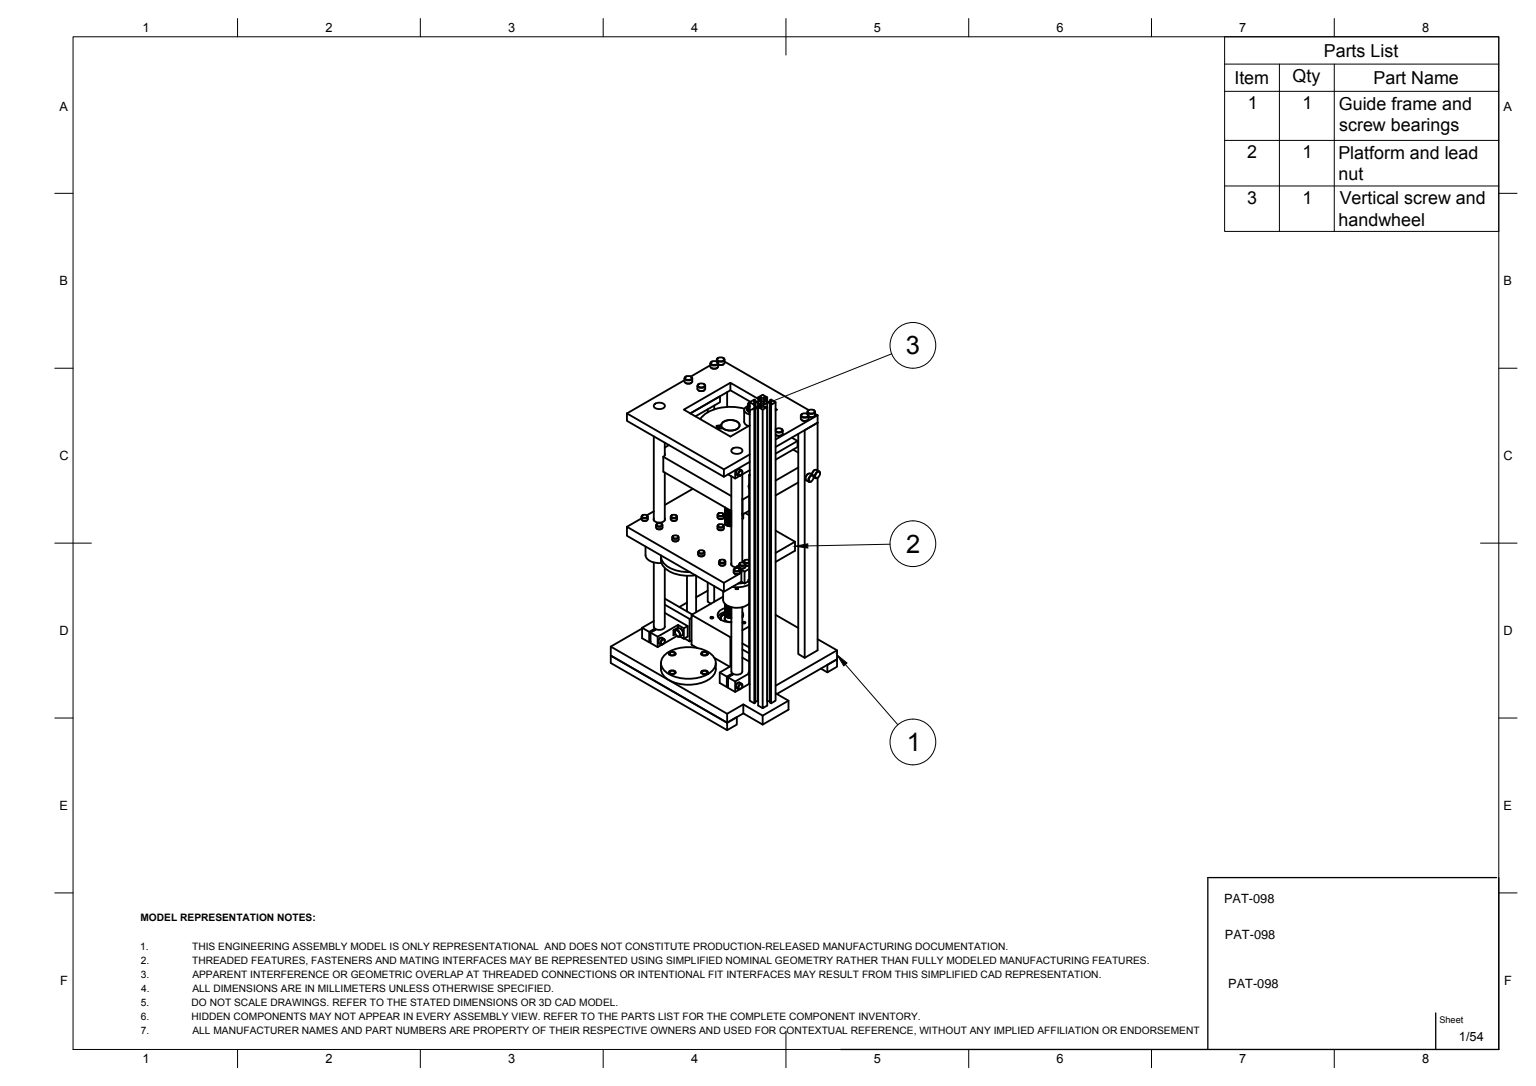
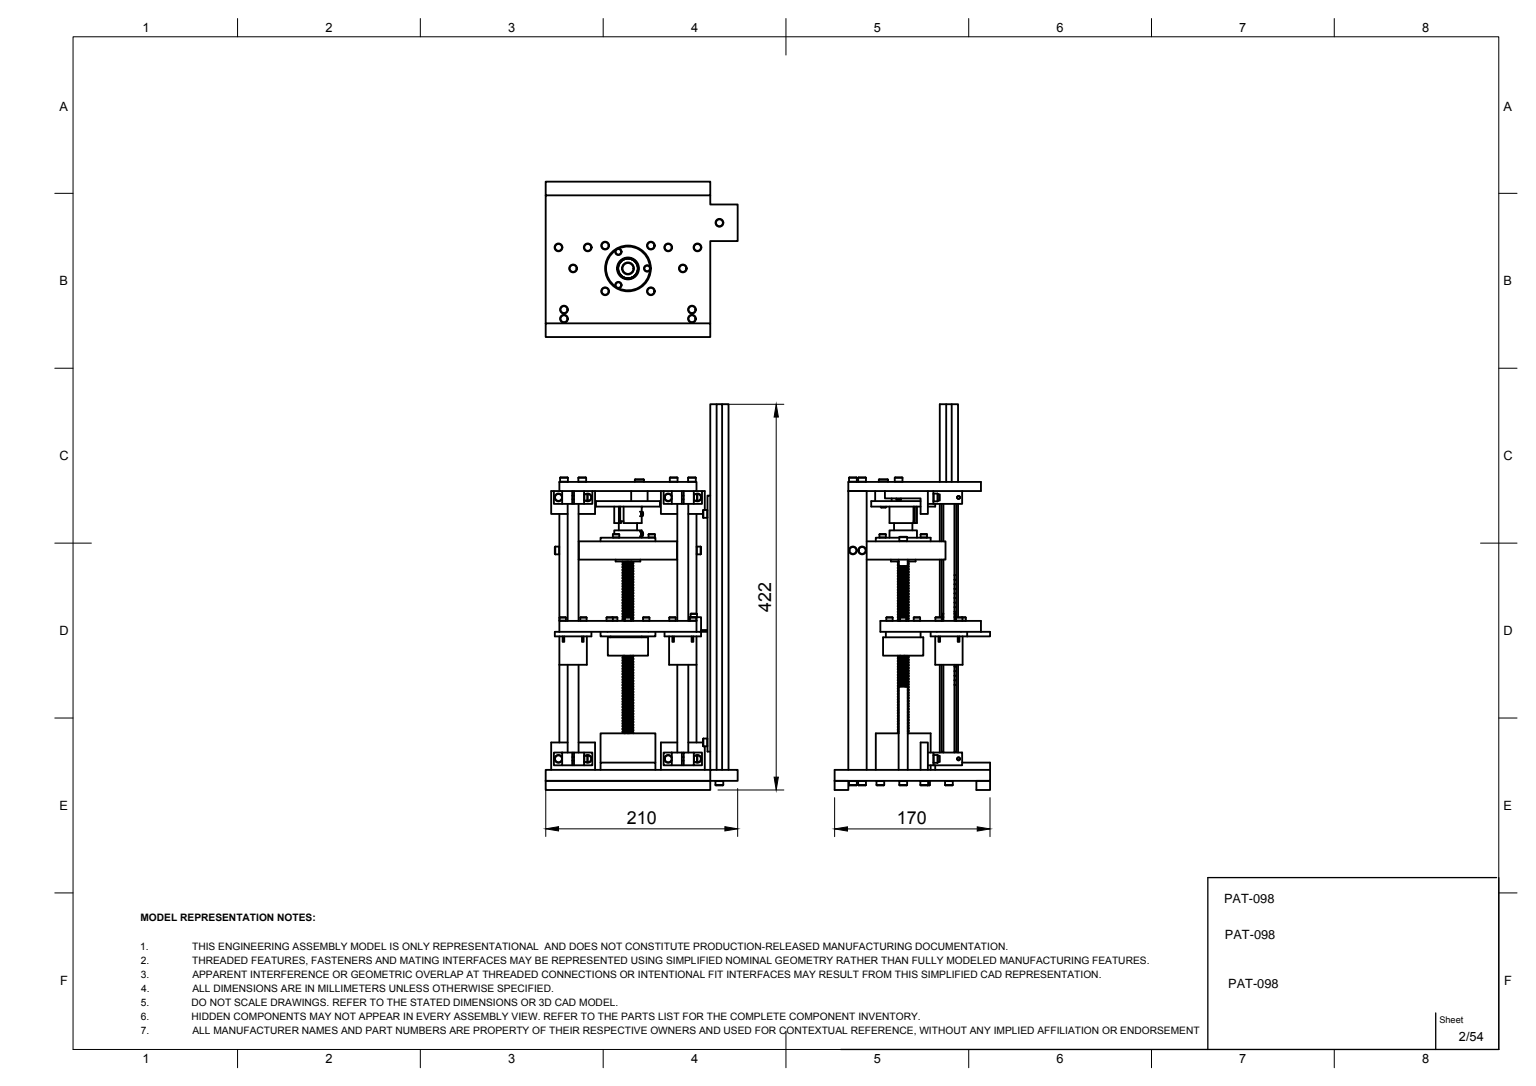
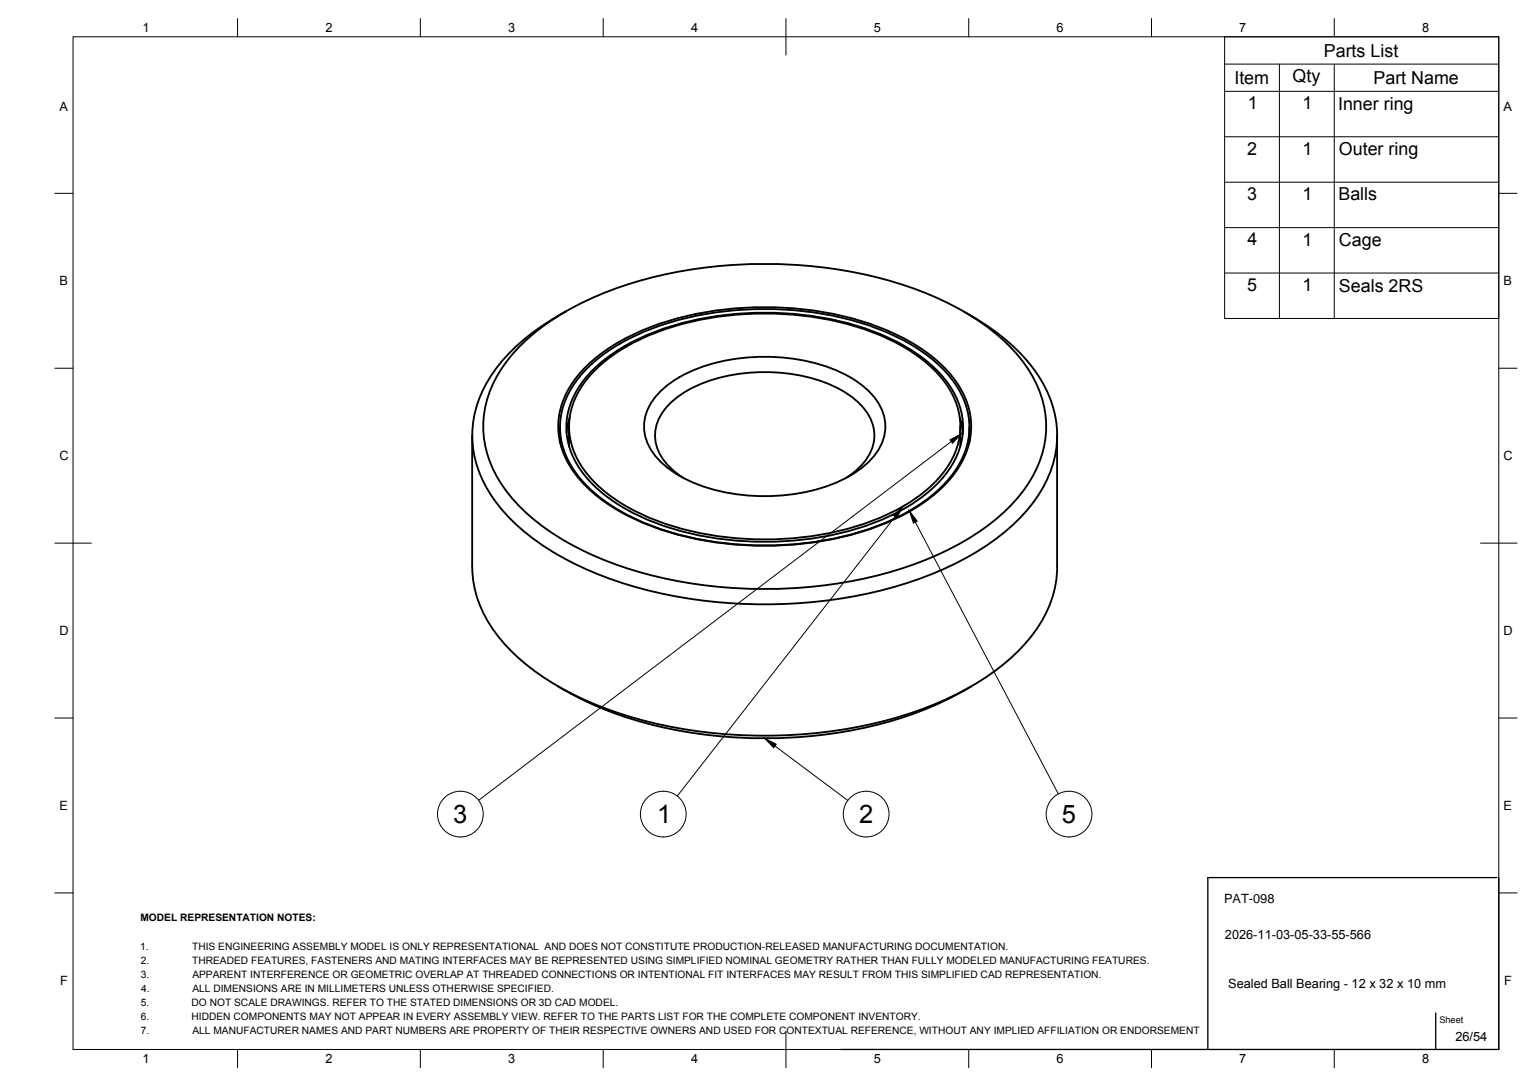
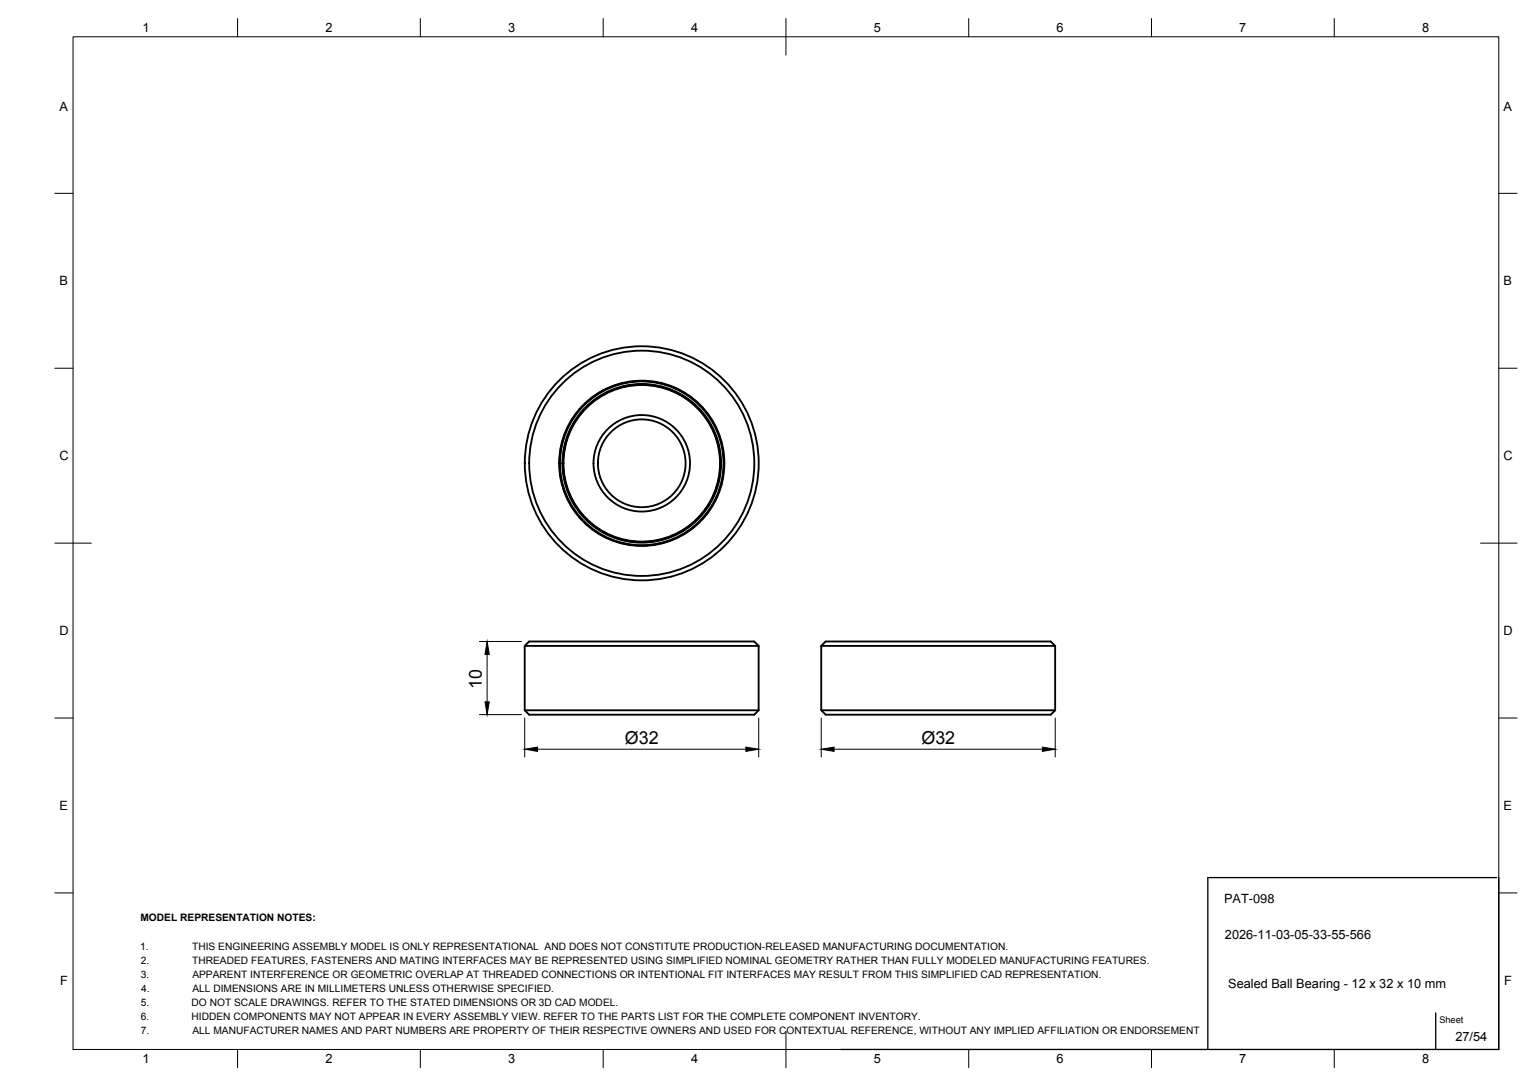
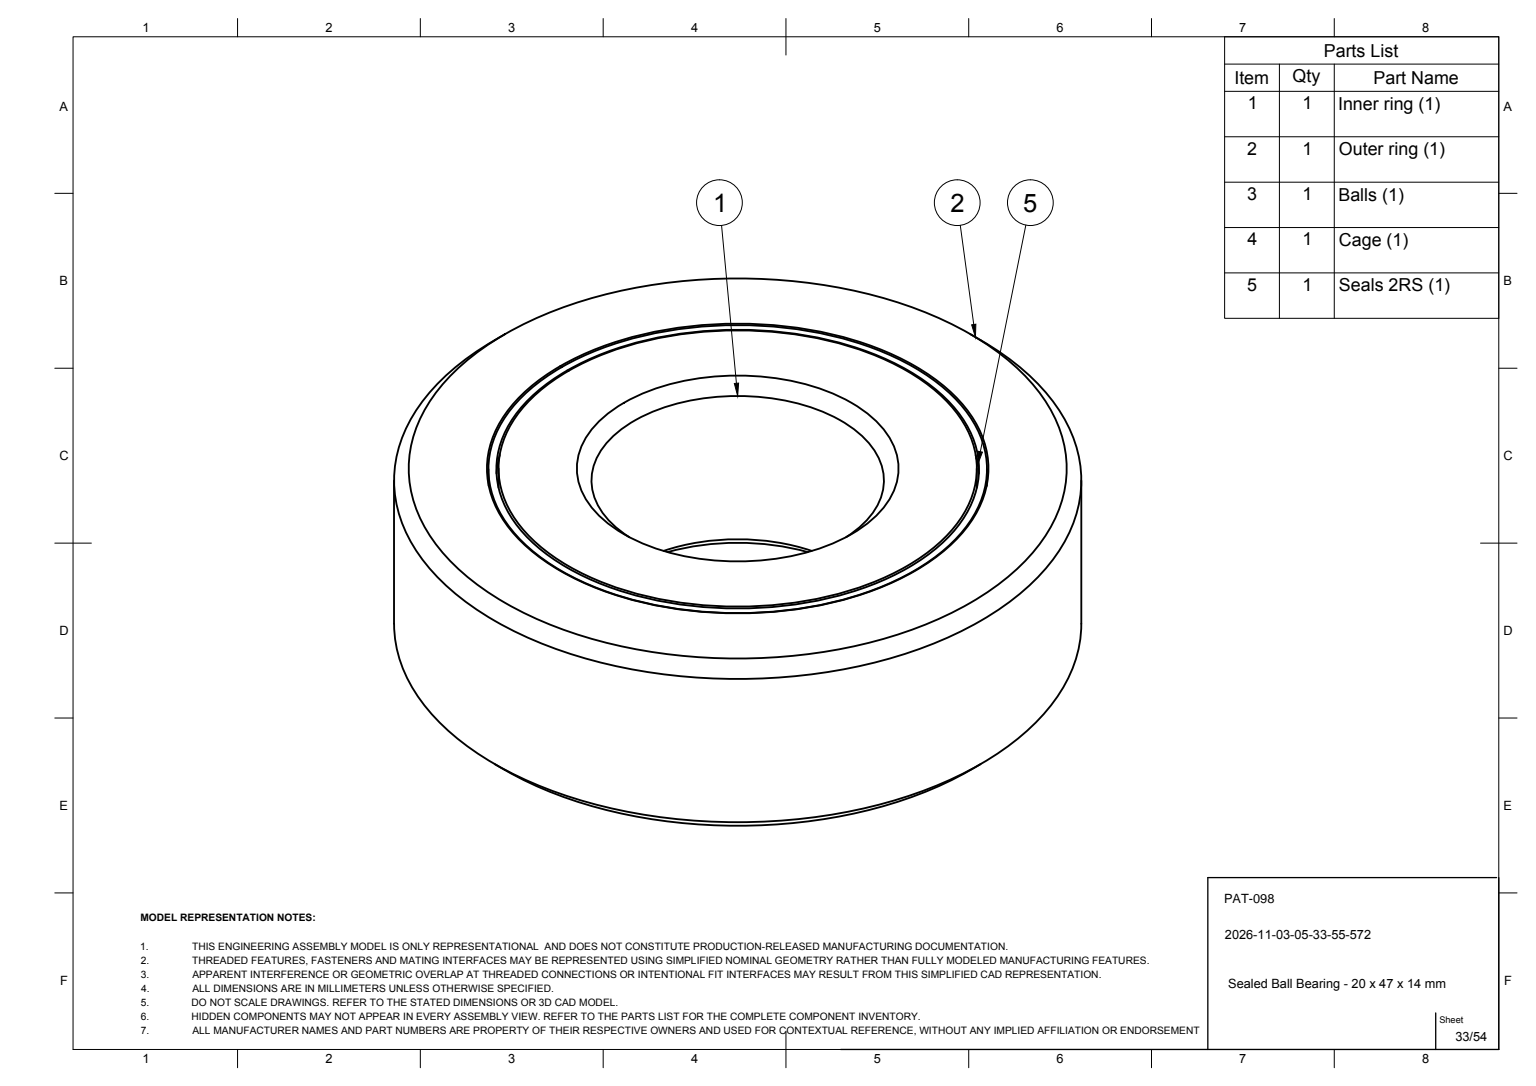
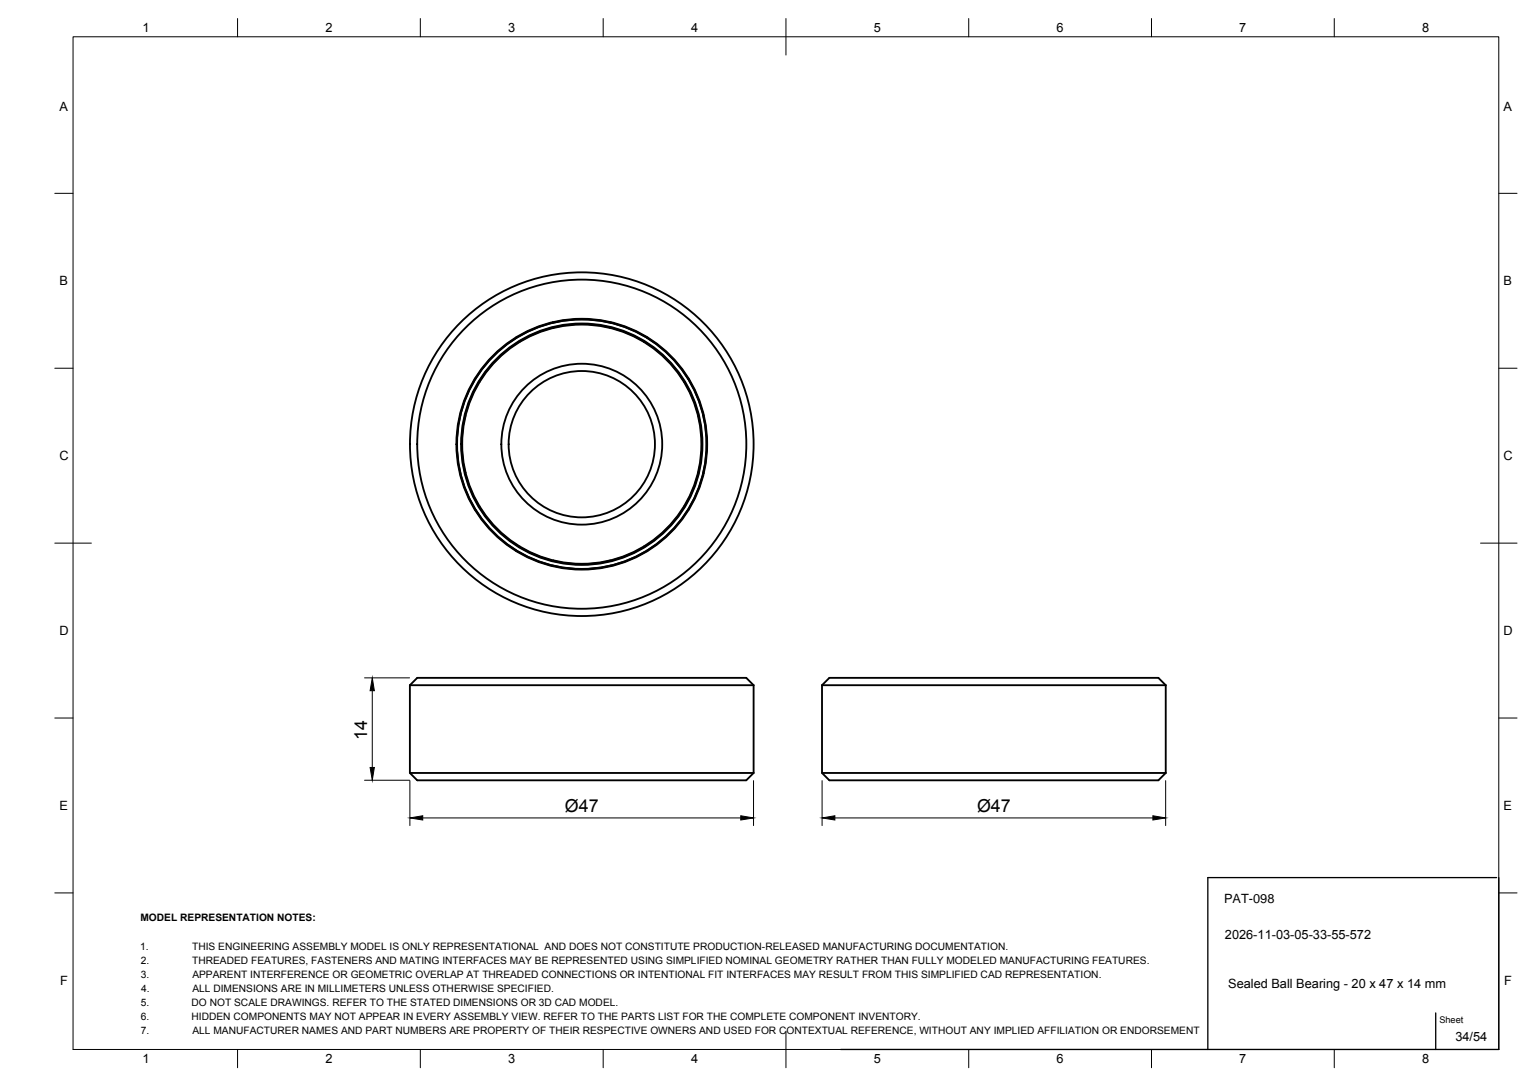
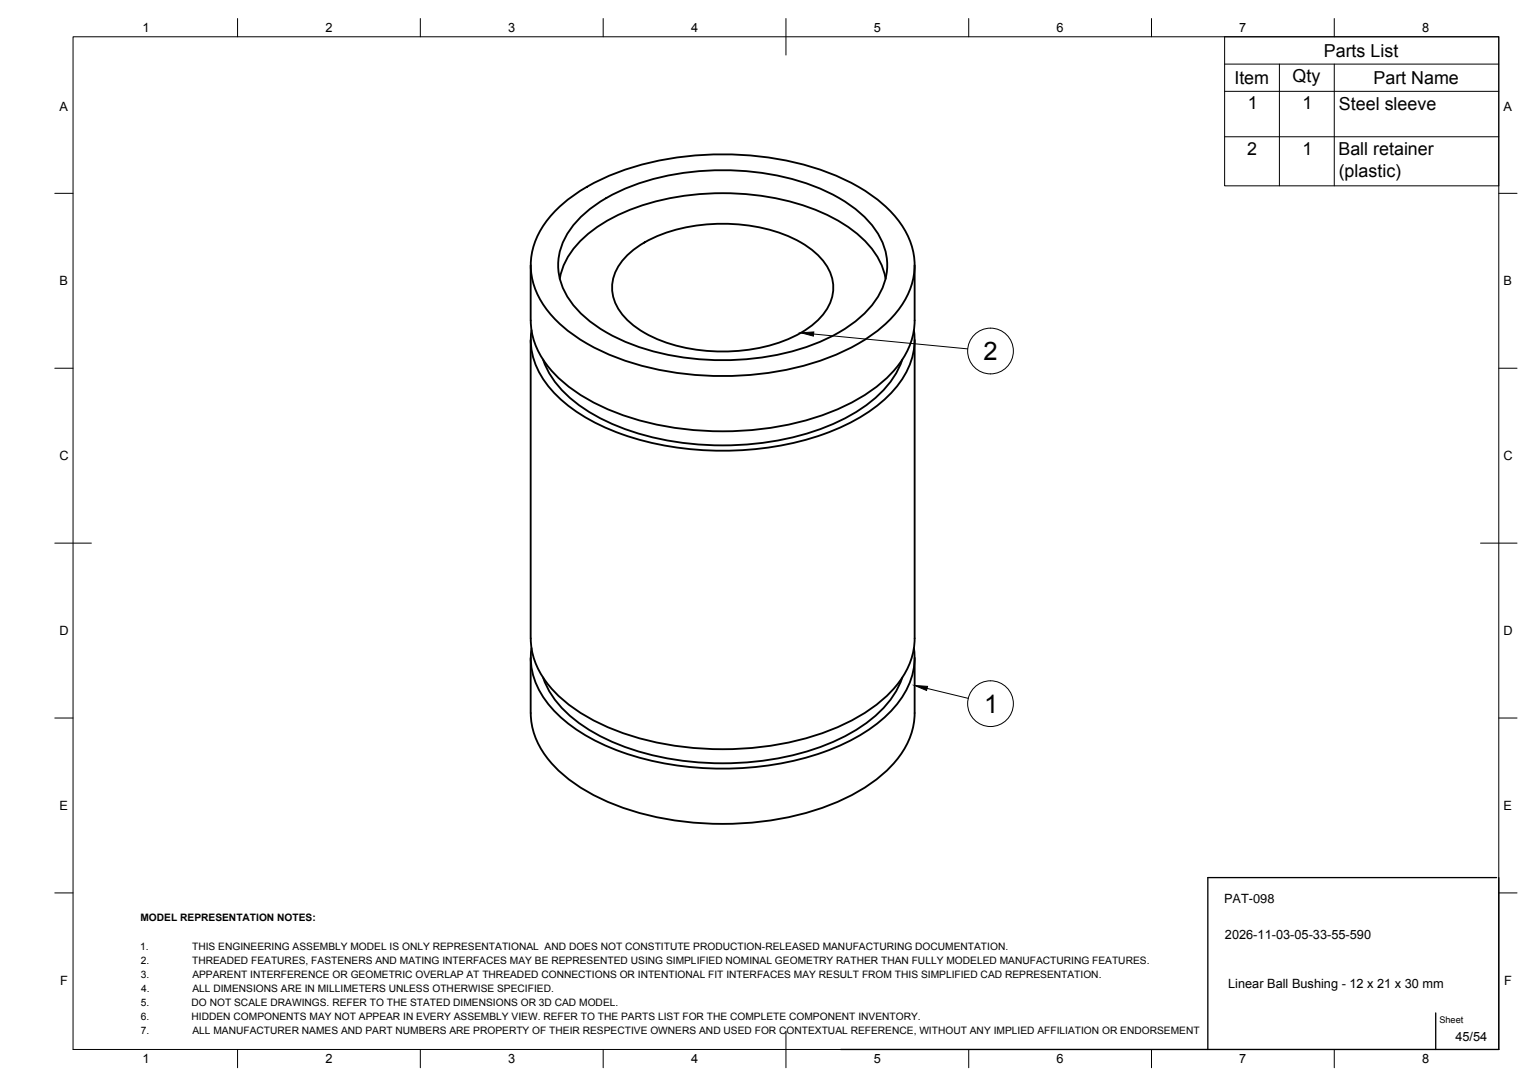
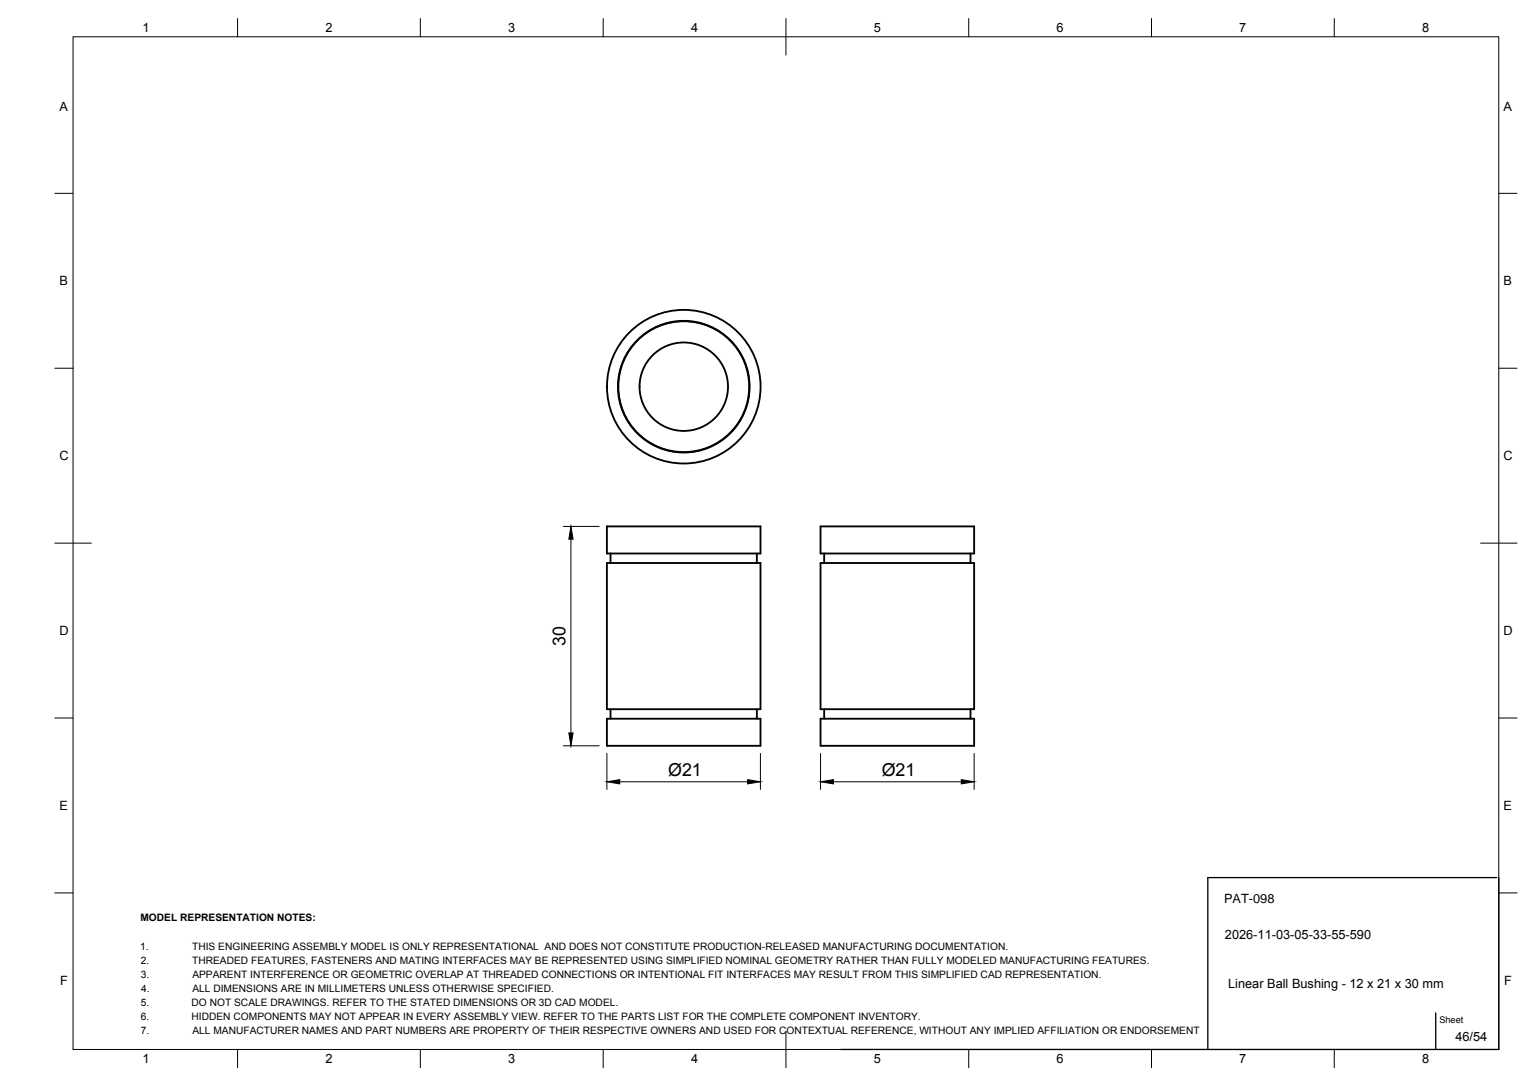
ISO-10303-21;
HEADER;
/* Generated by software containing ST-Developer
 * from STEP Tools, Inc. (www.steptools.com) 
 */

FILE_DESCRIPTION(
/* description */ ('Spring compression tester'),
/* implementation_level */ '2;1');

FILE_NAME(
/* name */ 'PAT-098',
/* time_stamp */ '2026-10-28T03:24:11-07:00',
/* author */ (''),
/* organization */ (''),
/* preprocessor_version */ 'ST-DEVELOPER v20.2',
/* originating_system */ 'Autodesk Translation Framework v15.17.0.0',
/* authorisation */ '');

FILE_SCHEMA (('AUTOMOTIVE_DESIGN { 1 0 10303 214 3 1 1 }'));
ENDSEC;

DATA;
#10=MECHANICAL_DESIGN_GEOMETRIC_PRESENTATION_REPRESENTATION('',(#1104,#1105,
#1106,#1107,#1108,#1109,#1110,#1111,#1112,#1113,#1114,#1115,#1116,#1117,
#1118,#1119,#1120,#1121,#1122,#1123,#1124,#1125,#1126,#1127,#1128,#1129,
#1130,#1131,#1132,#1133,#1134,#1135,#1136,#1137,#1138,#1139,#1140,#1141,
#1142,#1143,#1144,#1145,#1146,#1147,#1148,#1149,#1150,#1151,#1152,#1153,
#1154,#1155,#1156,#1157,#1158,#1159,#1160,#1161,#1162,#1163,#1164,#1165,
#1166,#1167,#1168,#1169,#1170,#1171,#1172,#1173,#1174,#1175,#1176,#1177,
#1178),#43521);
#11=B_SPLINE_SURFACE_WITH_KNOTS('',3,3,((#31855,#31856,#31857,#31858,#31859,
#31860,#31861,#31862,#31863,#31864,#31865,#31866,#31867,#31868,#31869,#31870,
#31871,#31872,#31873,#31874,#31875,#31876,#31877,#31878,#31879,#31880,#31881,
#31882,#31883,#31884,#31885,#31886,#31887,#31888,#31889,#31890,#31891,#31892,
#31893,#31894,#31895,#31896,#31897,#31898,#31899,#31900,#31901,#31902,#31903,
#31904,#31905,#31906,#31907,#31908,#31909,#31910,#31911,#31912,#31913,#31914,
#31915,#31916,#31917,#31918,#31919,#31920,#31921,#31922,#31923,#31924,#31925,
#31926,#31927,#31928,#31929,#31930,#31931,#31932,#31933,#31934,#31935,#31936,
#31937,#31938,#31939,#31940,#31941,#31942,#31943,#31944,#31945,#31946,#31947,
#31948,#31949,#31950,#31951,#31952,#31953,#31954,#31955,#31956,#31957,#31958,
#31959,#31960,#31961,#31962,#31963,#31964,#31965,#31966,#31967,#31968,#31969),
(#31970,#31971,#31972,#31973,#31974,#31975,#31976,#31977,#31978,#31979,
#31980,#31981,#31982,#31983,#31984,#31985,#31986,#31987,#31988,#31989,#31990,
#31991,#31992,#31993,#31994,#31995,#31996,#31997,#31998,#31999,#32000,#32001,
#32002,#32003,#32004,#32005,#32006,#32007,#32008,#32009,#32010,#32011,#32012,
#32013,#32014,#32015,#32016,#32017,#32018,#32019,#32020,#32021,#32022,#32023,
#32024,#32025,#32026,#32027,#32028,#32029,#32030,#32031,#32032,#32033,#32034,
#32035,#32036,#32037,#32038,#32039,#32040,#32041,#32042,#32043,#32044,#32045,
#32046,#32047,#32048,#32049,#32050,#32051,#32052,#32053,#32054,#32055,#32056,
#32057,#32058,#32059,#32060,#32061,#32062,#32063,#32064,#32065,#32066,#32067,
#32068,#32069,#32070,#32071,#32072,#32073,#32074,#32075,#32076,#32077,#32078,
#32079,#32080,#32081,#32082,#32083,#32084),(#32085,#32086,#32087,#32088,
#32089,#32090,#32091,#32092,#32093,#32094,#32095,#32096,#32097,#32098,#32099,
#32100,#32101,#32102,#32103,#32104,#32105,#32106,#32107,#32108,#32109,#32110,
#32111,#32112,#32113,#32114,#32115,#32116,#32117,#32118,#32119,#32120,#32121,
#32122,#32123,#32124,#32125,#32126,#32127,#32128,#32129,#32130,#32131,#32132,
#32133,#32134,#32135,#32136,#32137,#32138,#32139,#32140,#32141,#32142,#32143,
#32144,#32145,#32146,#32147,#32148,#32149,#32150,#32151,#32152,#32153,#32154,
#32155,#32156,#32157,#32158,#32159,#32160,#32161,#32162,#32163,#32164,#32165,
#32166,#32167,#32168,#32169,#32170,#32171,#32172,#32173,#32174,#32175,#32176,
#32177,#32178,#32179,#32180,#32181,#32182,#32183,#32184,#32185,#32186,#32187,
#32188,#32189,#32190,#32191,#32192,#32193,#32194,#32195,#32196,#32197,#32198,
#32199),(#32200,#32201,#32202,#32203,#32204,#32205,#32206,#32207,#32208,
#32209,#32210,#32211,#32212,#32213,#32214,#32215,#32216,#32217,#32218,#32219,
#32220,#32221,#32222,#32223,#32224,#32225,#32226,#32227,#32228,#32229,#32230,
#32231,#32232,#32233,#32234,#32235,#32236,#32237,#32238,#32239,#32240,#32241,
#32242,#32243,#32244,#32245,#32246,#32247,#32248,#32249,#32250,#32251,#32252,
#32253,#32254,#32255,#32256,#32257,#32258,#32259,#32260,#32261,#32262,#32263,
#32264,#32265,#32266,#32267,#32268,#32269,#32270,#32271,#32272,#32273,#32274,
#32275,#32276,#32277,#32278,#32279,#32280,#32281,#32282,#32283,#32284,#32285,
#32286,#32287,#32288,#32289,#32290,#32291,#32292,#32293,#32294,#32295,#32296,
#32297,#32298,#32299,#32300,#32301,#32302,#32303,#32304,#32305,#32306,#32307,
#32308,#32309,#32310,#32311,#32312,#32313,#32314)),.UNSPECIFIED.,.F.,.F.,
 .F.,(4,4),(4,1,1,1,1,1,1,1,1,1,1,1,1,1,1,1,1,1,1,1,1,1,1,1,1,1,1,1,1,1,
1,1,1,1,1,1,1,1,1,1,1,1,1,1,1,1,1,1,1,1,1,1,1,1,1,1,1,1,1,1,1,1,1,1,1,1,
1,1,1,1,1,1,1,1,1,1,1,1,1,1,1,1,1,1,1,1,1,1,1,1,1,1,1,1,1,1,1,1,1,1,1,1,
1,1,1,1,1,1,1,1,1,1,4),(0.,0.173020531651036),(12.1475814751569,12.6421543672732,
13.1367272593894,13.6313001515056,14.1258730436219,14.6204459357381,15.1150188278544,
15.6095917199706,16.1041646120869,16.5987375042031,17.0933103963194,17.5878832884356,
18.0824561805519,18.5770290726681,19.0716019647843,19.5661748569006,20.0607477490168,
20.5553206411331,21.0498935332493,21.5444664253656,22.0390393174818,22.5336122095981,
23.0281851017143,23.5227579938306,24.0173308859468,24.511903778063,25.0064766701793,
25.5010495622955,25.9956224544118,26.490195346528,26.9847682386443,27.4793411307605,
27.9739140228768,28.468486914993,28.9630598071093,29.4576326992255,29.9522055913417,
30.446778483458,30.9413513755742,31.4359242676905,31.9304971598067,32.425070051923,
32.9196429440392,33.4142158361555,33.9087887282717,34.403361620388,34.8979345125042,
35.3925074046204,35.8870802967367,36.3816531888529,36.8762260809692,37.3707989730854,
37.8653718652017,38.3599447573179,38.8545176494342,39.3490905415504,39.8436634336667,
40.3382363257829,40.8328092178991,41.3273821100154,41.8219550021316,42.3165278942479,
42.8111007863641,43.3056736784804,43.8002465705966,44.2948194627129,44.7893923548291,
45.2839652469454,45.7785381390616,46.2731110311778,46.7676839232941,47.2622568154103,
47.7568297075266,48.2514025996428,48.7459754917591,49.2405483838753,49.7351212759916,
50.2296941681078,50.7242670602241,51.2188399523403,51.7134128444565,52.2079857365728,
52.702558628689,53.1971315208053,53.6917044129215,54.1862773050378,54.680850197154,
55.1754230892703,55.6699959813865,56.1645688735028,56.659141765619,57.1537146577353,
57.6482875498515,58.1428604419677,58.637433334084,59.1320062262002,59.6265791183165,
60.1211520104327,60.615724902549,61.1102977946652,61.6048706867815,62.0994435788977,
62.5940164710139,63.0885893631302,63.5831622552464,64.0777351473627,64.5723080394789,
65.0668809315952,65.5614538237114,66.0560267158277,66.5505996079439,67.0451725000601,
67.5397453921764),.UNSPECIFIED.);
#12=B_SPLINE_SURFACE_WITH_KNOTS('',3,3,((#32414,#32415,#32416,#32417,#32418,
#32419,#32420,#32421,#32422,#32423,#32424,#32425,#32426,#32427,#32428,#32429,
#32430,#32431,#32432,#32433,#32434,#32435,#32436,#32437,#32438,#32439,#32440,
#32441,#32442,#32443,#32444,#32445,#32446,#32447,#32448,#32449,#32450,#32451,
#32452,#32453,#32454,#32455,#32456,#32457,#32458,#32459,#32460,#32461,#32462,
#32463,#32464,#32465,#32466,#32467,#32468,#32469,#32470,#32471,#32472,#32473,
#32474,#32475,#32476,#32477,#32478,#32479,#32480,#32481,#32482,#32483,#32484,
#32485,#32486,#32487,#32488,#32489,#32490,#32491,#32492,#32493,#32494,#32495,
#32496,#32497,#32498,#32499,#32500,#32501,#32502,#32503,#32504,#32505,#32506,
#32507,#32508,#32509,#32510,#32511,#32512,#32513,#32514,#32515,#32516,#32517,
#32518,#32519,#32520,#32521,#32522,#32523,#32524,#32525,#32526,#32527,#32528),
(#32529,#32530,#32531,#32532,#32533,#32534,#32535,#32536,#32537,#32538,
#32539,#32540,#32541,#32542,#32543,#32544,#32545,#32546,#32547,#32548,#32549,
#32550,#32551,#32552,#32553,#32554,#32555,#32556,#32557,#32558,#32559,#32560,
#32561,#32562,#32563,#32564,#32565,#32566,#32567,#32568,#32569,#32570,#32571,
#32572,#32573,#32574,#32575,#32576,#32577,#32578,#32579,#32580,#32581,#32582,
#32583,#32584,#32585,#32586,#32587,#32588,#32589,#32590,#32591,#32592,#32593,
#32594,#32595,#32596,#32597,#32598,#32599,#32600,#32601,#32602,#32603,#32604,
#32605,#32606,#32607,#32608,#32609,#32610,#32611,#32612,#32613,#32614,#32615,
#32616,#32617,#32618,#32619,#32620,#32621,#32622,#32623,#32624,#32625,#32626,
#32627,#32628,#32629,#32630,#32631,#32632,#32633,#32634,#32635,#32636,#32637,
#32638,#32639,#32640,#32641,#32642,#32643),(#32644,#32645,#32646,#32647,
#32648,#32649,#32650,#32651,#32652,#32653,#32654,#32655,#32656,#32657,#32658,
#32659,#32660,#32661,#32662,#32663,#32664,#32665,#32666,#32667,#32668,#32669,
#32670,#32671,#32672,#32673,#32674,#32675,#32676,#32677,#32678,#32679,#32680,
#32681,#32682,#32683,#32684,#32685,#32686,#32687,#32688,#32689,#32690,#32691,
#32692,#32693,#32694,#32695,#32696,#32697,#32698,#32699,#32700,#32701,#32702,
#32703,#32704,#32705,#32706,#32707,#32708,#32709,#32710,#32711,#32712,#32713,
#32714,#32715,#32716,#32717,#32718,#32719,#32720,#32721,#32722,#32723,#32724,
#32725,#32726,#32727,#32728,#32729,#32730,#32731,#32732,#32733,#32734,#32735,
#32736,#32737,#32738,#32739,#32740,#32741,#32742,#32743,#32744,#32745,#32746,
#32747,#32748,#32749,#32750,#32751,#32752,#32753,#32754,#32755,#32756,#32757,
#32758),(#32759,#32760,#32761,#32762,#32763,#32764,#32765,#32766,#32767,
#32768,#32769,#32770,#32771,#32772,#32773,#32774,#32775,#32776,#32777,#32778,
#32779,#32780,#32781,#32782,#32783,#32784,#32785,#32786,#32787,#32788,#32789,
#32790,#32791,#32792,#32793,#32794,#32795,#32796,#32797,#32798,#32799,#32800,
#32801,#32802,#32803,#32804,#32805,#32806,#32807,#32808,#32809,#32810,#32811,
#32812,#32813,#32814,#32815,#32816,#32817,#32818,#32819,#32820,#32821,#32822,
#32823,#32824,#32825,#32826,#32827,#32828,#32829,#32830,#32831,#32832,#32833,
#32834,#32835,#32836,#32837,#32838,#32839,#32840,#32841,#32842,#32843,#32844,
#32845,#32846,#32847,#32848,#32849,#32850,#32851,#32852,#32853,#32854,#32855,
#32856,#32857,#32858,#32859,#32860,#32861,#32862,#32863,#32864,#32865,#32866,
#32867,#32868,#32869,#32870,#32871,#32872,#32873)),.UNSPECIFIED.,.F.,.F.,
 .F.,(4,4),(4,1,1,1,1,1,1,1,1,1,1,1,1,1,1,1,1,1,1,1,1,1,1,1,1,1,1,1,1,1,
1,1,1,1,1,1,1,1,1,1,1,1,1,1,1,1,1,1,1,1,1,1,1,1,1,1,1,1,1,1,1,1,1,1,1,1,
1,1,1,1,1,1,1,1,1,1,1,1,1,1,1,1,1,1,1,1,1,1,1,1,1,1,1,1,1,1,1,1,1,1,1,1,
1,1,1,1,1,1,1,1,1,1,4),(0.,0.173020531651036),(15.1888611523549,15.6834340444711,
16.1780069365874,16.6725798287036,17.1671527208199,17.6617256129361,18.1562985050523,
18.6508713971686,19.1454442892848,19.6400171814011,20.1345900735173,20.6291629656336,
21.1237358577498,21.6183087498661,22.1128816419823,22.6074545340986,23.1020274262148,
23.596600318331,24.0911732104473,24.5857461025635,25.0803189946798,25.574891886796,
26.0694647789123,26.5640376710285,27.0586105631448,27.553183455261,28.0477563473773,
28.5423292394935,29.0369021316097,29.531475023726,30.0260479158422,30.5206208079585,
31.0151937000747,31.509766592191,32.0043394843072,32.4989123764235,32.9934852685397,
33.488058160656,33.9826310527722,34.4772039448884,34.9717768370047,35.4663497291209,
35.9609226212372,36.4554955133534,36.9500684054697,37.4446412975859,37.9392141897022,
38.4337870818184,38.9283599739347,39.4229328660509,39.9175057581671,40.4120786502834,
40.9066515423996,41.4012244345159,41.8957973266321,42.3903702187484,42.8849431108646,
43.3795160029809,43.8740888950971,44.3686617872134,44.8632346793296,45.3578075714458,
45.8523804635621,46.3469533556783,46.8415262477946,47.3360991399108,47.8306720320271,
48.3252449241433,48.8198178162596,49.3143907083758,49.8089636004921,50.3035364926083,
50.7981093847245,51.2926822768408,51.787255168957,52.2818280610733,52.7764009531895,
53.2709738453058,53.765546737422,54.2601196295383,54.7546925216545,55.2492654137708,
55.743838305887,56.2384111980032,56.7329840901195,57.2275569822357,57.722129874352,
58.2167027664682,58.7112756585845,59.2058485507007,59.700421442817,60.1949943349332,
60.6895672270495,61.1841401191657,61.6787130112819,62.1732859033982,62.6678587955144,
63.1624316876307,63.6570045797469,64.1515774718632,64.6461503639794,65.1407232560957,
65.6352961482119,66.1298690403281,66.6244419324444,67.1190148245607,67.6135877166769,
68.1081606087931,68.6027335009094,69.0973063930256,69.5918792851419,70.0864521772581,
70.5810250693744),.UNSPECIFIED.);
#13=B_SPLINE_SURFACE_WITH_KNOTS('',3,3,((#38747,#38748,#38749,#38750,#38751,
#38752,#38753,#38754,#38755,#38756,#38757,#38758,#38759,#38760,#38761,#38762,
#38763,#38764,#38765,#38766,#38767,#38768,#38769,#38770,#38771,#38772,#38773,
#38774,#38775,#38776,#38777,#38778,#38779,#38780,#38781,#38782,#38783,#38784,
#38785,#38786,#38787,#38788,#38789,#38790,#38791,#38792,#38793,#38794,#38795,
#38796,#38797,#38798,#38799,#38800,#38801,#38802,#38803,#38804,#38805,#38806,
#38807,#38808,#38809,#38810,#38811,#38812,#38813,#38814,#38815,#38816,#38817,
#38818,#38819,#38820,#38821,#38822,#38823,#38824,#38825,#38826,#38827,#38828,
#38829,#38830,#38831,#38832,#38833,#38834,#38835,#38836,#38837,#38838,#38839,
#38840,#38841,#38842,#38843,#38844,#38845,#38846,#38847,#38848,#38849,#38850,
#38851,#38852,#38853,#38854,#38855,#38856,#38857,#38858,#38859,#38860,#38861,
#38862,#38863,#38864,#38865,#38866,#38867,#38868,#38869,#38870,#38871,#38872,
#38873,#38874,#38875,#38876,#38877,#38878,#38879,#38880,#38881,#38882,#38883,
#38884,#38885,#38886,#38887,#38888,#38889,#38890,#38891,#38892,#38893,#38894,
#38895,#38896,#38897,#38898,#38899,#38900,#38901,#38902,#38903,#38904,#38905,
#38906,#38907,#38908,#38909,#38910,#38911,#38912,#38913,#38914,#38915,#38916,
#38917,#38918,#38919,#38920,#38921,#38922,#38923,#38924,#38925,#38926,#38927,
#38928,#38929,#38930,#38931,#38932,#38933,#38934,#38935,#38936,#38937,#38938,
#38939,#38940,#38941,#38942,#38943,#38944,#38945,#38946,#38947,#38948,#38949,
#38950,#38951,#38952,#38953,#38954,#38955,#38956,#38957,#38958,#38959,#38960,
#38961,#38962,#38963,#38964,#38965,#38966,#38967,#38968,#38969,#38970,#38971,
#38972,#38973,#38974,#38975,#38976,#38977,#38978,#38979,#38980,#38981,#38982,
#38983,#38984,#38985,#38986,#38987,#38988,#38989,#38990,#38991,#38992,#38993,
#38994,#38995,#38996,#38997,#38998,#38999,#39000,#39001,#39002,#39003,#39004,
#39005,#39006,#39007,#39008,#39009,#39010,#39011,#39012,#39013,#39014,#39015,
#39016,#39017,#39018,#39019,#39020,#39021,#39022,#39023,#39024,#39025,#39026,
#39027,#39028,#39029,#39030,#39031,#39032,#39033,#39034,#39035,#39036,#39037,
#39038,#39039,#39040,#39041,#39042,#39043,#39044,#39045,#39046,#39047,#39048,
#39049,#39050,#39051,#39052,#39053,#39054,#39055,#39056,#39057,#39058,#39059,
#39060,#39061,#39062,#39063,#39064,#39065,#39066,#39067,#39068,#39069,#39070,
#39071,#39072,#39073,#39074,#39075,#39076,#39077,#39078,#39079,#39080,#39081,
#39082,#39083,#39084,#39085,#39086,#39087,#39088,#39089,#39090,#39091,#39092,
#39093,#39094,#39095,#39096,#39097,#39098,#39099,#39100,#39101,#39102,#39103,
#39104,#39105,#39106,#39107,#39108,#39109,#39110,#39111,#39112,#39113,#39114,
#39115,#39116,#39117,#39118,#39119,#39120,#39121,#39122,#39123,#39124,#39125,
#39126,#39127,#39128,#39129,#39130,#39131,#39132,#39133,#39134,#39135,#39136,
#39137,#39138,#39139,#39140,#39141,#39142,#39143,#39144,#39145,#39146,#39147,
#39148,#39149,#39150,#39151,#39152,#39153,#39154,#39155,#39156,#39157,#39158,
#39159,#39160,#39161,#39162,#39163,#39164,#39165,#39166,#39167,#39168,#39169,
#39170,#39171,#39172,#39173,#39174,#39175,#39176,#39177,#39178,#39179,#39180,
#39181,#39182,#39183,#39184,#39185,#39186,#39187,#39188,#39189,#39190,#39191,
#39192,#39193,#39194,#39195,#39196,#39197,#39198,#39199,#39200,#39201,#39202,
#39203,#39204,#39205,#39206,#39207,#39208,#39209,#39210,#39211,#39212,#39213,
#39214,#39215,#39216,#39217,#39218,#39219,#39220,#39221,#39222,#39223,#39224,
#39225,#39226,#39227,#39228,#39229,#39230,#39231,#39232,#39233,#39234,#39235,
#39236,#39237,#39238,#39239,#39240,#39241,#39242,#39243,#39244),(#39245,
#39246,#39247,#39248,#39249,#39250,#39251,#39252,#39253,#39254,#39255,#39256,
#39257,#39258,#39259,#39260,#39261,#39262,#39263,#39264,#39265,#39266,#39267,
#39268,#39269,#39270,#39271,#39272,#39273,#39274,#39275,#39276,#39277,#39278,
#39279,#39280,#39281,#39282,#39283,#39284,#39285,#39286,#39287,#39288,#39289,
#39290,#39291,#39292,#39293,#39294,#39295,#39296,#39297,#39298,#39299,#39300,
#39301,#39302,#39303,#39304,#39305,#39306,#39307,#39308,#39309,#39310,#39311,
#39312,#39313,#39314,#39315,#39316,#39317,#39318,#39319,#39320,#39321,#39322,
#39323,#39324,#39325,#39326,#39327,#39328,#39329,#39330,#39331,#39332,#39333,
#39334,#39335,#39336,#39337,#39338,#39339,#39340,#39341,#39342,#39343,#39344,
#39345,#39346,#39347,#39348,#39349,#39350,#39351,#39352,#39353,#39354,#39355,
#39356,#39357,#39358,#39359,#39360,#39361,#39362,#39363,#39364,#39365,#39366,
#39367,#39368,#39369,#39370,#39371,#39372,#39373,#39374,#39375,#39376,#39377,
#39378,#39379,#39380,#39381,#39382,#39383,#39384,#39385,#39386,#39387,#39388,
#39389,#39390,#39391,#39392,#39393,#39394,#39395,#39396,#39397,#39398,#39399,
#39400,#39401,#39402,#39403,#39404,#39405,#39406,#39407,#39408,#39409,#39410,
#39411,#39412,#39413,#39414,#39415,#39416,#39417,#39418,#39419,#39420,#39421,
#39422,#39423,#39424,#39425,#39426,#39427,#39428,#39429,#39430,#39431,#39432,
#39433,#39434,#39435,#39436,#39437,#39438,#39439,#39440,#39441,#39442,#39443,
#39444,#39445,#39446,#39447,#39448,#39449,#39450,#39451,#39452,#39453,#39454,
#39455,#39456,#39457,#39458,#39459,#39460,#39461,#39462,#39463,#39464,#39465,
#39466,#39467,#39468,#39469,#39470,#39471,#39472,#39473,#39474,#39475,#39476,
#39477,#39478,#39479,#39480,#39481,#39482,#39483,#39484,#39485,#39486,#39487,
#39488,#39489,#39490,#39491,#39492,#39493,#39494,#39495,#39496,#39497,#39498,
#39499,#39500,#39501,#39502,#39503,#39504,#39505,#39506,#39507,#39508,#39509,
#39510,#39511,#39512,#39513,#39514,#39515,#39516,#39517,#39518,#39519,#39520,
#39521,#39522,#39523,#39524,#39525,#39526,#39527,#39528,#39529,#39530,#39531,
#39532,#39533,#39534,#39535,#39536,#39537,#39538,#39539,#39540,#39541,#39542,
#39543,#39544,#39545,#39546,#39547,#39548,#39549,#39550,#39551,#39552,#39553,
#39554,#39555,#39556,#39557,#39558,#39559,#39560,#39561,#39562,#39563,#39564,
#39565,#39566,#39567,#39568,#39569,#39570,#39571,#39572,#39573,#39574,#39575,
#39576,#39577,#39578,#39579,#39580,#39581,#39582,#39583,#39584,#39585,#39586,
#39587,#39588,#39589,#39590,#39591,#39592,#39593,#39594,#39595,#39596,#39597,
#39598,#39599,#39600,#39601,#39602,#39603,#39604,#39605,#39606,#39607,#39608,
#39609,#39610,#39611,#39612,#39613,#39614,#39615,#39616,#39617,#39618,#39619,
#39620,#39621,#39622,#39623,#39624,#39625,#39626,#39627,#39628,#39629,#39630,
#39631,#39632,#39633,#39634,#39635,#39636,#39637,#39638,#39639,#39640,#39641,
#39642,#39643,#39644,#39645,#39646,#39647,#39648,#39649,#39650,#39651,#39652,
#39653,#39654,#39655,#39656,#39657,#39658,#39659,#39660,#39661,#39662,#39663,
#39664,#39665,#39666,#39667,#39668,#39669,#39670,#39671,#39672,#39673,#39674,
#39675,#39676,#39677,#39678,#39679,#39680,#39681,#39682,#39683,#39684,#39685,
#39686,#39687,#39688,#39689,#39690,#39691,#39692,#39693,#39694,#39695,#39696,
#39697,#39698,#39699,#39700,#39701,#39702,#39703,#39704,#39705,#39706,#39707,
#39708,#39709,#39710,#39711,#39712,#39713,#39714,#39715,#39716,#39717,#39718,
#39719,#39720,#39721,#39722,#39723,#39724,#39725,#39726,#39727,#39728,#39729,
#39730,#39731,#39732,#39733,#39734,#39735,#39736,#39737,#39738,#39739,#39740,
#39741,#39742),(#39743,#39744,#39745,#39746,#39747,#39748,#39749,#39750,
#39751,#39752,#39753,#39754,#39755,#39756,#39757,#39758,#39759,#39760,#39761,
#39762,#39763,#39764,#39765,#39766,#39767,#39768,#39769,#39770,#39771,#39772,
#39773,#39774,#39775,#39776,#39777,#39778,#39779,#39780,#39781,#39782,#39783,
#39784,#39785,#39786,#39787,#39788,#39789,#39790,#39791,#39792,#39793,#39794,
#39795,#39796,#39797,#39798,#39799,#39800,#39801,#39802,#39803,#39804,#39805,
#39806,#39807,#39808,#39809,#39810,#39811,#39812,#39813,#39814,#39815,#39816,
#39817,#39818,#39819,#39820,#39821,#39822,#39823,#39824,#39825,#39826,#39827,
#39828,#39829,#39830,#39831,#39832,#39833,#39834,#39835,#39836,#39837,#39838,
#39839,#39840,#39841,#39842,#39843,#39844,#39845,#39846,#39847,#39848,#39849,
#39850,#39851,#39852,#39853,#39854,#39855,#39856,#39857,#39858,#39859,#39860,
#39861,#39862,#39863,#39864,#39865,#39866,#39867,#39868,#39869,#39870,#39871,
#39872,#39873,#39874,#39875,#39876,#39877,#39878,#39879,#39880,#39881,#39882,
#39883,#39884,#39885,#39886,#39887,#39888,#39889,#39890,#39891,#39892,#39893,
#39894,#39895,#39896,#39897,#39898,#39899,#39900,#39901,#39902,#39903,#39904,
#39905,#39906,#39907,#39908,#39909,#39910,#39911,#39912,#39913,#39914,#39915,
#39916,#39917,#39918,#39919,#39920,#39921,#39922,#39923,#39924,#39925,#39926,
#39927,#39928,#39929,#39930,#39931,#39932,#39933,#39934,#39935,#39936,#39937,
#39938,#39939,#39940,#39941,#39942,#39943,#39944,#39945,#39946,#39947,#39948,
#39949,#39950,#39951,#39952,#39953,#39954,#39955,#39956,#39957,#39958,#39959,
#39960,#39961,#39962,#39963,#39964,#39965,#39966,#39967,#39968,#39969,#39970,
#39971,#39972,#39973,#39974,#39975,#39976,#39977,#39978,#39979,#39980,#39981,
#39982,#39983,#39984,#39985,#39986,#39987,#39988,#39989,#39990,#39991,#39992,
#39993,#39994,#39995,#39996,#39997,#39998,#39999,#40000,#40001,#40002,#40003,
#40004,#40005,#40006,#40007,#40008,#40009,#40010,#40011,#40012,#40013,#40014,
#40015,#40016,#40017,#40018,#40019,#40020,#40021,#40022,#40023,#40024,#40025,
#40026,#40027,#40028,#40029,#40030,#40031,#40032,#40033,#40034,#40035,#40036,
#40037,#40038,#40039,#40040,#40041,#40042,#40043,#40044,#40045,#40046,#40047,
#40048,#40049,#40050,#40051,#40052,#40053,#40054,#40055,#40056,#40057,#40058,
#40059,#40060,#40061,#40062,#40063,#40064,#40065,#40066,#40067,#40068,#40069,
#40070,#40071,#40072,#40073,#40074,#40075,#40076,#40077,#40078,#40079,#40080,
#40081,#40082,#40083,#40084,#40085,#40086,#40087,#40088,#40089,#40090,#40091,
#40092,#40093,#40094,#40095,#40096,#40097,#40098,#40099,#40100,#40101,#40102,
#40103,#40104,#40105,#40106,#40107,#40108,#40109,#40110,#40111,#40112,#40113,
#40114,#40115,#40116,#40117,#40118,#40119,#40120,#40121,#40122,#40123,#40124,
#40125,#40126,#40127,#40128,#40129,#40130,#40131,#40132,#40133,#40134,#40135,
#40136,#40137,#40138,#40139,#40140,#40141,#40142,#40143,#40144,#40145,#40146,
#40147,#40148,#40149,#40150,#40151,#40152,#40153,#40154,#40155,#40156,#40157,
#40158,#40159,#40160,#40161,#40162,#40163,#40164,#40165,#40166,#40167,#40168,
#40169,#40170,#40171,#40172,#40173,#40174,#40175,#40176,#40177,#40178,#40179,
#40180,#40181,#40182,#40183,#40184,#40185,#40186,#40187,#40188,#40189,#40190,
#40191,#40192,#40193,#40194,#40195,#40196,#40197,#40198,#40199,#40200,#40201,
#40202,#40203,#40204,#40205,#40206,#40207,#40208,#40209,#40210,#40211,#40212,
#40213,#40214,#40215,#40216,#40217,#40218,#40219,#40220,#40221,#40222,#40223,
#40224,#40225,#40226,#40227,#40228,#40229,#40230,#40231,#40232,#40233,#40234,
#40235,#40236,#40237,#40238,#40239,#40240),(#40241,#40242,#40243,#40244,
#40245,#40246,#40247,#40248,#40249,#40250,#40251,#40252,#40253,#40254,#40255,
#40256,#40257,#40258,#40259,#40260,#40261,#40262,#40263,#40264,#40265,#40266,
#40267,#40268,#40269,#40270,#40271,#40272,#40273,#40274,#40275,#40276,#40277,
#40278,#40279,#40280,#40281,#40282,#40283,#40284,#40285,#40286,#40287,#40288,
#40289,#40290,#40291,#40292,#40293,#40294,#40295,#40296,#40297,#40298,#40299,
#40300,#40301,#40302,#40303,#40304,#40305,#40306,#40307,#40308,#40309,#40310,
#40311,#40312,#40313,#40314,#40315,#40316,#40317,#40318,#40319,#40320,#40321,
#40322,#40323,#40324,#40325,#40326,#40327,#40328,#40329,#40330,#40331,#40332,
#40333,#40334,#40335,#40336,#40337,#40338,#40339,#40340,#40341,#40342,#40343,
#40344,#40345,#40346,#40347,#40348,#40349,#40350,#40351,#40352,#40353,#40354,
#40355,#40356,#40357,#40358,#40359,#40360,#40361,#40362,#40363,#40364,#40365,
#40366,#40367,#40368,#40369,#40370,#40371,#40372,#40373,#40374,#40375,#40376,
#40377,#40378,#40379,#40380,#40381,#40382,#40383,#40384,#40385,#40386,#40387,
#40388,#40389,#40390,#40391,#40392,#40393,#40394,#40395,#40396,#40397,#40398,
#40399,#40400,#40401,#40402,#40403,#40404,#40405,#40406,#40407,#40408,#40409,
#40410,#40411,#40412,#40413,#40414,#40415,#40416,#40417,#40418,#40419,#40420,
#40421,#40422,#40423,#40424,#40425,#40426,#40427,#40428,#40429,#40430,#40431,
#40432,#40433,#40434,#40435,#40436,#40437,#40438,#40439,#40440,#40441,#40442,
#40443,#40444,#40445,#40446,#40447,#40448,#40449,#40450,#40451,#40452,#40453,
#40454,#40455,#40456,#40457,#40458,#40459,#40460,#40461,#40462,#40463,#40464,
#40465,#40466,#40467,#40468,#40469,#40470,#40471,#40472,#40473,#40474,#40475,
#40476,#40477,#40478,#40479,#40480,#40481,#40482,#40483,#40484,#40485,#40486,
#40487,#40488,#40489,#40490,#40491,#40492,#40493,#40494,#40495,#40496,#40497,
#40498,#40499,#40500,#40501,#40502,#40503,#40504,#40505,#40506,#40507,#40508,
#40509,#40510,#40511,#40512,#40513,#40514,#40515,#40516,#40517,#40518,#40519,
#40520,#40521,#40522,#40523,#40524,#40525,#40526,#40527,#40528,#40529,#40530,
#40531,#40532,#40533,#40534,#40535,#40536,#40537,#40538,#40539,#40540,#40541,
#40542,#40543,#40544,#40545,#40546,#40547,#40548,#40549,#40550,#40551,#40552,
#40553,#40554,#40555,#40556,#40557,#40558,#40559,#40560,#40561,#40562,#40563,
#40564,#40565,#40566,#40567,#40568,#40569,#40570,#40571,#40572,#40573,#40574,
#40575,#40576,#40577,#40578,#40579,#40580,#40581,#40582,#40583,#40584,#40585,
#40586,#40587,#40588,#40589,#40590,#40591,#40592,#40593,#40594,#40595,#40596,
#40597,#40598,#40599,#40600,#40601,#40602,#40603,#40604,#40605,#40606,#40607,
#40608,#40609,#40610,#40611,#40612,#40613,#40614,#40615,#40616,#40617,#40618,
#40619,#40620,#40621,#40622,#40623,#40624,#40625,#40626,#40627,#40628,#40629,
#40630,#40631,#40632,#40633,#40634,#40635,#40636,#40637,#40638,#40639,#40640,
#40641,#40642,#40643,#40644,#40645,#40646,#40647,#40648,#40649,#40650,#40651,
#40652,#40653,#40654,#40655,#40656,#40657,#40658,#40659,#40660,#40661,#40662,
#40663,#40664,#40665,#40666,#40667,#40668,#40669,#40670,#40671,#40672,#40673,
#40674,#40675,#40676,#40677,#40678,#40679,#40680,#40681,#40682,#40683,#40684,
#40685,#40686,#40687,#40688,#40689,#40690,#40691,#40692,#40693,#40694,#40695,
#40696,#40697,#40698,#40699,#40700,#40701,#40702,#40703,#40704,#40705,#40706,
#40707,#40708,#40709,#40710,#40711,#40712,#40713,#40714,#40715,#40716,#40717,
#40718,#40719,#40720,#40721,#40722,#40723,#40724,#40725,#40726,#40727,#40728,
#40729,#40730,#40731,#40732,#40733,#40734,#40735,#40736,#40737,#40738)),
 .UNSPECIFIED.,.F.,.F.,.F.,(4,4),(4,1,1,1,1,1,1,1,1,1,1,1,1,1,1,1,1,1,1,
1,1,1,1,1,1,1,1,1,1,1,1,1,1,1,1,1,1,1,1,1,1,1,1,1,1,1,1,1,1,1,1,1,1,1,1,
1,1,1,1,1,1,1,1,1,1,1,1,1,1,1,1,1,1,1,1,1,1,1,1,1,1,1,1,1,1,1,1,1,1,1,1,
1,1,1,1,1,1,1,1,1,1,1,1,1,1,1,1,1,1,1,1,1,1,1,1,1,1,1,1,1,1,1,1,1,1,1,1,
1,1,1,1,1,1,1,1,1,1,1,1,1,1,1,1,1,1,1,1,1,1,1,1,1,1,1,1,1,1,1,1,1,1,1,1,
1,1,1,1,1,1,1,1,1,1,1,1,1,1,1,1,1,1,1,1,1,1,1,1,1,1,1,1,1,1,1,1,1,1,1,1,
1,1,1,1,1,1,1,1,1,1,1,1,1,1,1,1,1,1,1,1,1,1,1,1,1,1,1,1,1,1,1,1,1,1,1,1,
1,1,1,1,1,1,1,1,1,1,1,1,1,1,1,1,1,1,1,1,1,1,1,1,1,1,1,1,1,1,1,1,1,1,1,1,
1,1,1,1,1,1,1,1,1,1,1,1,1,1,1,1,1,1,1,1,1,1,1,1,1,1,1,1,1,1,1,1,1,1,1,1,
1,1,1,1,1,1,1,1,1,1,1,1,1,1,1,1,1,1,1,1,1,1,1,1,1,1,1,1,1,1,1,1,1,1,1,1,
1,1,1,1,1,1,1,1,1,1,1,1,1,1,1,1,1,1,1,1,1,1,1,1,1,1,1,1,1,1,1,1,1,1,1,1,
1,1,1,1,1,1,1,1,1,1,1,1,1,1,1,1,1,1,1,1,1,1,1,1,1,1,1,1,1,1,1,1,1,1,1,1,
1,1,1,1,1,1,1,1,1,1,1,1,1,1,1,1,1,1,1,1,1,1,1,1,1,1,1,1,1,1,1,1,1,1,1,1,
1,1,1,1,1,1,1,1,1,1,1,1,1,1,1,1,1,1,1,1,1,1,1,1,1,1,1,1,1,1,1,1,1,1,1,1,
1,1,1,1,1,1,1,1,4),(0.,0.184512097253587),(8.98171729021681,9.48139635699984,
9.98107542378286,10.4807544905659,10.9804335573489,11.4801126241319,11.979791690915,
12.479470757698,12.979149824481,13.478828891264,13.9785079580471,14.4781870248301,
14.9778660916131,15.4775451583961,15.9772242251791,16.4769032919622,16.9765823587452,
17.4762614255282,17.9759404923112,18.4756195590943,18.9752986258773,19.4749776926603,
19.9746567594433,20.4743358262264,20.9740148930094,21.4736939597924,21.9733730265754,
22.4730520933585,22.9727311601415,23.4724102269245,23.9720892937075,24.4717683604905,
24.9714474272736,25.4711264940566,25.9708055608396,26.4704846276226,26.9701636944057,
27.4698427611887,27.9695218279717,28.4692008947547,28.9688799615378,29.4685590283208,
29.9682380951038,30.4679171618868,30.9675962286699,31.4672752954529,31.9669543622359,
32.4666334290189,32.966312495802,33.465991562585,33.965670629368,34.465349696151,
34.965028762934,35.4647078297171,35.9643868965001,36.4640659632831,36.9637450300661,
37.4634240968492,37.9631031636322,38.4627822304152,38.9624612971982,39.4621403639813,
39.9618194307643,40.4614984975473,40.9611775643303,41.4608566311134,41.9605356978964,
42.4602147646794,42.9598938314624,43.4595728982454,43.9592519650285,44.4589310318115,
44.9586100985945,45.4582891653775,45.9579682321606,46.4576472989436,46.9573263657266,
47.4570054325096,47.9566844992927,48.4563635660757,48.9560426328587,49.4557216996417,
49.9554007664248,50.4550798332078,50.9547588999908,51.4544379667738,51.9541170335568,
52.4537961003399,52.9534751671229,53.4531542339059,53.9528333006889,54.452512367472,
54.952191434255,55.451870501038,55.951549567821,56.4512286346041,56.9509077013871,
57.4505867681701,57.9502658349531,58.4499449017362,58.9496239685192,59.9489821020852,
60.9483402356513,61.9476983692173,62.9470565027834,63.9464146363494,64.9457727699155,
65.9451309034815,66.9444890370476,67.9438471706136,68.9432053041797,69.9425634377457,
70.9419215713118,71.9412797048778,72.9406378384438,73.9399959720099,74.9393541055759,
75.938712239142,76.938070372708,77.9374285062741,78.9367866398401,79.9361447734062,
80.9355029069722,81.9348610405383,82.9342191741043,83.9335773076704,84.9329354412364,
85.9322935748025,86.9316517083685,87.9310098419346,88.9303679755006,89.9297261090666,
90.9290842426327,91.9284423761987,92.9278005097648,93.9271586433308,94.9265167768969,
95.9258749104629,96.925233044029,97.924591177595,98.9239493111611,99.9233074447271,
100.922665578293,101.922023711859,102.921381845425,103.920739978991,104.920098112557,
105.919456246123,106.918814379689,107.918172513255,108.917530646822,109.916888780388,
110.916246913954,111.91560504752,112.914963181086,113.914321314652,114.913679448218,
115.913037581784,116.91239571535,117.911753848916,118.911111982482,119.910470116048,
120.909828249614,121.90918638318,122.908544516746,123.907902650312,124.907260783878,
125.906618917444,126.90597705101,127.905335184576,128.904693318142,129.904051451709,
130.903409585275,131.902767718841,132.902125852407,133.901483985973,134.900842119539,
135.900200253105,136.899558386671,137.898916520237,138.898274653803,139.897632787369,
140.896990920935,141.896349054501,142.895707188067,143.895065321633,144.894423455199,
145.893781588765,146.893139722331,147.892497855897,148.891855989463,149.891214123029,
150.890572256596,151.889930390162,152.889288523728,153.888646657294,154.88800479086,
155.887362924426,156.886721057992,157.886079191558,158.885437325124,159.88479545869,
160.884153592256,161.883511725822,162.882869859388,163.882227992954,164.88158612652,
165.880944260086,166.880302393652,167.879660527218,168.879018660784,169.87837679435,
170.877734927916,171.877093061483,172.876451195049,173.875809328615,174.875167462181,
175.874525595747,176.873883729313,177.873241862879,178.872599996445,179.871958130011,
180.871316263577,181.870674397143,182.870032530709,183.869390664275,184.868748797841,
185.868106931407,186.867465064973,187.866823198539,188.866181332105,189.865539465671,
190.864897599237,191.864255732803,192.86361386637,193.862971999936,194.862330133502,
195.861688267068,196.861046400634,197.8604045342,198.859762667766,199.859120801332,
200.858478934898,201.857837068464,202.85719520203,203.856553335596,204.855911469162,
205.855269602728,206.854627736294,207.85398586986,208.853344003426,209.852702136992,
210.852060270558,211.851418404124,212.85077653769,213.850134671257,214.849492804823,
215.848850938389,216.848209071955,217.847567205521,218.846925339087,219.846283472653,
220.845641606219,221.844999739785,222.844357873351,223.843716006917,224.843074140483,
225.842432274049,226.841790407615,227.841148541181,228.840506674747,229.839864808313,
230.839222941879,231.838581075445,232.837939209011,233.837297342577,234.836655476144,
235.83601360971,236.835371743276,237.834729876842,238.834088010408,239.833446143974,
240.83280427754,241.832162411106,242.831520544672,243.830878678238,244.830236811804,
245.82959494537,246.828953078936,247.828311212502,248.827669346068,249.827027479634,
250.8263856132,251.825743746766,252.825101880332,253.824460013898,254.823818147464,
255.82317628103,256.822534414597,257.821892548163,258.821250681729,259.820608815295,
260.819966948861,261.819325082427,262.818683215993,263.818041349559,264.817399483125,
265.816757616691,266.816115750257,267.815473883823,268.814832017389,269.814190150955,
270.813548284521,271.812906418087,272.812264551653,273.811622685219,274.810980818785,
275.810338952351,276.809697085917,277.809055219484,278.80841335305,279.807771486616,
280.807129620182,281.806487753748,282.805845887314,283.80520402088,284.804562154446,
285.803920288012,286.803278421578,287.802636555144,288.80199468871,289.801352822276,
290.800710955842,291.800069089408,292.799427222974,293.79878535654,294.798143490106,
295.797501623672,296.796859757238,297.796217890804,298.795576024371,299.794934157937,
300.794292291503,301.793650425069,302.793008558635,303.792366692201,304.791724825767,
305.791082959333,306.790441092899,307.789799226465,308.789157360031,309.788515493597,
310.787873627163,311.787231760729,312.786589894295,313.785948027861,314.785306161427,
315.784664294993,316.784022428559,317.783380562125,318.782738695691,319.782096829258,
320.781454962824,321.78081309639,322.780171229956,323.779529363522,324.778887497088,
325.778245630654,326.77760376422,327.776961897786,328.776320031352,329.775678164918,
330.775036298484,331.77439443205,332.773752565616,333.773110699182,334.772468832748,
335.771826966314,336.77118509988,337.770543233446,338.769901367012,339.769259500578,
340.768617634145,341.767975767711,342.767333901277,343.766692034843,344.766050168409,
345.765408301975,346.764766435541,347.764124569107,348.763482702673,349.762840836239,
350.762198969805,351.761557103371,352.760915236937,353.760273370503,354.259952437286,
354.759631504069,355.259310570852,355.758989637635,356.258668704418,356.758347771201,
357.258026837984,357.757705904767,358.25738497155,358.757064038333,359.256743105116,
359.756422171899,360.256101238682,360.755780305465,361.255459372248,361.755138439031,
362.254817505815,362.754496572598,363.254175639381,363.753854706164,364.253533772947,
364.75321283973,365.252891906513,365.752570973296,366.252250040079,366.751929106862,
367.251608173645,367.751287240428,368.250966307211,368.750645373994,369.250324440777,
369.75000350756,370.249682574343,370.749361641126,371.249040707909,371.748719774692,
372.248398841475,372.748077908258,373.247756975041,373.747436041824,374.247115108607,
374.74679417539,375.246473242173,375.746152308956,376.245831375739,376.745510442522,
377.245189509305,377.744868576088,378.244547642871,378.744226709654,379.243905776437,
379.74358484322,380.243263910003,380.742942976786,381.242622043569,381.742301110352,
382.241980177135,382.741659243918,383.241338310702,383.741017377485,384.240696444268,
384.740375511051,385.240054577834,385.739733644617,386.2394127114,386.739091778183,
387.238770844966,387.738449911749,388.238128978532,388.737808045315,389.237487112098,
389.737166178881,390.236845245664,390.736524312447,391.23620337923,391.735882446013,
392.235561512796,392.735240579579,393.234919646362,393.734598713145,394.234277779928,
394.733956846711,395.233635913494,395.733314980277,396.23299404706,396.732673113843,
397.232352180626,397.732031247409,398.231710314192,398.731389380975,399.231068447758,
399.730747514541,400.230426581324,400.730105648107,401.22978471489,401.729463781673,
402.229142848456,402.728821915239,403.228500982022,403.728180048805),
 .UNSPECIFIED.);
#14=B_SPLINE_SURFACE_WITH_KNOTS('',3,3,((#40832,#40833,#40834,#40835,#40836,
#40837,#40838,#40839,#40840,#40841,#40842,#40843,#40844,#40845,#40846,#40847,
#40848,#40849,#40850,#40851,#40852,#40853,#40854,#40855,#40856,#40857,#40858,
#40859,#40860,#40861,#40862,#40863,#40864,#40865,#40866,#40867,#40868,#40869,
#40870,#40871,#40872,#40873,#40874,#40875,#40876,#40877,#40878,#40879,#40880,
#40881,#40882,#40883,#40884,#40885,#40886,#40887,#40888,#40889,#40890,#40891,
#40892,#40893,#40894,#40895,#40896,#40897,#40898,#40899,#40900,#40901,#40902,
#40903,#40904,#40905,#40906,#40907,#40908,#40909,#40910,#40911,#40912,#40913,
#40914,#40915,#40916,#40917,#40918,#40919,#40920,#40921,#40922,#40923,#40924,
#40925,#40926,#40927,#40928,#40929,#40930,#40931,#40932,#40933,#40934,#40935,
#40936,#40937,#40938,#40939,#40940,#40941,#40942,#40943,#40944,#40945,#40946,
#40947,#40948,#40949,#40950,#40951,#40952,#40953,#40954,#40955,#40956,#40957,
#40958,#40959,#40960,#40961,#40962,#40963,#40964,#40965,#40966,#40967,#40968,
#40969,#40970,#40971,#40972,#40973,#40974,#40975,#40976,#40977,#40978,#40979,
#40980,#40981,#40982,#40983,#40984,#40985,#40986,#40987,#40988,#40989,#40990,
#40991,#40992,#40993,#40994,#40995,#40996,#40997,#40998,#40999,#41000,#41001,
#41002,#41003,#41004,#41005,#41006,#41007,#41008,#41009,#41010,#41011,#41012,
#41013,#41014,#41015,#41016,#41017,#41018,#41019,#41020,#41021,#41022,#41023,
#41024,#41025,#41026,#41027,#41028,#41029,#41030,#41031,#41032,#41033,#41034,
#41035,#41036,#41037,#41038,#41039,#41040,#41041,#41042,#41043,#41044,#41045,
#41046,#41047,#41048,#41049,#41050,#41051,#41052,#41053,#41054,#41055,#41056,
#41057,#41058,#41059,#41060,#41061,#41062,#41063,#41064,#41065,#41066,#41067,
#41068,#41069,#41070,#41071,#41072,#41073,#41074,#41075,#41076,#41077,#41078,
#41079,#41080,#41081,#41082,#41083,#41084,#41085,#41086,#41087,#41088,#41089,
#41090,#41091,#41092,#41093,#41094,#41095,#41096,#41097,#41098,#41099,#41100,
#41101,#41102,#41103,#41104,#41105,#41106,#41107,#41108,#41109,#41110,#41111,
#41112,#41113,#41114,#41115,#41116,#41117,#41118,#41119,#41120,#41121,#41122,
#41123,#41124,#41125,#41126,#41127,#41128,#41129,#41130,#41131,#41132,#41133,
#41134,#41135,#41136,#41137,#41138,#41139,#41140,#41141,#41142,#41143,#41144,
#41145,#41146,#41147,#41148,#41149,#41150,#41151,#41152,#41153,#41154,#41155,
#41156,#41157,#41158,#41159,#41160,#41161,#41162,#41163,#41164,#41165,#41166,
#41167,#41168,#41169,#41170,#41171,#41172,#41173,#41174,#41175,#41176,#41177,
#41178,#41179,#41180,#41181,#41182,#41183,#41184,#41185,#41186,#41187,#41188,
#41189,#41190,#41191,#41192,#41193,#41194,#41195,#41196,#41197,#41198,#41199,
#41200,#41201,#41202,#41203,#41204,#41205,#41206,#41207,#41208,#41209,#41210,
#41211,#41212,#41213,#41214,#41215,#41216,#41217,#41218,#41219,#41220,#41221,
#41222,#41223,#41224,#41225,#41226,#41227,#41228,#41229,#41230,#41231,#41232,
#41233,#41234,#41235,#41236,#41237,#41238,#41239,#41240,#41241,#41242,#41243,
#41244,#41245,#41246,#41247,#41248,#41249,#41250,#41251,#41252,#41253,#41254,
#41255,#41256,#41257,#41258,#41259,#41260,#41261,#41262,#41263,#41264,#41265,
#41266,#41267,#41268,#41269,#41270,#41271,#41272,#41273,#41274,#41275,#41276,
#41277,#41278,#41279,#41280,#41281,#41282,#41283,#41284,#41285,#41286,#41287,
#41288,#41289,#41290,#41291,#41292,#41293,#41294,#41295,#41296,#41297,#41298,
#41299,#41300,#41301,#41302,#41303,#41304,#41305,#41306,#41307,#41308,#41309,
#41310,#41311,#41312,#41313,#41314,#41315,#41316,#41317,#41318,#41319,#41320,
#41321,#41322,#41323,#41324,#41325,#41326,#41327,#41328,#41329),(#41330,
#41331,#41332,#41333,#41334,#41335,#41336,#41337,#41338,#41339,#41340,#41341,
#41342,#41343,#41344,#41345,#41346,#41347,#41348,#41349,#41350,#41351,#41352,
#41353,#41354,#41355,#41356,#41357,#41358,#41359,#41360,#41361,#41362,#41363,
#41364,#41365,#41366,#41367,#41368,#41369,#41370,#41371,#41372,#41373,#41374,
#41375,#41376,#41377,#41378,#41379,#41380,#41381,#41382,#41383,#41384,#41385,
#41386,#41387,#41388,#41389,#41390,#41391,#41392,#41393,#41394,#41395,#41396,
#41397,#41398,#41399,#41400,#41401,#41402,#41403,#41404,#41405,#41406,#41407,
#41408,#41409,#41410,#41411,#41412,#41413,#41414,#41415,#41416,#41417,#41418,
#41419,#41420,#41421,#41422,#41423,#41424,#41425,#41426,#41427,#41428,#41429,
#41430,#41431,#41432,#41433,#41434,#41435,#41436,#41437,#41438,#41439,#41440,
#41441,#41442,#41443,#41444,#41445,#41446,#41447,#41448,#41449,#41450,#41451,
#41452,#41453,#41454,#41455,#41456,#41457,#41458,#41459,#41460,#41461,#41462,
#41463,#41464,#41465,#41466,#41467,#41468,#41469,#41470,#41471,#41472,#41473,
#41474,#41475,#41476,#41477,#41478,#41479,#41480,#41481,#41482,#41483,#41484,
#41485,#41486,#41487,#41488,#41489,#41490,#41491,#41492,#41493,#41494,#41495,
#41496,#41497,#41498,#41499,#41500,#41501,#41502,#41503,#41504,#41505,#41506,
#41507,#41508,#41509,#41510,#41511,#41512,#41513,#41514,#41515,#41516,#41517,
#41518,#41519,#41520,#41521,#41522,#41523,#41524,#41525,#41526,#41527,#41528,
#41529,#41530,#41531,#41532,#41533,#41534,#41535,#41536,#41537,#41538,#41539,
#41540,#41541,#41542,#41543,#41544,#41545,#41546,#41547,#41548,#41549,#41550,
#41551,#41552,#41553,#41554,#41555,#41556,#41557,#41558,#41559,#41560,#41561,
#41562,#41563,#41564,#41565,#41566,#41567,#41568,#41569,#41570,#41571,#41572,
#41573,#41574,#41575,#41576,#41577,#41578,#41579,#41580,#41581,#41582,#41583,
#41584,#41585,#41586,#41587,#41588,#41589,#41590,#41591,#41592,#41593,#41594,
#41595,#41596,#41597,#41598,#41599,#41600,#41601,#41602,#41603,#41604,#41605,
#41606,#41607,#41608,#41609,#41610,#41611,#41612,#41613,#41614,#41615,#41616,
#41617,#41618,#41619,#41620,#41621,#41622,#41623,#41624,#41625,#41626,#41627,
#41628,#41629,#41630,#41631,#41632,#41633,#41634,#41635,#41636,#41637,#41638,
#41639,#41640,#41641,#41642,#41643,#41644,#41645,#41646,#41647,#41648,#41649,
#41650,#41651,#41652,#41653,#41654,#41655,#41656,#41657,#41658,#41659,#41660,
#41661,#41662,#41663,#41664,#41665,#41666,#41667,#41668,#41669,#41670,#41671,
#41672,#41673,#41674,#41675,#41676,#41677,#41678,#41679,#41680,#41681,#41682,
#41683,#41684,#41685,#41686,#41687,#41688,#41689,#41690,#41691,#41692,#41693,
#41694,#41695,#41696,#41697,#41698,#41699,#41700,#41701,#41702,#41703,#41704,
#41705,#41706,#41707,#41708,#41709,#41710,#41711,#41712,#41713,#41714,#41715,
#41716,#41717,#41718,#41719,#41720,#41721,#41722,#41723,#41724,#41725,#41726,
#41727,#41728,#41729,#41730,#41731,#41732,#41733,#41734,#41735,#41736,#41737,
#41738,#41739,#41740,#41741,#41742,#41743,#41744,#41745,#41746,#41747,#41748,
#41749,#41750,#41751,#41752,#41753,#41754,#41755,#41756,#41757,#41758,#41759,
#41760,#41761,#41762,#41763,#41764,#41765,#41766,#41767,#41768,#41769,#41770,
#41771,#41772,#41773,#41774,#41775,#41776,#41777,#41778,#41779,#41780,#41781,
#41782,#41783,#41784,#41785,#41786,#41787,#41788,#41789,#41790,#41791,#41792,
#41793,#41794,#41795,#41796,#41797,#41798,#41799,#41800,#41801,#41802,#41803,
#41804,#41805,#41806,#41807,#41808,#41809,#41810,#41811,#41812,#41813,#41814,
#41815,#41816,#41817,#41818,#41819,#41820,#41821,#41822,#41823,#41824,#41825,
#41826,#41827),(#41828,#41829,#41830,#41831,#41832,#41833,#41834,#41835,
#41836,#41837,#41838,#41839,#41840,#41841,#41842,#41843,#41844,#41845,#41846,
#41847,#41848,#41849,#41850,#41851,#41852,#41853,#41854,#41855,#41856,#41857,
#41858,#41859,#41860,#41861,#41862,#41863,#41864,#41865,#41866,#41867,#41868,
#41869,#41870,#41871,#41872,#41873,#41874,#41875,#41876,#41877,#41878,#41879,
#41880,#41881,#41882,#41883,#41884,#41885,#41886,#41887,#41888,#41889,#41890,
#41891,#41892,#41893,#41894,#41895,#41896,#41897,#41898,#41899,#41900,#41901,
#41902,#41903,#41904,#41905,#41906,#41907,#41908,#41909,#41910,#41911,#41912,
#41913,#41914,#41915,#41916,#41917,#41918,#41919,#41920,#41921,#41922,#41923,
#41924,#41925,#41926,#41927,#41928,#41929,#41930,#41931,#41932,#41933,#41934,
#41935,#41936,#41937,#41938,#41939,#41940,#41941,#41942,#41943,#41944,#41945,
#41946,#41947,#41948,#41949,#41950,#41951,#41952,#41953,#41954,#41955,#41956,
#41957,#41958,#41959,#41960,#41961,#41962,#41963,#41964,#41965,#41966,#41967,
#41968,#41969,#41970,#41971,#41972,#41973,#41974,#41975,#41976,#41977,#41978,
#41979,#41980,#41981,#41982,#41983,#41984,#41985,#41986,#41987,#41988,#41989,
#41990,#41991,#41992,#41993,#41994,#41995,#41996,#41997,#41998,#41999,#42000,
#42001,#42002,#42003,#42004,#42005,#42006,#42007,#42008,#42009,#42010,#42011,
#42012,#42013,#42014,#42015,#42016,#42017,#42018,#42019,#42020,#42021,#42022,
#42023,#42024,#42025,#42026,#42027,#42028,#42029,#42030,#42031,#42032,#42033,
#42034,#42035,#42036,#42037,#42038,#42039,#42040,#42041,#42042,#42043,#42044,
#42045,#42046,#42047,#42048,#42049,#42050,#42051,#42052,#42053,#42054,#42055,
#42056,#42057,#42058,#42059,#42060,#42061,#42062,#42063,#42064,#42065,#42066,
#42067,#42068,#42069,#42070,#42071,#42072,#42073,#42074,#42075,#42076,#42077,
#42078,#42079,#42080,#42081,#42082,#42083,#42084,#42085,#42086,#42087,#42088,
#42089,#42090,#42091,#42092,#42093,#42094,#42095,#42096,#42097,#42098,#42099,
#42100,#42101,#42102,#42103,#42104,#42105,#42106,#42107,#42108,#42109,#42110,
#42111,#42112,#42113,#42114,#42115,#42116,#42117,#42118,#42119,#42120,#42121,
#42122,#42123,#42124,#42125,#42126,#42127,#42128,#42129,#42130,#42131,#42132,
#42133,#42134,#42135,#42136,#42137,#42138,#42139,#42140,#42141,#42142,#42143,
#42144,#42145,#42146,#42147,#42148,#42149,#42150,#42151,#42152,#42153,#42154,
#42155,#42156,#42157,#42158,#42159,#42160,#42161,#42162,#42163,#42164,#42165,
#42166,#42167,#42168,#42169,#42170,#42171,#42172,#42173,#42174,#42175,#42176,
#42177,#42178,#42179,#42180,#42181,#42182,#42183,#42184,#42185,#42186,#42187,
#42188,#42189,#42190,#42191,#42192,#42193,#42194,#42195,#42196,#42197,#42198,
#42199,#42200,#42201,#42202,#42203,#42204,#42205,#42206,#42207,#42208,#42209,
#42210,#42211,#42212,#42213,#42214,#42215,#42216,#42217,#42218,#42219,#42220,
#42221,#42222,#42223,#42224,#42225,#42226,#42227,#42228,#42229,#42230,#42231,
#42232,#42233,#42234,#42235,#42236,#42237,#42238,#42239,#42240,#42241,#42242,
#42243,#42244,#42245,#42246,#42247,#42248,#42249,#42250,#42251,#42252,#42253,
#42254,#42255,#42256,#42257,#42258,#42259,#42260,#42261,#42262,#42263,#42264,
#42265,#42266,#42267,#42268,#42269,#42270,#42271,#42272,#42273,#42274,#42275,
#42276,#42277,#42278,#42279,#42280,#42281,#42282,#42283,#42284,#42285,#42286,
#42287,#42288,#42289,#42290,#42291,#42292,#42293,#42294,#42295,#42296,#42297,
#42298,#42299,#42300,#42301,#42302,#42303,#42304,#42305,#42306,#42307,#42308,
#42309,#42310,#42311,#42312,#42313,#42314,#42315,#42316,#42317,#42318,#42319,
#42320,#42321,#42322,#42323,#42324,#42325),(#42326,#42327,#42328,#42329,
#42330,#42331,#42332,#42333,#42334,#42335,#42336,#42337,#42338,#42339,#42340,
#42341,#42342,#42343,#42344,#42345,#42346,#42347,#42348,#42349,#42350,#42351,
#42352,#42353,#42354,#42355,#42356,#42357,#42358,#42359,#42360,#42361,#42362,
#42363,#42364,#42365,#42366,#42367,#42368,#42369,#42370,#42371,#42372,#42373,
#42374,#42375,#42376,#42377,#42378,#42379,#42380,#42381,#42382,#42383,#42384,
#42385,#42386,#42387,#42388,#42389,#42390,#42391,#42392,#42393,#42394,#42395,
#42396,#42397,#42398,#42399,#42400,#42401,#42402,#42403,#42404,#42405,#42406,
#42407,#42408,#42409,#42410,#42411,#42412,#42413,#42414,#42415,#42416,#42417,
#42418,#42419,#42420,#42421,#42422,#42423,#42424,#42425,#42426,#42427,#42428,
#42429,#42430,#42431,#42432,#42433,#42434,#42435,#42436,#42437,#42438,#42439,
#42440,#42441,#42442,#42443,#42444,#42445,#42446,#42447,#42448,#42449,#42450,
#42451,#42452,#42453,#42454,#42455,#42456,#42457,#42458,#42459,#42460,#42461,
#42462,#42463,#42464,#42465,#42466,#42467,#42468,#42469,#42470,#42471,#42472,
#42473,#42474,#42475,#42476,#42477,#42478,#42479,#42480,#42481,#42482,#42483,
#42484,#42485,#42486,#42487,#42488,#42489,#42490,#42491,#42492,#42493,#42494,
#42495,#42496,#42497,#42498,#42499,#42500,#42501,#42502,#42503,#42504,#42505,
#42506,#42507,#42508,#42509,#42510,#42511,#42512,#42513,#42514,#42515,#42516,
#42517,#42518,#42519,#42520,#42521,#42522,#42523,#42524,#42525,#42526,#42527,
#42528,#42529,#42530,#42531,#42532,#42533,#42534,#42535,#42536,#42537,#42538,
#42539,#42540,#42541,#42542,#42543,#42544,#42545,#42546,#42547,#42548,#42549,
#42550,#42551,#42552,#42553,#42554,#42555,#42556,#42557,#42558,#42559,#42560,
#42561,#42562,#42563,#42564,#42565,#42566,#42567,#42568,#42569,#42570,#42571,
#42572,#42573,#42574,#42575,#42576,#42577,#42578,#42579,#42580,#42581,#42582,
#42583,#42584,#42585,#42586,#42587,#42588,#42589,#42590,#42591,#42592,#42593,
#42594,#42595,#42596,#42597,#42598,#42599,#42600,#42601,#42602,#42603,#42604,
#42605,#42606,#42607,#42608,#42609,#42610,#42611,#42612,#42613,#42614,#42615,
#42616,#42617,#42618,#42619,#42620,#42621,#42622,#42623,#42624,#42625,#42626,
#42627,#42628,#42629,#42630,#42631,#42632,#42633,#42634,#42635,#42636,#42637,
#42638,#42639,#42640,#42641,#42642,#42643,#42644,#42645,#42646,#42647,#42648,
#42649,#42650,#42651,#42652,#42653,#42654,#42655,#42656,#42657,#42658,#42659,
#42660,#42661,#42662,#42663,#42664,#42665,#42666,#42667,#42668,#42669,#42670,
#42671,#42672,#42673,#42674,#42675,#42676,#42677,#42678,#42679,#42680,#42681,
#42682,#42683,#42684,#42685,#42686,#42687,#42688,#42689,#42690,#42691,#42692,
#42693,#42694,#42695,#42696,#42697,#42698,#42699,#42700,#42701,#42702,#42703,
#42704,#42705,#42706,#42707,#42708,#42709,#42710,#42711,#42712,#42713,#42714,
#42715,#42716,#42717,#42718,#42719,#42720,#42721,#42722,#42723,#42724,#42725,
#42726,#42727,#42728,#42729,#42730,#42731,#42732,#42733,#42734,#42735,#42736,
#42737,#42738,#42739,#42740,#42741,#42742,#42743,#42744,#42745,#42746,#42747,
#42748,#42749,#42750,#42751,#42752,#42753,#42754,#42755,#42756,#42757,#42758,
#42759,#42760,#42761,#42762,#42763,#42764,#42765,#42766,#42767,#42768,#42769,
#42770,#42771,#42772,#42773,#42774,#42775,#42776,#42777,#42778,#42779,#42780,
#42781,#42782,#42783,#42784,#42785,#42786,#42787,#42788,#42789,#42790,#42791,
#42792,#42793,#42794,#42795,#42796,#42797,#42798,#42799,#42800,#42801,#42802,
#42803,#42804,#42805,#42806,#42807,#42808,#42809,#42810,#42811,#42812,#42813,
#42814,#42815,#42816,#42817,#42818,#42819,#42820,#42821,#42822,#42823)),
 .UNSPECIFIED.,.F.,.F.,.F.,(4,4),(4,1,1,1,1,1,1,1,1,1,1,1,1,1,1,1,1,1,1,
1,1,1,1,1,1,1,1,1,1,1,1,1,1,1,1,1,1,1,1,1,1,1,1,1,1,1,1,1,1,1,1,1,1,1,1,
1,1,1,1,1,1,1,1,1,1,1,1,1,1,1,1,1,1,1,1,1,1,1,1,1,1,1,1,1,1,1,1,1,1,1,1,
1,1,1,1,1,1,1,1,1,1,1,1,1,1,1,1,1,1,1,1,1,1,1,1,1,1,1,1,1,1,1,1,1,1,1,1,
1,1,1,1,1,1,1,1,1,1,1,1,1,1,1,1,1,1,1,1,1,1,1,1,1,1,1,1,1,1,1,1,1,1,1,1,
1,1,1,1,1,1,1,1,1,1,1,1,1,1,1,1,1,1,1,1,1,1,1,1,1,1,1,1,1,1,1,1,1,1,1,1,
1,1,1,1,1,1,1,1,1,1,1,1,1,1,1,1,1,1,1,1,1,1,1,1,1,1,1,1,1,1,1,1,1,1,1,1,
1,1,1,1,1,1,1,1,1,1,1,1,1,1,1,1,1,1,1,1,1,1,1,1,1,1,1,1,1,1,1,1,1,1,1,1,
1,1,1,1,1,1,1,1,1,1,1,1,1,1,1,1,1,1,1,1,1,1,1,1,1,1,1,1,1,1,1,1,1,1,1,1,
1,1,1,1,1,1,1,1,1,1,1,1,1,1,1,1,1,1,1,1,1,1,1,1,1,1,1,1,1,1,1,1,1,1,1,1,
1,1,1,1,1,1,1,1,1,1,1,1,1,1,1,1,1,1,1,1,1,1,1,1,1,1,1,1,1,1,1,1,1,1,1,1,
1,1,1,1,1,1,1,1,1,1,1,1,1,1,1,1,1,1,1,1,1,1,1,1,1,1,1,1,1,1,1,1,1,1,1,1,
1,1,1,1,1,1,1,1,1,1,1,1,1,1,1,1,1,1,1,1,1,1,1,1,1,1,1,1,1,1,1,1,1,1,1,1,
1,1,1,1,1,1,1,1,1,1,1,1,1,1,1,1,1,1,1,1,1,1,1,1,1,1,1,1,1,1,1,1,1,1,1,1,
1,1,1,1,1,1,1,1,4),(0.,0.184512097253587),(12.0092477762453,12.5089268430284,
13.0086059098114,13.5082849765944,14.0079640433774,14.5076431101605,15.0073221769435,
15.5070012437265,16.0066803105095,16.5063593772925,17.0060384440756,17.5057175108586,
18.0053965776416,18.5050756444246,19.0047547112077,19.5044337779907,20.0041128447737,
20.5037919115567,21.0034709783398,21.5031500451228,22.0028291119058,22.5025081786888,
23.0021872454719,23.5018663122549,24.0015453790379,24.5012244458209,25.0009035126039,
25.500582579387,26.00026164617,26.499940712953,26.999619779736,27.4992988465191,
27.9989779133021,28.4986569800851,28.9983360468681,29.4980151136512,29.9976941804342,
30.4973732472172,30.9970523140002,31.4967313807832,31.9964104475663,32.4960895143493,
32.9957685811323,33.4954476479153,33.9951267146984,34.4948057814814,34.9944848482644,
35.4941639150474,35.9938429818305,36.4935220486135,36.9932011153965,37.4928801821795,
37.9925592489626,38.4922383157456,38.9919173825286,39.4915964493116,39.9912755160946,
40.4909545828777,40.9906336496607,41.4903127164437,41.9899917832267,42.4896708500098,
42.9893499167928,43.4890289835758,43.9887080503588,44.4883871171419,44.9880661839249,
45.4877452507079,45.9874243174909,46.4871033842739,46.986782451057,47.48646151784,
47.986140584623,48.485819651406,48.9854987181891,49.4851777849721,49.9848568517551,
50.4845359185381,50.9842149853212,51.4838940521042,51.9835731188872,52.4832521856702,
52.9829312524532,53.4826103192363,53.9822893860193,54.4819684528023,54.9816475195853,
55.4813265863684,55.9810056531514,56.4806847199344,56.9803637867174,57.4800428535005,
57.9797219202835,58.4794009870665,58.9790800538495,59.4787591206325,59.9784381874156,
60.4781172541986,60.9777963209816,61.4774753877646,61.9771544545477,62.9765125881137,
63.9758707216798,64.9752288552458,65.9745869888119,66.9739451223779,67.9733032559439,
68.97266138951,69.972019523076,70.9713776566421,71.9707357902081,72.9700939237742,
73.9694520573402,74.9688101909063,75.9681683244723,76.9675264580384,77.9668845916044,
78.9662427251705,79.9656008587365,80.9649589923026,81.9643171258686,82.9636752594347,
83.9630333930007,84.9623915265667,85.9617496601328,86.9611077936988,87.9604659272649,
88.9598240608309,89.959182194397,90.958540327963,91.9578984615291,92.9572565950951,
93.9566147286612,94.9559728622272,95.9553309957932,96.9546891293593,97.9540472629253,
98.9534053964914,99.9527635300574,100.952121663623,101.95147979719,102.950837930756,
103.950196064322,104.949554197888,105.948912331454,106.94827046502,107.947628598586,
108.946986732152,109.946344865718,110.945702999284,111.94506113285,112.944419266416,
113.943777399982,114.943135533548,115.942493667114,116.94185180068,117.941209934246,
118.940568067812,119.939926201378,120.939284334944,121.93864246851,122.938000602077,
123.937358735643,124.936716869209,125.936075002775,126.935433136341,127.934791269907,
128.934149403473,129.933507537039,130.932865670605,131.932223804171,132.931581937737,
133.930940071303,134.930298204869,135.929656338435,136.929014472001,137.928372605567,
138.927730739133,139.927088872699,140.926447006265,141.925805139831,142.925163273397,
143.924521406963,144.92387954053,145.923237674096,146.922595807662,147.921953941228,
148.921312074794,149.92067020836,150.920028341926,151.919386475492,152.918744609058,
153.918102742624,154.91746087619,155.916819009756,156.916177143322,157.915535276888,
158.914893410454,159.91425154402,160.913609677586,161.912967811152,162.912325944718,
163.911684078284,164.91104221185,165.910400345416,166.909758478983,167.909116612549,
168.908474746115,169.907832879681,170.907191013247,171.906549146813,172.905907280379,
173.905265413945,174.904623547511,175.903981681077,176.903339814643,177.902697948209,
178.902056081775,179.901414215341,180.900772348907,181.900130482473,182.899488616039,
183.898846749605,184.898204883171,185.897563016737,186.896921150303,187.89627928387,
188.895637417436,189.894995551002,190.894353684568,191.893711818134,192.8930699517,
193.892428085266,194.891786218832,195.891144352398,196.890502485964,197.88986061953,
198.889218753096,199.888576886662,200.887935020228,201.887293153794,202.88665128736,
203.886009420926,204.885367554492,205.884725688058,206.884083821624,207.88344195519,
208.882800088756,209.882158222323,210.881516355889,211.880874489455,212.880232623021,
213.879590756587,214.878948890153,215.878307023719,216.877665157285,217.877023290851,
218.876381424417,219.875739557983,220.875097691549,221.874455825115,222.873813958681,
223.873172092247,224.872530225813,225.871888359379,226.871246492945,227.870604626511,
228.869962760077,229.869320893643,230.86867902721,231.868037160776,232.867395294342,
233.866753427908,234.866111561474,235.86546969504,236.864827828606,237.864185962172,
238.863544095738,239.862902229304,240.86226036287,241.861618496436,242.860976630002,
243.860334763568,244.859692897134,245.8590510307,246.858409164266,247.857767297832,
248.857125431398,249.856483564964,250.85584169853,251.855199832097,252.854557965663,
253.853916099229,254.853274232795,255.852632366361,256.851990499927,257.851348633493,
258.850706767059,259.850064900625,260.849423034191,261.848781167757,262.848139301323,
263.847497434889,264.846855568455,265.846213702021,266.845571835587,267.844929969153,
268.844288102719,269.843646236285,270.843004369851,271.842362503417,272.841720636983,
273.84107877055,274.840436904116,275.839795037682,276.839153171248,277.838511304814,
278.83786943838,279.837227571946,280.836585705512,281.835943839078,282.835301972644,
283.83466010621,284.834018239776,285.833376373342,286.832734506908,287.832092640474,
288.83145077404,289.830808907606,290.830167041172,291.829525174738,292.828883308304,
293.82824144187,294.827599575437,295.826957709003,296.826315842569,297.825673976135,
298.825032109701,299.824390243267,300.823748376833,301.823106510399,302.822464643965,
303.821822777531,304.821180911097,305.820539044663,306.819897178229,307.819255311795,
308.818613445361,309.817971578927,310.817329712493,311.816687846059,312.816045979625,
313.815404113191,314.814762246757,315.814120380323,316.81347851389,317.812836647456,
318.812194781022,319.811552914588,320.810911048154,321.81026918172,322.809627315286,
323.808985448852,324.808343582418,325.807701715984,326.80705984955,327.806417983116,
328.805776116682,329.805134250248,330.804492383814,331.80385051738,332.803208650946,
333.802566784512,334.801924918078,335.801283051644,336.80064118521,337.799999318776,
338.799357452343,339.798715585909,340.798073719475,341.797431853041,342.796789986607,
343.796148120173,344.795506253739,345.794864387305,346.794222520871,347.793580654437,
348.792938788003,349.792296921569,350.791655055135,351.791013188701,352.790371322267,
353.789729455833,354.789087589399,355.788445722965,356.787803856531,357.287482923314,
357.787161990097,358.28684105688,358.786520123663,359.286199190446,359.78587825723,
360.285557324013,360.785236390796,361.284915457579,361.784594524362,362.284273591145,
362.783952657928,363.283631724711,363.783310791494,364.282989858277,364.78266892506,
365.282347991843,365.782027058626,366.281706125409,366.781385192192,367.281064258975,
367.780743325758,368.280422392541,368.780101459324,369.279780526107,369.77945959289,
370.279138659673,370.778817726456,371.278496793239,371.778175860022,372.277854926805,
372.777533993588,373.277213060371,373.776892127154,374.276571193937,374.77625026072,
375.275929327503,375.775608394286,376.275287461069,376.774966527852,377.274645594635,
377.774324661418,378.274003728201,378.773682794984,379.273361861767,379.77304092855,
380.272719995333,380.772399062117,381.2720781289,381.771757195683,382.271436262466,
382.771115329249,383.270794396032,383.770473462815,384.270152529598,384.769831596381,
385.269510663164,385.769189729947,386.26886879673,386.768547863513,387.268226930296,
387.767905997079,388.267585063862,388.767264130645,389.266943197428,389.766622264211,
390.266301330994,390.765980397777,391.26565946456,391.765338531343,392.265017598126,
392.764696664909,393.264375731692,393.764054798475,394.263733865258,394.763412932041,
395.263091998824,395.762771065607,396.26245013239,396.762129199173,397.261808265956,
397.761487332739,398.261166399522,398.760845466305,399.260524533088,399.760203599871,
400.259882666654,400.759561733437,401.25924080022,401.758919867003,402.258598933787,
402.75827800057,403.257957067353,403.757636134136,404.257315200919,404.756994267702,
405.256673334485,405.756352401268,406.256031468051,406.755710534834),
 .UNSPECIFIED.);
#15=ELLIPSE('',#20393,0.299389011154384,0.2117);
#16=ELLIPSE('',#20397,0.299389011154384,0.2117);
#17=ITEM_DEFINED_TRANSFORMATION($,$,#19993,#20115);
#18=ITEM_DEFINED_TRANSFORMATION($,$,#20013,#20116);
#19=ITEM_DEFINED_TRANSFORMATION($,$,#20033,#20117);
#20=ITEM_DEFINED_TRANSFORMATION($,$,#20048,#20118);
#21=ITEM_DEFINED_TRANSFORMATION($,$,#20098,#20119);
#22=ITEM_DEFINED_TRANSFORMATION($,$,#20121,#20249);
#23=ITEM_DEFINED_TRANSFORMATION($,$,#20141,#20250);
#24=ITEM_DEFINED_TRANSFORMATION($,$,#20161,#20251);
#25=ITEM_DEFINED_TRANSFORMATION($,$,#20178,#20252);
#26=ITEM_DEFINED_TRANSFORMATION($,$,#20232,#20253);
#27=ITEM_DEFINED_TRANSFORMATION($,$,#20640,#20689);
#28=ITEM_DEFINED_TRANSFORMATION($,$,#20672,#20690);
#29=ITEM_DEFINED_TRANSFORMATION($,$,#19286,#20790);
#30=ITEM_DEFINED_TRANSFORMATION($,$,#19361,#20791);
#31=ITEM_DEFINED_TRANSFORMATION($,$,#19368,#20792);
#32=ITEM_DEFINED_TRANSFORMATION($,$,#19375,#20793);
#33=ITEM_DEFINED_TRANSFORMATION($,$,#19416,#20794);
#34=ITEM_DEFINED_TRANSFORMATION($,$,#19445,#20795);
#35=ITEM_DEFINED_TRANSFORMATION($,$,#19474,#20796);
#36=ITEM_DEFINED_TRANSFORMATION($,$,#19495,#20797);
#37=ITEM_DEFINED_TRANSFORMATION($,$,#19522,#20798);
#38=ITEM_DEFINED_TRANSFORMATION($,$,#19543,#20799);
#39=ITEM_DEFINED_TRANSFORMATION($,$,#19570,#20800);
#40=ITEM_DEFINED_TRANSFORMATION($,$,#19613,#20801);
#41=ITEM_DEFINED_TRANSFORMATION($,$,#19664,#20802);
#42=ITEM_DEFINED_TRANSFORMATION($,$,#19686,#20803);
#43=ITEM_DEFINED_TRANSFORMATION($,$,#19708,#20804);
#44=ITEM_DEFINED_TRANSFORMATION($,$,#19718,#20805);
#45=ITEM_DEFINED_TRANSFORMATION($,$,#19728,#20806);
#46=ITEM_DEFINED_TRANSFORMATION($,$,#19738,#20807);
#47=ITEM_DEFINED_TRANSFORMATION($,$,#19748,#20808);
#48=ITEM_DEFINED_TRANSFORMATION($,$,#19782,#20809);
#49=ITEM_DEFINED_TRANSFORMATION($,$,#20356,#20810);
#50=ITEM_DEFINED_TRANSFORMATION($,$,#20356,#20811);
#51=ITEM_DEFINED_TRANSFORMATION($,$,#20356,#20812);
#52=ITEM_DEFINED_TRANSFORMATION($,$,#20356,#20813);
#53=ITEM_DEFINED_TRANSFORMATION($,$,#20356,#20814);
#54=ITEM_DEFINED_TRANSFORMATION($,$,#20356,#20815);
#55=ITEM_DEFINED_TRANSFORMATION($,$,#20356,#20816);
#56=ITEM_DEFINED_TRANSFORMATION($,$,#20356,#20817);
#57=ITEM_DEFINED_TRANSFORMATION($,$,#19920,#20818);
#58=ITEM_DEFINED_TRANSFORMATION($,$,#19930,#20819);
#59=ITEM_DEFINED_TRANSFORMATION($,$,#19968,#20820);
#60=ITEM_DEFINED_TRANSFORMATION($,$,#19968,#20821);
#61=ITEM_DEFINED_TRANSFORMATION($,$,#20764,#20822);
#62=ITEM_DEFINED_TRANSFORMATION($,$,#20356,#20823);
#63=ITEM_DEFINED_TRANSFORMATION($,$,#20356,#20824);
#64=ITEM_DEFINED_TRANSFORMATION($,$,#19930,#20825);
#65=ITEM_DEFINED_TRANSFORMATION($,$,#19968,#20826);
#66=ITEM_DEFINED_TRANSFORMATION($,$,#19968,#20827);
#67=ITEM_DEFINED_TRANSFORMATION($,$,#20764,#20828);
#68=ITEM_DEFINED_TRANSFORMATION($,$,#20356,#20829);
#69=ITEM_DEFINED_TRANSFORMATION($,$,#20356,#20830);
#70=ITEM_DEFINED_TRANSFORMATION($,$,#19920,#20831);
#71=ITEM_DEFINED_TRANSFORMATION($,$,#19930,#20832);
#72=ITEM_DEFINED_TRANSFORMATION($,$,#19968,#20833);
#73=ITEM_DEFINED_TRANSFORMATION($,$,#19968,#20834);
#74=ITEM_DEFINED_TRANSFORMATION($,$,#20764,#20835);
#75=ITEM_DEFINED_TRANSFORMATION($,$,#20356,#20836);
#76=ITEM_DEFINED_TRANSFORMATION($,$,#20356,#20837);
#77=ITEM_DEFINED_TRANSFORMATION($,$,#19930,#20838);
#78=ITEM_DEFINED_TRANSFORMATION($,$,#19968,#20839);
#79=ITEM_DEFINED_TRANSFORMATION($,$,#19968,#20840);
#80=ITEM_DEFINED_TRANSFORMATION($,$,#20764,#20841);
#81=ITEM_DEFINED_TRANSFORMATION($,$,#20356,#20842);
#82=ITEM_DEFINED_TRANSFORMATION($,$,#20356,#20843);
#83=ITEM_DEFINED_TRANSFORMATION($,$,#19992,#20844);
#84=ITEM_DEFINED_TRANSFORMATION($,$,#20356,#20845);
#85=ITEM_DEFINED_TRANSFORMATION($,$,#20356,#20846);
#86=ITEM_DEFINED_TRANSFORMATION($,$,#20356,#20847);
#87=ITEM_DEFINED_TRANSFORMATION($,$,#20356,#20848);
#88=ITEM_DEFINED_TRANSFORMATION($,$,#20120,#20849);
#89=ITEM_DEFINED_TRANSFORMATION($,$,#20356,#20850);
#90=ITEM_DEFINED_TRANSFORMATION($,$,#20356,#20851);
#91=ITEM_DEFINED_TRANSFORMATION($,$,#20356,#20852);
#92=ITEM_DEFINED_TRANSFORMATION($,$,#20356,#20853);
#93=ITEM_DEFINED_TRANSFORMATION($,$,#20764,#20854);
#94=ITEM_DEFINED_TRANSFORMATION($,$,#20764,#20855);
#95=ITEM_DEFINED_TRANSFORMATION($,$,#20764,#20856);
#96=ITEM_DEFINED_TRANSFORMATION($,$,#20764,#20857);
#97=ITEM_DEFINED_TRANSFORMATION($,$,#20764,#20858);
#98=ITEM_DEFINED_TRANSFORMATION($,$,#20764,#20859);
#99=ITEM_DEFINED_TRANSFORMATION($,$,#20356,#20860);
#100=ITEM_DEFINED_TRANSFORMATION($,$,#20254,#20861);
#101=ITEM_DEFINED_TRANSFORMATION($,$,#20356,#20862);
#102=ITEM_DEFINED_TRANSFORMATION($,$,#20254,#20863);
#103=ITEM_DEFINED_TRANSFORMATION($,$,#20282,#20864);
#104=ITEM_DEFINED_TRANSFORMATION($,$,#20282,#20865);
#105=ITEM_DEFINED_TRANSFORMATION($,$,#20282,#20866);
#106=ITEM_DEFINED_TRANSFORMATION($,$,#20282,#20867);
#107=ITEM_DEFINED_TRANSFORMATION($,$,#20306,#20868);
#108=ITEM_DEFINED_TRANSFORMATION($,$,#20356,#20869);
#109=ITEM_DEFINED_TRANSFORMATION($,$,#20382,#20870);
#110=ITEM_DEFINED_TRANSFORMATION($,$,#20403,#20871);
#111=ITEM_DEFINED_TRANSFORMATION($,$,#20382,#20872);
#112=ITEM_DEFINED_TRANSFORMATION($,$,#20403,#20873);
#113=ITEM_DEFINED_TRANSFORMATION($,$,#20427,#20874);
#114=ITEM_DEFINED_TRANSFORMATION($,$,#20488,#20875);
#115=ITEM_DEFINED_TRANSFORMATION($,$,#20537,#20876);
#116=ITEM_DEFINED_TRANSFORMATION($,$,#20586,#20877);
#117=ITEM_DEFINED_TRANSFORMATION($,$,#20607,#20878);
#118=ITEM_DEFINED_TRANSFORMATION($,$,#20619,#20879);
#119=ITEM_DEFINED_TRANSFORMATION($,$,#20639,#20880);
#120=ITEM_DEFINED_TRANSFORMATION($,$,#20764,#20881);
#121=ITEM_DEFINED_TRANSFORMATION($,$,#20764,#20882);
#122=ITEM_DEFINED_TRANSFORMATION($,$,#20764,#20883);
#123=ITEM_DEFINED_TRANSFORMATION($,$,#20764,#20884);
#124=ITEM_DEFINED_TRANSFORMATION($,$,#20639,#20885);
#125=ITEM_DEFINED_TRANSFORMATION($,$,#20764,#20886);
#126=ITEM_DEFINED_TRANSFORMATION($,$,#20764,#20887);
#127=ITEM_DEFINED_TRANSFORMATION($,$,#20764,#20888);
#128=ITEM_DEFINED_TRANSFORMATION($,$,#20764,#20889);
#129=ITEM_DEFINED_TRANSFORMATION($,$,#20691,#20890);
#130=ITEM_DEFINED_TRANSFORMATION($,$,#20736,#20891);
#131=ITEM_DEFINED_TRANSFORMATION($,$,#20736,#20892);
#132=ITEM_DEFINED_TRANSFORMATION($,$,#20736,#20893);
#133=ITEM_DEFINED_TRANSFORMATION($,$,#20764,#20894);
#134=ITEM_DEFINED_TRANSFORMATION($,$,#20764,#20895);
#135=ITEM_DEFINED_TRANSFORMATION($,$,#20764,#20896);
#136=ITEM_DEFINED_TRANSFORMATION($,$,#20764,#20897);
#137=ITEM_DEFINED_TRANSFORMATION($,$,#20899,#21182);
#138=ITEM_DEFINED_TRANSFORMATION($,$,#21054,#21183);
#139=ITEM_DEFINED_TRANSFORMATION($,$,#21063,#21184);
#140=ITEM_DEFINED_TRANSFORMATION($,$,#21077,#21185);
#141=ITEM_DEFINED_TRANSFORMATION($,$,#21101,#21186);
#142=ITEM_DEFINED_TRANSFORMATION($,$,#21110,#21187);
#143=ITEM_DEFINED_TRANSFORMATION($,$,#21119,#21188);
#144=ITEM_DEFINED_TRANSFORMATION($,$,#21130,#21189);
#145=ITEM_DEFINED_TRANSFORMATION($,$,#21130,#21190);
#146=ITEM_DEFINED_TRANSFORMATION($,$,#21147,#21191);
#147=ITEM_DEFINED_TRANSFORMATION($,$,#21156,#21192);
#148=ITEM_DEFINED_TRANSFORMATION($,$,#19285,#21193);
#149=ITEM_DEFINED_TRANSFORMATION($,$,#20426,#21194);
#150=ITEM_DEFINED_TRANSFORMATION($,$,#20898,#21195);
#151=(
REPRESENTATION_RELATIONSHIP($,$,#43820,#43819)
REPRESENTATION_RELATIONSHIP_WITH_TRANSFORMATION(#17)
SHAPE_REPRESENTATION_RELATIONSHIP()
);
#152=(
REPRESENTATION_RELATIONSHIP($,$,#43821,#43819)
REPRESENTATION_RELATIONSHIP_WITH_TRANSFORMATION(#18)
SHAPE_REPRESENTATION_RELATIONSHIP()
);
#153=(
REPRESENTATION_RELATIONSHIP($,$,#43822,#43819)
REPRESENTATION_RELATIONSHIP_WITH_TRANSFORMATION(#19)
SHAPE_REPRESENTATION_RELATIONSHIP()
);
#154=(
REPRESENTATION_RELATIONSHIP($,$,#43823,#43819)
REPRESENTATION_RELATIONSHIP_WITH_TRANSFORMATION(#20)
SHAPE_REPRESENTATION_RELATIONSHIP()
);
#155=(
REPRESENTATION_RELATIONSHIP($,$,#43824,#43819)
REPRESENTATION_RELATIONSHIP_WITH_TRANSFORMATION(#21)
SHAPE_REPRESENTATION_RELATIONSHIP()
);
#156=(
REPRESENTATION_RELATIONSHIP($,$,#43826,#43825)
REPRESENTATION_RELATIONSHIP_WITH_TRANSFORMATION(#22)
SHAPE_REPRESENTATION_RELATIONSHIP()
);
#157=(
REPRESENTATION_RELATIONSHIP($,$,#43827,#43825)
REPRESENTATION_RELATIONSHIP_WITH_TRANSFORMATION(#23)
SHAPE_REPRESENTATION_RELATIONSHIP()
);
#158=(
REPRESENTATION_RELATIONSHIP($,$,#43828,#43825)
REPRESENTATION_RELATIONSHIP_WITH_TRANSFORMATION(#24)
SHAPE_REPRESENTATION_RELATIONSHIP()
);
#159=(
REPRESENTATION_RELATIONSHIP($,$,#43829,#43825)
REPRESENTATION_RELATIONSHIP_WITH_TRANSFORMATION(#25)
SHAPE_REPRESENTATION_RELATIONSHIP()
);
#160=(
REPRESENTATION_RELATIONSHIP($,$,#43830,#43825)
REPRESENTATION_RELATIONSHIP_WITH_TRANSFORMATION(#26)
SHAPE_REPRESENTATION_RELATIONSHIP()
);
#161=(
REPRESENTATION_RELATIONSHIP($,$,#43845,#43844)
REPRESENTATION_RELATIONSHIP_WITH_TRANSFORMATION(#27)
SHAPE_REPRESENTATION_RELATIONSHIP()
);
#162=(
REPRESENTATION_RELATIONSHIP($,$,#43846,#43844)
REPRESENTATION_RELATIONSHIP_WITH_TRANSFORMATION(#28)
SHAPE_REPRESENTATION_RELATIONSHIP()
);
#163=(
REPRESENTATION_RELATIONSHIP($,$,#43796,#43795)
REPRESENTATION_RELATIONSHIP_WITH_TRANSFORMATION(#29)
SHAPE_REPRESENTATION_RELATIONSHIP()
);
#164=(
REPRESENTATION_RELATIONSHIP($,$,#43797,#43795)
REPRESENTATION_RELATIONSHIP_WITH_TRANSFORMATION(#30)
SHAPE_REPRESENTATION_RELATIONSHIP()
);
#165=(
REPRESENTATION_RELATIONSHIP($,$,#43798,#43795)
REPRESENTATION_RELATIONSHIP_WITH_TRANSFORMATION(#31)
SHAPE_REPRESENTATION_RELATIONSHIP()
);
#166=(
REPRESENTATION_RELATIONSHIP($,$,#43799,#43795)
REPRESENTATION_RELATIONSHIP_WITH_TRANSFORMATION(#32)
SHAPE_REPRESENTATION_RELATIONSHIP()
);
#167=(
REPRESENTATION_RELATIONSHIP($,$,#43800,#43795)
REPRESENTATION_RELATIONSHIP_WITH_TRANSFORMATION(#33)
SHAPE_REPRESENTATION_RELATIONSHIP()
);
#168=(
REPRESENTATION_RELATIONSHIP($,$,#43801,#43795)
REPRESENTATION_RELATIONSHIP_WITH_TRANSFORMATION(#34)
SHAPE_REPRESENTATION_RELATIONSHIP()
);
#169=(
REPRESENTATION_RELATIONSHIP($,$,#43802,#43795)
REPRESENTATION_RELATIONSHIP_WITH_TRANSFORMATION(#35)
SHAPE_REPRESENTATION_RELATIONSHIP()
);
#170=(
REPRESENTATION_RELATIONSHIP($,$,#43803,#43795)
REPRESENTATION_RELATIONSHIP_WITH_TRANSFORMATION(#36)
SHAPE_REPRESENTATION_RELATIONSHIP()
);
#171=(
REPRESENTATION_RELATIONSHIP($,$,#43804,#43795)
REPRESENTATION_RELATIONSHIP_WITH_TRANSFORMATION(#37)
SHAPE_REPRESENTATION_RELATIONSHIP()
);
#172=(
REPRESENTATION_RELATIONSHIP($,$,#43805,#43795)
REPRESENTATION_RELATIONSHIP_WITH_TRANSFORMATION(#38)
SHAPE_REPRESENTATION_RELATIONSHIP()
);
#173=(
REPRESENTATION_RELATIONSHIP($,$,#43806,#43795)
REPRESENTATION_RELATIONSHIP_WITH_TRANSFORMATION(#39)
SHAPE_REPRESENTATION_RELATIONSHIP()
);
#174=(
REPRESENTATION_RELATIONSHIP($,$,#43807,#43795)
REPRESENTATION_RELATIONSHIP_WITH_TRANSFORMATION(#40)
SHAPE_REPRESENTATION_RELATIONSHIP()
);
#175=(
REPRESENTATION_RELATIONSHIP($,$,#43808,#43795)
REPRESENTATION_RELATIONSHIP_WITH_TRANSFORMATION(#41)
SHAPE_REPRESENTATION_RELATIONSHIP()
);
#176=(
REPRESENTATION_RELATIONSHIP($,$,#43809,#43795)
REPRESENTATION_RELATIONSHIP_WITH_TRANSFORMATION(#42)
SHAPE_REPRESENTATION_RELATIONSHIP()
);
#177=(
REPRESENTATION_RELATIONSHIP($,$,#43810,#43795)
REPRESENTATION_RELATIONSHIP_WITH_TRANSFORMATION(#43)
SHAPE_REPRESENTATION_RELATIONSHIP()
);
#178=(
REPRESENTATION_RELATIONSHIP($,$,#43811,#43795)
REPRESENTATION_RELATIONSHIP_WITH_TRANSFORMATION(#44)
SHAPE_REPRESENTATION_RELATIONSHIP()
);
#179=(
REPRESENTATION_RELATIONSHIP($,$,#43812,#43795)
REPRESENTATION_RELATIONSHIP_WITH_TRANSFORMATION(#45)
SHAPE_REPRESENTATION_RELATIONSHIP()
);
#180=(
REPRESENTATION_RELATIONSHIP($,$,#43813,#43795)
REPRESENTATION_RELATIONSHIP_WITH_TRANSFORMATION(#46)
SHAPE_REPRESENTATION_RELATIONSHIP()
);
#181=(
REPRESENTATION_RELATIONSHIP($,$,#43814,#43795)
REPRESENTATION_RELATIONSHIP_WITH_TRANSFORMATION(#47)
SHAPE_REPRESENTATION_RELATIONSHIP()
);
#182=(
REPRESENTATION_RELATIONSHIP($,$,#43815,#43795)
REPRESENTATION_RELATIONSHIP_WITH_TRANSFORMATION(#48)
SHAPE_REPRESENTATION_RELATIONSHIP()
);
#183=(
REPRESENTATION_RELATIONSHIP($,$,#43834,#43795)
REPRESENTATION_RELATIONSHIP_WITH_TRANSFORMATION(#49)
SHAPE_REPRESENTATION_RELATIONSHIP()
);
#184=(
REPRESENTATION_RELATIONSHIP($,$,#43834,#43795)
REPRESENTATION_RELATIONSHIP_WITH_TRANSFORMATION(#50)
SHAPE_REPRESENTATION_RELATIONSHIP()
);
#185=(
REPRESENTATION_RELATIONSHIP($,$,#43834,#43795)
REPRESENTATION_RELATIONSHIP_WITH_TRANSFORMATION(#51)
SHAPE_REPRESENTATION_RELATIONSHIP()
);
#186=(
REPRESENTATION_RELATIONSHIP($,$,#43834,#43795)
REPRESENTATION_RELATIONSHIP_WITH_TRANSFORMATION(#52)
SHAPE_REPRESENTATION_RELATIONSHIP()
);
#187=(
REPRESENTATION_RELATIONSHIP($,$,#43834,#43795)
REPRESENTATION_RELATIONSHIP_WITH_TRANSFORMATION(#53)
SHAPE_REPRESENTATION_RELATIONSHIP()
);
#188=(
REPRESENTATION_RELATIONSHIP($,$,#43834,#43795)
REPRESENTATION_RELATIONSHIP_WITH_TRANSFORMATION(#54)
SHAPE_REPRESENTATION_RELATIONSHIP()
);
#189=(
REPRESENTATION_RELATIONSHIP($,$,#43834,#43795)
REPRESENTATION_RELATIONSHIP_WITH_TRANSFORMATION(#55)
SHAPE_REPRESENTATION_RELATIONSHIP()
);
#190=(
REPRESENTATION_RELATIONSHIP($,$,#43834,#43795)
REPRESENTATION_RELATIONSHIP_WITH_TRANSFORMATION(#56)
SHAPE_REPRESENTATION_RELATIONSHIP()
);
#191=(
REPRESENTATION_RELATIONSHIP($,$,#43816,#43795)
REPRESENTATION_RELATIONSHIP_WITH_TRANSFORMATION(#57)
SHAPE_REPRESENTATION_RELATIONSHIP()
);
#192=(
REPRESENTATION_RELATIONSHIP($,$,#43817,#43795)
REPRESENTATION_RELATIONSHIP_WITH_TRANSFORMATION(#58)
SHAPE_REPRESENTATION_RELATIONSHIP()
);
#193=(
REPRESENTATION_RELATIONSHIP($,$,#43818,#43795)
REPRESENTATION_RELATIONSHIP_WITH_TRANSFORMATION(#59)
SHAPE_REPRESENTATION_RELATIONSHIP()
);
#194=(
REPRESENTATION_RELATIONSHIP($,$,#43818,#43795)
REPRESENTATION_RELATIONSHIP_WITH_TRANSFORMATION(#60)
SHAPE_REPRESENTATION_RELATIONSHIP()
);
#195=(
REPRESENTATION_RELATIONSHIP($,$,#43849,#43795)
REPRESENTATION_RELATIONSHIP_WITH_TRANSFORMATION(#61)
SHAPE_REPRESENTATION_RELATIONSHIP()
);
#196=(
REPRESENTATION_RELATIONSHIP($,$,#43834,#43795)
REPRESENTATION_RELATIONSHIP_WITH_TRANSFORMATION(#62)
SHAPE_REPRESENTATION_RELATIONSHIP()
);
#197=(
REPRESENTATION_RELATIONSHIP($,$,#43834,#43795)
REPRESENTATION_RELATIONSHIP_WITH_TRANSFORMATION(#63)
SHAPE_REPRESENTATION_RELATIONSHIP()
);
#198=(
REPRESENTATION_RELATIONSHIP($,$,#43817,#43795)
REPRESENTATION_RELATIONSHIP_WITH_TRANSFORMATION(#64)
SHAPE_REPRESENTATION_RELATIONSHIP()
);
#199=(
REPRESENTATION_RELATIONSHIP($,$,#43818,#43795)
REPRESENTATION_RELATIONSHIP_WITH_TRANSFORMATION(#65)
SHAPE_REPRESENTATION_RELATIONSHIP()
);
#200=(
REPRESENTATION_RELATIONSHIP($,$,#43818,#43795)
REPRESENTATION_RELATIONSHIP_WITH_TRANSFORMATION(#66)
SHAPE_REPRESENTATION_RELATIONSHIP()
);
#201=(
REPRESENTATION_RELATIONSHIP($,$,#43849,#43795)
REPRESENTATION_RELATIONSHIP_WITH_TRANSFORMATION(#67)
SHAPE_REPRESENTATION_RELATIONSHIP()
);
#202=(
REPRESENTATION_RELATIONSHIP($,$,#43834,#43795)
REPRESENTATION_RELATIONSHIP_WITH_TRANSFORMATION(#68)
SHAPE_REPRESENTATION_RELATIONSHIP()
);
#203=(
REPRESENTATION_RELATIONSHIP($,$,#43834,#43795)
REPRESENTATION_RELATIONSHIP_WITH_TRANSFORMATION(#69)
SHAPE_REPRESENTATION_RELATIONSHIP()
);
#204=(
REPRESENTATION_RELATIONSHIP($,$,#43816,#43795)
REPRESENTATION_RELATIONSHIP_WITH_TRANSFORMATION(#70)
SHAPE_REPRESENTATION_RELATIONSHIP()
);
#205=(
REPRESENTATION_RELATIONSHIP($,$,#43817,#43795)
REPRESENTATION_RELATIONSHIP_WITH_TRANSFORMATION(#71)
SHAPE_REPRESENTATION_RELATIONSHIP()
);
#206=(
REPRESENTATION_RELATIONSHIP($,$,#43818,#43795)
REPRESENTATION_RELATIONSHIP_WITH_TRANSFORMATION(#72)
SHAPE_REPRESENTATION_RELATIONSHIP()
);
#207=(
REPRESENTATION_RELATIONSHIP($,$,#43818,#43795)
REPRESENTATION_RELATIONSHIP_WITH_TRANSFORMATION(#73)
SHAPE_REPRESENTATION_RELATIONSHIP()
);
#208=(
REPRESENTATION_RELATIONSHIP($,$,#43849,#43795)
REPRESENTATION_RELATIONSHIP_WITH_TRANSFORMATION(#74)
SHAPE_REPRESENTATION_RELATIONSHIP()
);
#209=(
REPRESENTATION_RELATIONSHIP($,$,#43834,#43795)
REPRESENTATION_RELATIONSHIP_WITH_TRANSFORMATION(#75)
SHAPE_REPRESENTATION_RELATIONSHIP()
);
#210=(
REPRESENTATION_RELATIONSHIP($,$,#43834,#43795)
REPRESENTATION_RELATIONSHIP_WITH_TRANSFORMATION(#76)
SHAPE_REPRESENTATION_RELATIONSHIP()
);
#211=(
REPRESENTATION_RELATIONSHIP($,$,#43817,#43795)
REPRESENTATION_RELATIONSHIP_WITH_TRANSFORMATION(#77)
SHAPE_REPRESENTATION_RELATIONSHIP()
);
#212=(
REPRESENTATION_RELATIONSHIP($,$,#43818,#43795)
REPRESENTATION_RELATIONSHIP_WITH_TRANSFORMATION(#78)
SHAPE_REPRESENTATION_RELATIONSHIP()
);
#213=(
REPRESENTATION_RELATIONSHIP($,$,#43818,#43795)
REPRESENTATION_RELATIONSHIP_WITH_TRANSFORMATION(#79)
SHAPE_REPRESENTATION_RELATIONSHIP()
);
#214=(
REPRESENTATION_RELATIONSHIP($,$,#43849,#43795)
REPRESENTATION_RELATIONSHIP_WITH_TRANSFORMATION(#80)
SHAPE_REPRESENTATION_RELATIONSHIP()
);
#215=(
REPRESENTATION_RELATIONSHIP($,$,#43834,#43795)
REPRESENTATION_RELATIONSHIP_WITH_TRANSFORMATION(#81)
SHAPE_REPRESENTATION_RELATIONSHIP()
);
#216=(
REPRESENTATION_RELATIONSHIP($,$,#43834,#43795)
REPRESENTATION_RELATIONSHIP_WITH_TRANSFORMATION(#82)
SHAPE_REPRESENTATION_RELATIONSHIP()
);
#217=(
REPRESENTATION_RELATIONSHIP($,$,#43819,#43795)
REPRESENTATION_RELATIONSHIP_WITH_TRANSFORMATION(#83)
SHAPE_REPRESENTATION_RELATIONSHIP()
);
#218=(
REPRESENTATION_RELATIONSHIP($,$,#43834,#43795)
REPRESENTATION_RELATIONSHIP_WITH_TRANSFORMATION(#84)
SHAPE_REPRESENTATION_RELATIONSHIP()
);
#219=(
REPRESENTATION_RELATIONSHIP($,$,#43834,#43795)
REPRESENTATION_RELATIONSHIP_WITH_TRANSFORMATION(#85)
SHAPE_REPRESENTATION_RELATIONSHIP()
);
#220=(
REPRESENTATION_RELATIONSHIP($,$,#43834,#43795)
REPRESENTATION_RELATIONSHIP_WITH_TRANSFORMATION(#86)
SHAPE_REPRESENTATION_RELATIONSHIP()
);
#221=(
REPRESENTATION_RELATIONSHIP($,$,#43834,#43795)
REPRESENTATION_RELATIONSHIP_WITH_TRANSFORMATION(#87)
SHAPE_REPRESENTATION_RELATIONSHIP()
);
#222=(
REPRESENTATION_RELATIONSHIP($,$,#43825,#43795)
REPRESENTATION_RELATIONSHIP_WITH_TRANSFORMATION(#88)
SHAPE_REPRESENTATION_RELATIONSHIP()
);
#223=(
REPRESENTATION_RELATIONSHIP($,$,#43834,#43795)
REPRESENTATION_RELATIONSHIP_WITH_TRANSFORMATION(#89)
SHAPE_REPRESENTATION_RELATIONSHIP()
);
#224=(
REPRESENTATION_RELATIONSHIP($,$,#43834,#43795)
REPRESENTATION_RELATIONSHIP_WITH_TRANSFORMATION(#90)
SHAPE_REPRESENTATION_RELATIONSHIP()
);
#225=(
REPRESENTATION_RELATIONSHIP($,$,#43834,#43795)
REPRESENTATION_RELATIONSHIP_WITH_TRANSFORMATION(#91)
SHAPE_REPRESENTATION_RELATIONSHIP()
);
#226=(
REPRESENTATION_RELATIONSHIP($,$,#43834,#43795)
REPRESENTATION_RELATIONSHIP_WITH_TRANSFORMATION(#92)
SHAPE_REPRESENTATION_RELATIONSHIP()
);
#227=(
REPRESENTATION_RELATIONSHIP($,$,#43849,#43795)
REPRESENTATION_RELATIONSHIP_WITH_TRANSFORMATION(#93)
SHAPE_REPRESENTATION_RELATIONSHIP()
);
#228=(
REPRESENTATION_RELATIONSHIP($,$,#43849,#43795)
REPRESENTATION_RELATIONSHIP_WITH_TRANSFORMATION(#94)
SHAPE_REPRESENTATION_RELATIONSHIP()
);
#229=(
REPRESENTATION_RELATIONSHIP($,$,#43849,#43795)
REPRESENTATION_RELATIONSHIP_WITH_TRANSFORMATION(#95)
SHAPE_REPRESENTATION_RELATIONSHIP()
);
#230=(
REPRESENTATION_RELATIONSHIP($,$,#43849,#43795)
REPRESENTATION_RELATIONSHIP_WITH_TRANSFORMATION(#96)
SHAPE_REPRESENTATION_RELATIONSHIP()
);
#231=(
REPRESENTATION_RELATIONSHIP($,$,#43849,#43795)
REPRESENTATION_RELATIONSHIP_WITH_TRANSFORMATION(#97)
SHAPE_REPRESENTATION_RELATIONSHIP()
);
#232=(
REPRESENTATION_RELATIONSHIP($,$,#43849,#43795)
REPRESENTATION_RELATIONSHIP_WITH_TRANSFORMATION(#98)
SHAPE_REPRESENTATION_RELATIONSHIP()
);
#233=(
REPRESENTATION_RELATIONSHIP($,$,#43834,#43795)
REPRESENTATION_RELATIONSHIP_WITH_TRANSFORMATION(#99)
SHAPE_REPRESENTATION_RELATIONSHIP()
);
#234=(
REPRESENTATION_RELATIONSHIP($,$,#43831,#43795)
REPRESENTATION_RELATIONSHIP_WITH_TRANSFORMATION(#100)
SHAPE_REPRESENTATION_RELATIONSHIP()
);
#235=(
REPRESENTATION_RELATIONSHIP($,$,#43834,#43795)
REPRESENTATION_RELATIONSHIP_WITH_TRANSFORMATION(#101)
SHAPE_REPRESENTATION_RELATIONSHIP()
);
#236=(
REPRESENTATION_RELATIONSHIP($,$,#43831,#43795)
REPRESENTATION_RELATIONSHIP_WITH_TRANSFORMATION(#102)
SHAPE_REPRESENTATION_RELATIONSHIP()
);
#237=(
REPRESENTATION_RELATIONSHIP($,$,#43832,#43795)
REPRESENTATION_RELATIONSHIP_WITH_TRANSFORMATION(#103)
SHAPE_REPRESENTATION_RELATIONSHIP()
);
#238=(
REPRESENTATION_RELATIONSHIP($,$,#43832,#43795)
REPRESENTATION_RELATIONSHIP_WITH_TRANSFORMATION(#104)
SHAPE_REPRESENTATION_RELATIONSHIP()
);
#239=(
REPRESENTATION_RELATIONSHIP($,$,#43832,#43795)
REPRESENTATION_RELATIONSHIP_WITH_TRANSFORMATION(#105)
SHAPE_REPRESENTATION_RELATIONSHIP()
);
#240=(
REPRESENTATION_RELATIONSHIP($,$,#43832,#43795)
REPRESENTATION_RELATIONSHIP_WITH_TRANSFORMATION(#106)
SHAPE_REPRESENTATION_RELATIONSHIP()
);
#241=(
REPRESENTATION_RELATIONSHIP($,$,#43833,#43795)
REPRESENTATION_RELATIONSHIP_WITH_TRANSFORMATION(#107)
SHAPE_REPRESENTATION_RELATIONSHIP()
);
#242=(
REPRESENTATION_RELATIONSHIP($,$,#43834,#43795)
REPRESENTATION_RELATIONSHIP_WITH_TRANSFORMATION(#108)
SHAPE_REPRESENTATION_RELATIONSHIP()
);
#243=(
REPRESENTATION_RELATIONSHIP($,$,#43835,#43795)
REPRESENTATION_RELATIONSHIP_WITH_TRANSFORMATION(#109)
SHAPE_REPRESENTATION_RELATIONSHIP()
);
#244=(
REPRESENTATION_RELATIONSHIP($,$,#43836,#43795)
REPRESENTATION_RELATIONSHIP_WITH_TRANSFORMATION(#110)
SHAPE_REPRESENTATION_RELATIONSHIP()
);
#245=(
REPRESENTATION_RELATIONSHIP($,$,#43835,#43795)
REPRESENTATION_RELATIONSHIP_WITH_TRANSFORMATION(#111)
SHAPE_REPRESENTATION_RELATIONSHIP()
);
#246=(
REPRESENTATION_RELATIONSHIP($,$,#43836,#43795)
REPRESENTATION_RELATIONSHIP_WITH_TRANSFORMATION(#112)
SHAPE_REPRESENTATION_RELATIONSHIP()
);
#247=(
REPRESENTATION_RELATIONSHIP($,$,#43838,#43837)
REPRESENTATION_RELATIONSHIP_WITH_TRANSFORMATION(#113)
SHAPE_REPRESENTATION_RELATIONSHIP()
);
#248=(
REPRESENTATION_RELATIONSHIP($,$,#43839,#43837)
REPRESENTATION_RELATIONSHIP_WITH_TRANSFORMATION(#114)
SHAPE_REPRESENTATION_RELATIONSHIP()
);
#249=(
REPRESENTATION_RELATIONSHIP($,$,#43840,#43837)
REPRESENTATION_RELATIONSHIP_WITH_TRANSFORMATION(#115)
SHAPE_REPRESENTATION_RELATIONSHIP()
);
#250=(
REPRESENTATION_RELATIONSHIP($,$,#43841,#43837)
REPRESENTATION_RELATIONSHIP_WITH_TRANSFORMATION(#116)
SHAPE_REPRESENTATION_RELATIONSHIP()
);
#251=(
REPRESENTATION_RELATIONSHIP($,$,#43842,#43837)
REPRESENTATION_RELATIONSHIP_WITH_TRANSFORMATION(#117)
SHAPE_REPRESENTATION_RELATIONSHIP()
);
#252=(
REPRESENTATION_RELATIONSHIP($,$,#43843,#43837)
REPRESENTATION_RELATIONSHIP_WITH_TRANSFORMATION(#118)
SHAPE_REPRESENTATION_RELATIONSHIP()
);
#253=(
REPRESENTATION_RELATIONSHIP($,$,#43844,#43837)
REPRESENTATION_RELATIONSHIP_WITH_TRANSFORMATION(#119)
SHAPE_REPRESENTATION_RELATIONSHIP()
);
#254=(
REPRESENTATION_RELATIONSHIP($,$,#43849,#43837)
REPRESENTATION_RELATIONSHIP_WITH_TRANSFORMATION(#120)
SHAPE_REPRESENTATION_RELATIONSHIP()
);
#255=(
REPRESENTATION_RELATIONSHIP($,$,#43849,#43837)
REPRESENTATION_RELATIONSHIP_WITH_TRANSFORMATION(#121)
SHAPE_REPRESENTATION_RELATIONSHIP()
);
#256=(
REPRESENTATION_RELATIONSHIP($,$,#43849,#43837)
REPRESENTATION_RELATIONSHIP_WITH_TRANSFORMATION(#122)
SHAPE_REPRESENTATION_RELATIONSHIP()
);
#257=(
REPRESENTATION_RELATIONSHIP($,$,#43849,#43837)
REPRESENTATION_RELATIONSHIP_WITH_TRANSFORMATION(#123)
SHAPE_REPRESENTATION_RELATIONSHIP()
);
#258=(
REPRESENTATION_RELATIONSHIP($,$,#43844,#43837)
REPRESENTATION_RELATIONSHIP_WITH_TRANSFORMATION(#124)
SHAPE_REPRESENTATION_RELATIONSHIP()
);
#259=(
REPRESENTATION_RELATIONSHIP($,$,#43849,#43837)
REPRESENTATION_RELATIONSHIP_WITH_TRANSFORMATION(#125)
SHAPE_REPRESENTATION_RELATIONSHIP()
);
#260=(
REPRESENTATION_RELATIONSHIP($,$,#43849,#43837)
REPRESENTATION_RELATIONSHIP_WITH_TRANSFORMATION(#126)
SHAPE_REPRESENTATION_RELATIONSHIP()
);
#261=(
REPRESENTATION_RELATIONSHIP($,$,#43849,#43837)
REPRESENTATION_RELATIONSHIP_WITH_TRANSFORMATION(#127)
SHAPE_REPRESENTATION_RELATIONSHIP()
);
#262=(
REPRESENTATION_RELATIONSHIP($,$,#43849,#43837)
REPRESENTATION_RELATIONSHIP_WITH_TRANSFORMATION(#128)
SHAPE_REPRESENTATION_RELATIONSHIP()
);
#263=(
REPRESENTATION_RELATIONSHIP($,$,#43847,#43837)
REPRESENTATION_RELATIONSHIP_WITH_TRANSFORMATION(#129)
SHAPE_REPRESENTATION_RELATIONSHIP()
);
#264=(
REPRESENTATION_RELATIONSHIP($,$,#43848,#43837)
REPRESENTATION_RELATIONSHIP_WITH_TRANSFORMATION(#130)
SHAPE_REPRESENTATION_RELATIONSHIP()
);
#265=(
REPRESENTATION_RELATIONSHIP($,$,#43848,#43837)
REPRESENTATION_RELATIONSHIP_WITH_TRANSFORMATION(#131)
SHAPE_REPRESENTATION_RELATIONSHIP()
);
#266=(
REPRESENTATION_RELATIONSHIP($,$,#43848,#43837)
REPRESENTATION_RELATIONSHIP_WITH_TRANSFORMATION(#132)
SHAPE_REPRESENTATION_RELATIONSHIP()
);
#267=(
REPRESENTATION_RELATIONSHIP($,$,#43849,#43837)
REPRESENTATION_RELATIONSHIP_WITH_TRANSFORMATION(#133)
SHAPE_REPRESENTATION_RELATIONSHIP()
);
#268=(
REPRESENTATION_RELATIONSHIP($,$,#43849,#43837)
REPRESENTATION_RELATIONSHIP_WITH_TRANSFORMATION(#134)
SHAPE_REPRESENTATION_RELATIONSHIP()
);
#269=(
REPRESENTATION_RELATIONSHIP($,$,#43849,#43837)
REPRESENTATION_RELATIONSHIP_WITH_TRANSFORMATION(#135)
SHAPE_REPRESENTATION_RELATIONSHIP()
);
#270=(
REPRESENTATION_RELATIONSHIP($,$,#43849,#43837)
REPRESENTATION_RELATIONSHIP_WITH_TRANSFORMATION(#136)
SHAPE_REPRESENTATION_RELATIONSHIP()
);
#271=(
REPRESENTATION_RELATIONSHIP($,$,#43851,#43850)
REPRESENTATION_RELATIONSHIP_WITH_TRANSFORMATION(#137)
SHAPE_REPRESENTATION_RELATIONSHIP()
);
#272=(
REPRESENTATION_RELATIONSHIP($,$,#43852,#43850)
REPRESENTATION_RELATIONSHIP_WITH_TRANSFORMATION(#138)
SHAPE_REPRESENTATION_RELATIONSHIP()
);
#273=(
REPRESENTATION_RELATIONSHIP($,$,#43853,#43850)
REPRESENTATION_RELATIONSHIP_WITH_TRANSFORMATION(#139)
SHAPE_REPRESENTATION_RELATIONSHIP()
);
#274=(
REPRESENTATION_RELATIONSHIP($,$,#43854,#43850)
REPRESENTATION_RELATIONSHIP_WITH_TRANSFORMATION(#140)
SHAPE_REPRESENTATION_RELATIONSHIP()
);
#275=(
REPRESENTATION_RELATIONSHIP($,$,#43855,#43850)
REPRESENTATION_RELATIONSHIP_WITH_TRANSFORMATION(#141)
SHAPE_REPRESENTATION_RELATIONSHIP()
);
#276=(
REPRESENTATION_RELATIONSHIP($,$,#43856,#43850)
REPRESENTATION_RELATIONSHIP_WITH_TRANSFORMATION(#142)
SHAPE_REPRESENTATION_RELATIONSHIP()
);
#277=(
REPRESENTATION_RELATIONSHIP($,$,#43857,#43850)
REPRESENTATION_RELATIONSHIP_WITH_TRANSFORMATION(#143)
SHAPE_REPRESENTATION_RELATIONSHIP()
);
#278=(
REPRESENTATION_RELATIONSHIP($,$,#43858,#43850)
REPRESENTATION_RELATIONSHIP_WITH_TRANSFORMATION(#144)
SHAPE_REPRESENTATION_RELATIONSHIP()
);
#279=(
REPRESENTATION_RELATIONSHIP($,$,#43858,#43850)
REPRESENTATION_RELATIONSHIP_WITH_TRANSFORMATION(#145)
SHAPE_REPRESENTATION_RELATIONSHIP()
);
#280=(
REPRESENTATION_RELATIONSHIP($,$,#43859,#43850)
REPRESENTATION_RELATIONSHIP_WITH_TRANSFORMATION(#146)
SHAPE_REPRESENTATION_RELATIONSHIP()
);
#281=(
REPRESENTATION_RELATIONSHIP($,$,#43860,#43850)
REPRESENTATION_RELATIONSHIP_WITH_TRANSFORMATION(#147)
SHAPE_REPRESENTATION_RELATIONSHIP()
);
#282=(
REPRESENTATION_RELATIONSHIP($,$,#43795,#43794)
REPRESENTATION_RELATIONSHIP_WITH_TRANSFORMATION(#148)
SHAPE_REPRESENTATION_RELATIONSHIP()
);
#283=(
REPRESENTATION_RELATIONSHIP($,$,#43837,#43794)
REPRESENTATION_RELATIONSHIP_WITH_TRANSFORMATION(#149)
SHAPE_REPRESENTATION_RELATIONSHIP()
);
#284=(
REPRESENTATION_RELATIONSHIP($,$,#43850,#43794)
REPRESENTATION_RELATIONSHIP_WITH_TRANSFORMATION(#150)
SHAPE_REPRESENTATION_RELATIONSHIP()
);
#285=CONTEXT_DEPENDENT_SHAPE_REPRESENTATION(#151,#43624);
#286=CONTEXT_DEPENDENT_SHAPE_REPRESENTATION(#152,#43625);
#287=CONTEXT_DEPENDENT_SHAPE_REPRESENTATION(#153,#43626);
#288=CONTEXT_DEPENDENT_SHAPE_REPRESENTATION(#154,#43627);
#289=CONTEXT_DEPENDENT_SHAPE_REPRESENTATION(#155,#43628);
#290=CONTEXT_DEPENDENT_SHAPE_REPRESENTATION(#156,#43635);
#291=CONTEXT_DEPENDENT_SHAPE_REPRESENTATION(#157,#43636);
#292=CONTEXT_DEPENDENT_SHAPE_REPRESENTATION(#158,#43637);
#293=CONTEXT_DEPENDENT_SHAPE_REPRESENTATION(#159,#43638);
#294=CONTEXT_DEPENDENT_SHAPE_REPRESENTATION(#160,#43639);
#295=CONTEXT_DEPENDENT_SHAPE_REPRESENTATION(#161,#43656);
#296=CONTEXT_DEPENDENT_SHAPE_REPRESENTATION(#162,#43657);
#297=CONTEXT_DEPENDENT_SHAPE_REPRESENTATION(#163,#43661);
#298=CONTEXT_DEPENDENT_SHAPE_REPRESENTATION(#164,#43662);
#299=CONTEXT_DEPENDENT_SHAPE_REPRESENTATION(#165,#43663);
#300=CONTEXT_DEPENDENT_SHAPE_REPRESENTATION(#166,#43664);
#301=CONTEXT_DEPENDENT_SHAPE_REPRESENTATION(#167,#43665);
#302=CONTEXT_DEPENDENT_SHAPE_REPRESENTATION(#168,#43666);
#303=CONTEXT_DEPENDENT_SHAPE_REPRESENTATION(#169,#43667);
#304=CONTEXT_DEPENDENT_SHAPE_REPRESENTATION(#170,#43668);
#305=CONTEXT_DEPENDENT_SHAPE_REPRESENTATION(#171,#43669);
#306=CONTEXT_DEPENDENT_SHAPE_REPRESENTATION(#172,#43670);
#307=CONTEXT_DEPENDENT_SHAPE_REPRESENTATION(#173,#43671);
#308=CONTEXT_DEPENDENT_SHAPE_REPRESENTATION(#174,#43672);
#309=CONTEXT_DEPENDENT_SHAPE_REPRESENTATION(#175,#43673);
#310=CONTEXT_DEPENDENT_SHAPE_REPRESENTATION(#176,#43674);
#311=CONTEXT_DEPENDENT_SHAPE_REPRESENTATION(#177,#43675);
#312=CONTEXT_DEPENDENT_SHAPE_REPRESENTATION(#178,#43676);
#313=CONTEXT_DEPENDENT_SHAPE_REPRESENTATION(#179,#43677);
#314=CONTEXT_DEPENDENT_SHAPE_REPRESENTATION(#180,#43678);
#315=CONTEXT_DEPENDENT_SHAPE_REPRESENTATION(#181,#43679);
#316=CONTEXT_DEPENDENT_SHAPE_REPRESENTATION(#182,#43680);
#317=CONTEXT_DEPENDENT_SHAPE_REPRESENTATION(#183,#43681);
#318=CONTEXT_DEPENDENT_SHAPE_REPRESENTATION(#184,#43682);
#319=CONTEXT_DEPENDENT_SHAPE_REPRESENTATION(#185,#43683);
#320=CONTEXT_DEPENDENT_SHAPE_REPRESENTATION(#186,#43684);
#321=CONTEXT_DEPENDENT_SHAPE_REPRESENTATION(#187,#43685);
#322=CONTEXT_DEPENDENT_SHAPE_REPRESENTATION(#188,#43686);
#323=CONTEXT_DEPENDENT_SHAPE_REPRESENTATION(#189,#43687);
#324=CONTEXT_DEPENDENT_SHAPE_REPRESENTATION(#190,#43688);
#325=CONTEXT_DEPENDENT_SHAPE_REPRESENTATION(#191,#43689);
#326=CONTEXT_DEPENDENT_SHAPE_REPRESENTATION(#192,#43690);
#327=CONTEXT_DEPENDENT_SHAPE_REPRESENTATION(#193,#43691);
#328=CONTEXT_DEPENDENT_SHAPE_REPRESENTATION(#194,#43692);
#329=CONTEXT_DEPENDENT_SHAPE_REPRESENTATION(#195,#43693);
#330=CONTEXT_DEPENDENT_SHAPE_REPRESENTATION(#196,#43694);
#331=CONTEXT_DEPENDENT_SHAPE_REPRESENTATION(#197,#43695);
#332=CONTEXT_DEPENDENT_SHAPE_REPRESENTATION(#198,#43696);
#333=CONTEXT_DEPENDENT_SHAPE_REPRESENTATION(#199,#43697);
#334=CONTEXT_DEPENDENT_SHAPE_REPRESENTATION(#200,#43698);
#335=CONTEXT_DEPENDENT_SHAPE_REPRESENTATION(#201,#43699);
#336=CONTEXT_DEPENDENT_SHAPE_REPRESENTATION(#202,#43700);
#337=CONTEXT_DEPENDENT_SHAPE_REPRESENTATION(#203,#43701);
#338=CONTEXT_DEPENDENT_SHAPE_REPRESENTATION(#204,#43702);
#339=CONTEXT_DEPENDENT_SHAPE_REPRESENTATION(#205,#43703);
#340=CONTEXT_DEPENDENT_SHAPE_REPRESENTATION(#206,#43704);
#341=CONTEXT_DEPENDENT_SHAPE_REPRESENTATION(#207,#43705);
#342=CONTEXT_DEPENDENT_SHAPE_REPRESENTATION(#208,#43706);
#343=CONTEXT_DEPENDENT_SHAPE_REPRESENTATION(#209,#43707);
#344=CONTEXT_DEPENDENT_SHAPE_REPRESENTATION(#210,#43708);
#345=CONTEXT_DEPENDENT_SHAPE_REPRESENTATION(#211,#43709);
#346=CONTEXT_DEPENDENT_SHAPE_REPRESENTATION(#212,#43710);
#347=CONTEXT_DEPENDENT_SHAPE_REPRESENTATION(#213,#43711);
#348=CONTEXT_DEPENDENT_SHAPE_REPRESENTATION(#214,#43712);
#349=CONTEXT_DEPENDENT_SHAPE_REPRESENTATION(#215,#43713);
#350=CONTEXT_DEPENDENT_SHAPE_REPRESENTATION(#216,#43714);
#351=CONTEXT_DEPENDENT_SHAPE_REPRESENTATION(#217,#43715);
#352=CONTEXT_DEPENDENT_SHAPE_REPRESENTATION(#218,#43716);
#353=CONTEXT_DEPENDENT_SHAPE_REPRESENTATION(#219,#43717);
#354=CONTEXT_DEPENDENT_SHAPE_REPRESENTATION(#220,#43718);
#355=CONTEXT_DEPENDENT_SHAPE_REPRESENTATION(#221,#43719);
#356=CONTEXT_DEPENDENT_SHAPE_REPRESENTATION(#222,#43720);
#357=CONTEXT_DEPENDENT_SHAPE_REPRESENTATION(#223,#43721);
#358=CONTEXT_DEPENDENT_SHAPE_REPRESENTATION(#224,#43722);
#359=CONTEXT_DEPENDENT_SHAPE_REPRESENTATION(#225,#43723);
#360=CONTEXT_DEPENDENT_SHAPE_REPRESENTATION(#226,#43724);
#361=CONTEXT_DEPENDENT_SHAPE_REPRESENTATION(#227,#43725);
#362=CONTEXT_DEPENDENT_SHAPE_REPRESENTATION(#228,#43726);
#363=CONTEXT_DEPENDENT_SHAPE_REPRESENTATION(#229,#43727);
#364=CONTEXT_DEPENDENT_SHAPE_REPRESENTATION(#230,#43728);
#365=CONTEXT_DEPENDENT_SHAPE_REPRESENTATION(#231,#43729);
#366=CONTEXT_DEPENDENT_SHAPE_REPRESENTATION(#232,#43730);
#367=CONTEXT_DEPENDENT_SHAPE_REPRESENTATION(#233,#43731);
#368=CONTEXT_DEPENDENT_SHAPE_REPRESENTATION(#234,#43732);
#369=CONTEXT_DEPENDENT_SHAPE_REPRESENTATION(#235,#43733);
#370=CONTEXT_DEPENDENT_SHAPE_REPRESENTATION(#236,#43734);
#371=CONTEXT_DEPENDENT_SHAPE_REPRESENTATION(#237,#43735);
#372=CONTEXT_DEPENDENT_SHAPE_REPRESENTATION(#238,#43736);
#373=CONTEXT_DEPENDENT_SHAPE_REPRESENTATION(#239,#43737);
#374=CONTEXT_DEPENDENT_SHAPE_REPRESENTATION(#240,#43738);
#375=CONTEXT_DEPENDENT_SHAPE_REPRESENTATION(#241,#43739);
#376=CONTEXT_DEPENDENT_SHAPE_REPRESENTATION(#242,#43740);
#377=CONTEXT_DEPENDENT_SHAPE_REPRESENTATION(#243,#43741);
#378=CONTEXT_DEPENDENT_SHAPE_REPRESENTATION(#244,#43742);
#379=CONTEXT_DEPENDENT_SHAPE_REPRESENTATION(#245,#43743);
#380=CONTEXT_DEPENDENT_SHAPE_REPRESENTATION(#246,#43744);
#381=CONTEXT_DEPENDENT_SHAPE_REPRESENTATION(#247,#43745);
#382=CONTEXT_DEPENDENT_SHAPE_REPRESENTATION(#248,#43746);
#383=CONTEXT_DEPENDENT_SHAPE_REPRESENTATION(#249,#43747);
#384=CONTEXT_DEPENDENT_SHAPE_REPRESENTATION(#250,#43748);
#385=CONTEXT_DEPENDENT_SHAPE_REPRESENTATION(#251,#43749);
#386=CONTEXT_DEPENDENT_SHAPE_REPRESENTATION(#252,#43750);
#387=CONTEXT_DEPENDENT_SHAPE_REPRESENTATION(#253,#43751);
#388=CONTEXT_DEPENDENT_SHAPE_REPRESENTATION(#254,#43752);
#389=CONTEXT_DEPENDENT_SHAPE_REPRESENTATION(#255,#43753);
#390=CONTEXT_DEPENDENT_SHAPE_REPRESENTATION(#256,#43754);
#391=CONTEXT_DEPENDENT_SHAPE_REPRESENTATION(#257,#43755);
#392=CONTEXT_DEPENDENT_SHAPE_REPRESENTATION(#258,#43756);
#393=CONTEXT_DEPENDENT_SHAPE_REPRESENTATION(#259,#43757);
#394=CONTEXT_DEPENDENT_SHAPE_REPRESENTATION(#260,#43758);
#395=CONTEXT_DEPENDENT_SHAPE_REPRESENTATION(#261,#43759);
#396=CONTEXT_DEPENDENT_SHAPE_REPRESENTATION(#262,#43760);
#397=CONTEXT_DEPENDENT_SHAPE_REPRESENTATION(#263,#43761);
#398=CONTEXT_DEPENDENT_SHAPE_REPRESENTATION(#264,#43762);
#399=CONTEXT_DEPENDENT_SHAPE_REPRESENTATION(#265,#43763);
#400=CONTEXT_DEPENDENT_SHAPE_REPRESENTATION(#266,#43764);
#401=CONTEXT_DEPENDENT_SHAPE_REPRESENTATION(#267,#43765);
#402=CONTEXT_DEPENDENT_SHAPE_REPRESENTATION(#268,#43766);
#403=CONTEXT_DEPENDENT_SHAPE_REPRESENTATION(#269,#43767);
#404=CONTEXT_DEPENDENT_SHAPE_REPRESENTATION(#270,#43768);
#405=CONTEXT_DEPENDENT_SHAPE_REPRESENTATION(#271,#43780);
#406=CONTEXT_DEPENDENT_SHAPE_REPRESENTATION(#272,#43781);
#407=CONTEXT_DEPENDENT_SHAPE_REPRESENTATION(#273,#43782);
#408=CONTEXT_DEPENDENT_SHAPE_REPRESENTATION(#274,#43783);
#409=CONTEXT_DEPENDENT_SHAPE_REPRESENTATION(#275,#43784);
#410=CONTEXT_DEPENDENT_SHAPE_REPRESENTATION(#276,#43785);
#411=CONTEXT_DEPENDENT_SHAPE_REPRESENTATION(#277,#43786);
#412=CONTEXT_DEPENDENT_SHAPE_REPRESENTATION(#278,#43787);
#413=CONTEXT_DEPENDENT_SHAPE_REPRESENTATION(#279,#43788);
#414=CONTEXT_DEPENDENT_SHAPE_REPRESENTATION(#280,#43789);
#415=CONTEXT_DEPENDENT_SHAPE_REPRESENTATION(#281,#43790);
#416=CONTEXT_DEPENDENT_SHAPE_REPRESENTATION(#282,#43791);
#417=CONTEXT_DEPENDENT_SHAPE_REPRESENTATION(#283,#43792);
#418=CONTEXT_DEPENDENT_SHAPE_REPRESENTATION(#284,#43793);
#419=NEXT_ASSEMBLY_USAGE_OCCURRENCE('Inner ring:1','Inner ring:1',
'Inner ring:1',#43887,#43888,'Inner ring:1');
#420=NEXT_ASSEMBLY_USAGE_OCCURRENCE('Outer ring:1','Outer ring:1',
'Outer ring:1',#43887,#43889,'Outer ring:1');
#421=NEXT_ASSEMBLY_USAGE_OCCURRENCE('Balls:1','Balls:1','Balls:1',#43887,
#43890,'Balls:1');
#422=NEXT_ASSEMBLY_USAGE_OCCURRENCE('Cage:1','Cage:1','Cage:1',#43887,#43891,
'Cage:1');
#423=NEXT_ASSEMBLY_USAGE_OCCURRENCE('Seals 2RS:1','Seals 2RS:1',
'Seals 2RS:1',#43887,#43892,'Seals 2RS:1');
#424=NEXT_ASSEMBLY_USAGE_OCCURRENCE('Inner ring (1):1',
'Inner ring (1):1','Inner ring (1):1',#43893,#43894,'Inner ring (1):1');
#425=NEXT_ASSEMBLY_USAGE_OCCURRENCE('Outer ring (1):1',
'Outer ring (1):1','Outer ring (1):1',#43893,#43895,'Outer ring (1):1');
#426=NEXT_ASSEMBLY_USAGE_OCCURRENCE('Balls (1):1','Balls (1):1',
'Balls (1):1',#43893,#43896,'Balls (1):1');
#427=NEXT_ASSEMBLY_USAGE_OCCURRENCE('Cage (1):1','Cage (1):1',
'Cage (1):1',#43893,#43897,'Cage (1):1');
#428=NEXT_ASSEMBLY_USAGE_OCCURRENCE('Seals 2RS (1):1','Seals 2RS (1):1',
'Seals 2RS (1):1',#43893,#43898,'Seals 2RS (1):1');
#429=NEXT_ASSEMBLY_USAGE_OCCURRENCE('Steel sleeve:1','Steel sleeve:1',
'Steel sleeve:1',#43912,#43913,'Steel sleeve:1');
#430=NEXT_ASSEMBLY_USAGE_OCCURRENCE('Ball retainer (plastic):1',
'Ball retainer (plastic):1','Ball retainer (plastic):1',#43912,#43914,
'Ball retainer (plastic):1');
#431=NEXT_ASSEMBLY_USAGE_OCCURRENCE('Base:1','Base:1','Base:1',#43863,#43864,
'Base:1');
#432=NEXT_ASSEMBLY_USAGE_OCCURRENCE('Foot strip:1','Foot strip:1',
'Foot strip:1',#43863,#43865,'Foot strip:1');
#433=NEXT_ASSEMBLY_USAGE_OCCURRENCE('Foot strip (1):1',
'Foot strip (1):1','Foot strip (1):1',#43863,#43866,'Foot strip (1):1');
#434=NEXT_ASSEMBLY_USAGE_OCCURRENCE('Top guide plate:1',
'Top guide plate:1','Top guide plate:1',#43863,#43867,
'Top guide plate:1');
#435=NEXT_ASSEMBLY_USAGE_OCCURRENCE('Frame upright:1','Frame upright:1',
'Frame upright:1',#43863,#43868,'Frame upright:1');
#436=NEXT_ASSEMBLY_USAGE_OCCURRENCE('Frame upright (1):1',
'Frame upright (1):1','Frame upright (1):1',#43863,#43869,
'Frame upright (1):1');
#437=NEXT_ASSEMBLY_USAGE_OCCURRENCE('Lower guide bracket:1',
'Lower guide bracket:1','Lower guide bracket:1',#43863,#43870,
'Lower guide bracket:1');
#438=NEXT_ASSEMBLY_USAGE_OCCURRENCE('Upper guide bracket:1',
'Upper guide bracket:1','Upper guide bracket:1',#43863,#43871,
'Upper guide bracket:1');
#439=NEXT_ASSEMBLY_USAGE_OCCURRENCE('Lower guide bracket (1):1',
'Lower guide bracket (1):1','Lower guide bracket (1):1',#43863,#43872,
'Lower guide bracket (1):1');
#440=NEXT_ASSEMBLY_USAGE_OCCURRENCE('Upper guide bracket (1):1',
'Upper guide bracket (1):1','Upper guide bracket (1):1',#43863,#43873,
'Upper guide bracket (1):1');
#441=NEXT_ASSEMBLY_USAGE_OCCURRENCE('Floating bearing pedestal:1',
'Floating bearing pedestal:1','Floating bearing pedestal:1',#43863,#43874,
'Floating bearing pedestal:1');
#442=NEXT_ASSEMBLY_USAGE_OCCURRENCE('Fixed bearing crossbar:1',
'Fixed bearing crossbar:1','Fixed bearing crossbar:1',#43863,#43875,
'Fixed bearing crossbar:1');
#443=NEXT_ASSEMBLY_USAGE_OCCURRENCE('Floating bearing cap:1',
'Floating bearing cap:1','Floating bearing cap:1',#43863,#43876,
'Floating bearing cap:1');
#444=NEXT_ASSEMBLY_USAGE_OCCURRENCE('Fixed bearing cap:1',
'Fixed bearing cap:1','Fixed bearing cap:1',#43863,#43877,
'Fixed bearing cap:1');
#445=NEXT_ASSEMBLY_USAGE_OCCURRENCE('Lower travel stop:1',
'Lower travel stop:1','Lower travel stop:1',#43863,#43878,
'Lower travel stop:1');
#446=NEXT_ASSEMBLY_USAGE_OCCURRENCE('Upper travel stop:1',
'Upper travel stop:1','Upper travel stop:1',#43863,#43879,
'Upper travel stop:1');
#447=NEXT_ASSEMBLY_USAGE_OCCURRENCE('Lower travel stop (1):1',
'Lower travel stop (1):1','Lower travel stop (1):1',#43863,#43880,
'Lower travel stop (1):1');
#448=NEXT_ASSEMBLY_USAGE_OCCURRENCE('Upper travel stop (1):1',
'Upper travel stop (1):1','Upper travel stop (1):1',#43863,#43881,
'Upper travel stop (1):1');
#449=NEXT_ASSEMBLY_USAGE_OCCURRENCE('Lower compression platen:1',
'Lower compression platen:1','Lower compression platen:1',#43863,#43882,
'Lower compression platen:1');
#450=NEXT_ASSEMBLY_USAGE_OCCURRENCE('Graduated scale:1',
'Graduated scale:1','Graduated scale:1',#43863,#43883,
'Graduated scale:1');
#451=NEXT_ASSEMBLY_USAGE_OCCURRENCE('Cap Screw - M5x20:2',
'Cap Screw - M5x20:2','Cap Screw - M5x20:2',#43863,#43902,
'Cap Screw - M5x20:2');
#452=NEXT_ASSEMBLY_USAGE_OCCURRENCE('Cap Screw - M5x20:3',
'Cap Screw - M5x20:3','Cap Screw - M5x20:3',#43863,#43902,
'Cap Screw - M5x20:3');
#453=NEXT_ASSEMBLY_USAGE_OCCURRENCE('Cap Screw - M5x20:4',
'Cap Screw - M5x20:4','Cap Screw - M5x20:4',#43863,#43902,
'Cap Screw - M5x20:4');
#454=NEXT_ASSEMBLY_USAGE_OCCURRENCE('Cap Screw - M5x20:5',
'Cap Screw - M5x20:5','Cap Screw - M5x20:5',#43863,#43902,
'Cap Screw - M5x20:5');
#455=NEXT_ASSEMBLY_USAGE_OCCURRENCE('Cap Screw - M5x20:6',
'Cap Screw - M5x20:6','Cap Screw - M5x20:6',#43863,#43902,
'Cap Screw - M5x20:6');
#456=NEXT_ASSEMBLY_USAGE_OCCURRENCE('Cap Screw - M5x20:7',
'Cap Screw - M5x20:7','Cap Screw - M5x20:7',#43863,#43902,
'Cap Screw - M5x20:7');
#457=NEXT_ASSEMBLY_USAGE_OCCURRENCE('Cap Screw - M5x20:8',
'Cap Screw - M5x20:8','Cap Screw - M5x20:8',#43863,#43902,
'Cap Screw - M5x20:8');
#458=NEXT_ASSEMBLY_USAGE_OCCURRENCE('Cap Screw - M5x20:9',
'Cap Screw - M5x20:9','Cap Screw - M5x20:9',#43863,#43902,
'Cap Screw - M5x20:9');
#459=NEXT_ASSEMBLY_USAGE_OCCURRENCE(
'Precision Shaft - 12 mm Diameter, 300 mm Long:2',
'Precision Shaft - 12 mm Diameter, 300 mm Long:2',
'Precision Shaft - 12 mm Diameter, 300 mm Long:2',#43863,#43884,
'Precision Shaft - 12 mm Diameter, 300 mm Long:2');
#460=NEXT_ASSEMBLY_USAGE_OCCURRENCE('Shaft Support - 12 mm Bore:2',
'Shaft Support - 12 mm Bore:2','Shaft Support - 12 mm Bore:2',#43863,#43885,
'Shaft Support - 12 mm Bore:2');
#461=NEXT_ASSEMBLY_USAGE_OCCURRENCE('M5x14 Cap Screw:2',
'M5x14 Cap Screw:2','M5x14 Cap Screw:2',#43863,#43886,
'M5x14 Cap Screw:2');
#462=NEXT_ASSEMBLY_USAGE_OCCURRENCE('M5x14 Cap Screw:3',
'M5x14 Cap Screw:3','M5x14 Cap Screw:3',#43863,#43886,
'M5x14 Cap Screw:3');
#463=NEXT_ASSEMBLY_USAGE_OCCURRENCE('Cap Screw - M4x16:2',
'Cap Screw - M4x16:2','Cap Screw - M4x16:2',#43863,#43917,
'Cap Screw - M4x16:2');
#464=NEXT_ASSEMBLY_USAGE_OCCURRENCE('Cap Screw - M5x20:10',
'Cap Screw - M5x20:10','Cap Screw - M5x20:10',#43863,#43902,
'Cap Screw - M5x20:10');
#465=NEXT_ASSEMBLY_USAGE_OCCURRENCE('Cap Screw - M5x20:11',
'Cap Screw - M5x20:11','Cap Screw - M5x20:11',#43863,#43902,
'Cap Screw - M5x20:11');
#466=NEXT_ASSEMBLY_USAGE_OCCURRENCE('Shaft Support - 12 mm Bore:3',
'Shaft Support - 12 mm Bore:3','Shaft Support - 12 mm Bore:3',#43863,#43885,
'Shaft Support - 12 mm Bore:3');
#467=NEXT_ASSEMBLY_USAGE_OCCURRENCE('M5x14 Cap Screw:4',
'M5x14 Cap Screw:4','M5x14 Cap Screw:4',#43863,#43886,
'M5x14 Cap Screw:4');
#468=NEXT_ASSEMBLY_USAGE_OCCURRENCE('M5x14 Cap Screw:5',
'M5x14 Cap Screw:5','M5x14 Cap Screw:5',#43863,#43886,
'M5x14 Cap Screw:5');
#469=NEXT_ASSEMBLY_USAGE_OCCURRENCE('Cap Screw - M4x16:3',
'Cap Screw - M4x16:3','Cap Screw - M4x16:3',#43863,#43917,
'Cap Screw - M4x16:3');
#470=NEXT_ASSEMBLY_USAGE_OCCURRENCE('Cap Screw - M5x20:12',
'Cap Screw - M5x20:12','Cap Screw - M5x20:12',#43863,#43902,
'Cap Screw - M5x20:12');
#471=NEXT_ASSEMBLY_USAGE_OCCURRENCE('Cap Screw - M5x20:13',
'Cap Screw - M5x20:13','Cap Screw - M5x20:13',#43863,#43902,
'Cap Screw - M5x20:13');
#472=NEXT_ASSEMBLY_USAGE_OCCURRENCE(
'Precision Shaft - 12 mm Diameter, 300 mm Long:3',
'Precision Shaft - 12 mm Diameter, 300 mm Long:3',
'Precision Shaft - 12 mm Diameter, 300 mm Long:3',#43863,#43884,
'Precision Shaft - 12 mm Diameter, 300 mm Long:3');
#473=NEXT_ASSEMBLY_USAGE_OCCURRENCE('Shaft Support - 12 mm Bore:4',
'Shaft Support - 12 mm Bore:4','Shaft Support - 12 mm Bore:4',#43863,#43885,
'Shaft Support - 12 mm Bore:4');
#474=NEXT_ASSEMBLY_USAGE_OCCURRENCE('M5x14 Cap Screw:6',
'M5x14 Cap Screw:6','M5x14 Cap Screw:6',#43863,#43886,
'M5x14 Cap Screw:6');
#475=NEXT_ASSEMBLY_USAGE_OCCURRENCE('M5x14 Cap Screw:7',
'M5x14 Cap Screw:7','M5x14 Cap Screw:7',#43863,#43886,
'M5x14 Cap Screw:7');
#476=NEXT_ASSEMBLY_USAGE_OCCURRENCE('Cap Screw - M4x16:4',
'Cap Screw - M4x16:4','Cap Screw - M4x16:4',#43863,#43917,
'Cap Screw - M4x16:4');
#477=NEXT_ASSEMBLY_USAGE_OCCURRENCE('Cap Screw - M5x20:14',
'Cap Screw - M5x20:14','Cap Screw - M5x20:14',#43863,#43902,
'Cap Screw - M5x20:14');
#478=NEXT_ASSEMBLY_USAGE_OCCURRENCE('Cap Screw - M5x20:15',
'Cap Screw - M5x20:15','Cap Screw - M5x20:15',#43863,#43902,
'Cap Screw - M5x20:15');
#479=NEXT_ASSEMBLY_USAGE_OCCURRENCE('Shaft Support - 12 mm Bore:5',
'Shaft Support - 12 mm Bore:5','Shaft Support - 12 mm Bore:5',#43863,#43885,
'Shaft Support - 12 mm Bore:5');
#480=NEXT_ASSEMBLY_USAGE_OCCURRENCE('M5x14 Cap Screw:8',
'M5x14 Cap Screw:8','M5x14 Cap Screw:8',#43863,#43886,
'M5x14 Cap Screw:8');
#481=NEXT_ASSEMBLY_USAGE_OCCURRENCE('M5x14 Cap Screw:9',
'M5x14 Cap Screw:9','M5x14 Cap Screw:9',#43863,#43886,
'M5x14 Cap Screw:9');
#482=NEXT_ASSEMBLY_USAGE_OCCURRENCE('Cap Screw - M4x16:5',
'Cap Screw - M4x16:5','Cap Screw - M4x16:5',#43863,#43917,
'Cap Screw - M4x16:5');
#483=NEXT_ASSEMBLY_USAGE_OCCURRENCE('Cap Screw - M5x20:16',
'Cap Screw - M5x20:16','Cap Screw - M5x20:16',#43863,#43902,
'Cap Screw - M5x20:16');
#484=NEXT_ASSEMBLY_USAGE_OCCURRENCE('Cap Screw - M5x20:17',
'Cap Screw - M5x20:17','Cap Screw - M5x20:17',#43863,#43902,
'Cap Screw - M5x20:17');
#485=NEXT_ASSEMBLY_USAGE_OCCURRENCE(
'Sealed Ball Bearing - 12 x 32 x 10 mm:2',
'Sealed Ball Bearing - 12 x 32 x 10 mm:2',
'Sealed Ball Bearing - 12 x 32 x 10 mm:2',#43863,#43887,
'Sealed Ball Bearing - 12 x 32 x 10 mm:2');
#486=NEXT_ASSEMBLY_USAGE_OCCURRENCE('Cap Screw - M5x20:18',
'Cap Screw - M5x20:18','Cap Screw - M5x20:18',#43863,#43902,
'Cap Screw - M5x20:18');
#487=NEXT_ASSEMBLY_USAGE_OCCURRENCE('Cap Screw - M5x20:19',
'Cap Screw - M5x20:19','Cap Screw - M5x20:19',#43863,#43902,
'Cap Screw - M5x20:19');
#488=NEXT_ASSEMBLY_USAGE_OCCURRENCE('Cap Screw - M5x20:20',
'Cap Screw - M5x20:20','Cap Screw - M5x20:20',#43863,#43902,
'Cap Screw - M5x20:20');
#489=NEXT_ASSEMBLY_USAGE_OCCURRENCE('Cap Screw - M5x20:21',
'Cap Screw - M5x20:21','Cap Screw - M5x20:21',#43863,#43902,
'Cap Screw - M5x20:21');
#490=NEXT_ASSEMBLY_USAGE_OCCURRENCE(
'Sealed Ball Bearing - 20 x 47 x 14 mm:2',
'Sealed Ball Bearing - 20 x 47 x 14 mm:2',
'Sealed Ball Bearing - 20 x 47 x 14 mm:2',#43863,#43893,
'Sealed Ball Bearing - 20 x 47 x 14 mm:2');
#491=NEXT_ASSEMBLY_USAGE_OCCURRENCE('Cap Screw - M5x20:22',
'Cap Screw - M5x20:22','Cap Screw - M5x20:22',#43863,#43902,
'Cap Screw - M5x20:22');
#492=NEXT_ASSEMBLY_USAGE_OCCURRENCE('Cap Screw - M5x20:23',
'Cap Screw - M5x20:23','Cap Screw - M5x20:23',#43863,#43902,
'Cap Screw - M5x20:23');
#493=NEXT_ASSEMBLY_USAGE_OCCURRENCE('Cap Screw - M5x20:24',
'Cap Screw - M5x20:24','Cap Screw - M5x20:24',#43863,#43902,
'Cap Screw - M5x20:24');
#494=NEXT_ASSEMBLY_USAGE_OCCURRENCE('Cap Screw - M5x20:25',
'Cap Screw - M5x20:25','Cap Screw - M5x20:25',#43863,#43902,
'Cap Screw - M5x20:25');
#495=NEXT_ASSEMBLY_USAGE_OCCURRENCE('Cap Screw - M4x16:14',
'Cap Screw - M4x16:14','Cap Screw - M4x16:14',#43863,#43917,
'Cap Screw - M4x16:14');
#496=NEXT_ASSEMBLY_USAGE_OCCURRENCE('Cap Screw - M4x16:15',
'Cap Screw - M4x16:15','Cap Screw - M4x16:15',#43863,#43917,
'Cap Screw - M4x16:15');
#497=NEXT_ASSEMBLY_USAGE_OCCURRENCE('Cap Screw - M4x16:16',
'Cap Screw - M4x16:16','Cap Screw - M4x16:16',#43863,#43917,
'Cap Screw - M4x16:16');
#498=NEXT_ASSEMBLY_USAGE_OCCURRENCE('Cap Screw - M4x16:17',
'Cap Screw - M4x16:17','Cap Screw - M4x16:17',#43863,#43917,
'Cap Screw - M4x16:17');
#499=NEXT_ASSEMBLY_USAGE_OCCURRENCE('Cap Screw - M4x16:18',
'Cap Screw - M4x16:18','Cap Screw - M4x16:18',#43863,#43917,
'Cap Screw - M4x16:18');
#500=NEXT_ASSEMBLY_USAGE_OCCURRENCE('Cap Screw - M4x16:19',
'Cap Screw - M4x16:19','Cap Screw - M4x16:19',#43863,#43917,
'Cap Screw - M4x16:19');
#501=NEXT_ASSEMBLY_USAGE_OCCURRENCE('Cap Screw - M5x20:26',
'Cap Screw - M5x20:26','Cap Screw - M5x20:26',#43863,#43902,
'Cap Screw - M5x20:26');
#502=NEXT_ASSEMBLY_USAGE_OCCURRENCE('M5x25 stop screw:2',
'M5x25 stop screw:2','M5x25 stop screw:2',#43863,#43899,
'M5x25 stop screw:2');
#503=NEXT_ASSEMBLY_USAGE_OCCURRENCE('Cap Screw - M5x20:27',
'Cap Screw - M5x20:27','Cap Screw - M5x20:27',#43863,#43902,
'Cap Screw - M5x20:27');
#504=NEXT_ASSEMBLY_USAGE_OCCURRENCE('M5x25 stop screw:3',
'M5x25 stop screw:3','M5x25 stop screw:3',#43863,#43899,
'M5x25 stop screw:3');
#505=NEXT_ASSEMBLY_USAGE_OCCURRENCE('M4x10 Cap Screw:2',
'M4x10 Cap Screw:2','M4x10 Cap Screw:2',#43863,#43900,
'M4x10 Cap Screw:2');
#506=NEXT_ASSEMBLY_USAGE_OCCURRENCE('M4x10 Cap Screw:3',
'M4x10 Cap Screw:3','M4x10 Cap Screw:3',#43863,#43900,
'M4x10 Cap Screw:3');
#507=NEXT_ASSEMBLY_USAGE_OCCURRENCE('M4x10 Cap Screw:4',
'M4x10 Cap Screw:4','M4x10 Cap Screw:4',#43863,#43900,
'M4x10 Cap Screw:4');
#508=NEXT_ASSEMBLY_USAGE_OCCURRENCE('M4x10 Cap Screw:5',
'M4x10 Cap Screw:5','M4x10 Cap Screw:5',#43863,#43900,
'M4x10 Cap Screw:5');
#509=NEXT_ASSEMBLY_USAGE_OCCURRENCE(
'Slotted Extrusion - 20 x 20 x 400 mm:2',
'Slotted Extrusion - 20 x 20 x 400 mm:2',
'Slotted Extrusion - 20 x 20 x 400 mm:2',#43863,#43901,
'Slotted Extrusion - 20 x 20 x 400 mm:2');
#510=NEXT_ASSEMBLY_USAGE_OCCURRENCE('Cap Screw - M5x20:28',
'Cap Screw - M5x20:28','Cap Screw - M5x20:28',#43863,#43902,
'Cap Screw - M5x20:28');
#511=NEXT_ASSEMBLY_USAGE_OCCURRENCE('Captive slot nut:2',
'Captive slot nut:2','Captive slot nut:2',#43863,#43903,
'Captive slot nut:2');
#512=NEXT_ASSEMBLY_USAGE_OCCURRENCE('M5x8 ruler screw:2',
'M5x8 ruler screw:2','M5x8 ruler screw:2',#43863,#43904,
'M5x8 ruler screw:2');
#513=NEXT_ASSEMBLY_USAGE_OCCURRENCE('Captive slot nut:3',
'Captive slot nut:3','Captive slot nut:3',#43863,#43903,
'Captive slot nut:3');
#514=NEXT_ASSEMBLY_USAGE_OCCURRENCE('M5x8 ruler screw:3',
'M5x8 ruler screw:3','M5x8 ruler screw:3',#43863,#43904,
'M5x8 ruler screw:3');
#515=NEXT_ASSEMBLY_USAGE_OCCURRENCE('Platform:1','Platform:1',
'Platform:1',#43905,#43906,'Platform:1');
#516=NEXT_ASSEMBLY_USAGE_OCCURRENCE('Linear bushing housing:1',
'Linear bushing housing:1','Linear bushing housing:1',#43905,#43907,
'Linear bushing housing:1');
#517=NEXT_ASSEMBLY_USAGE_OCCURRENCE('Linear bushing housing (1):1',
'Linear bushing housing (1):1','Linear bushing housing (1):1',#43905,#43908,
'Linear bushing housing (1):1');
#518=NEXT_ASSEMBLY_USAGE_OCCURRENCE('Nut carrier:1','Nut carrier:1',
'Nut carrier:1',#43905,#43909,'Nut carrier:1');
#519=NEXT_ASSEMBLY_USAGE_OCCURRENCE('Upper compression platen:1',
'Upper compression platen:1','Upper compression platen:1',#43905,#43910,
'Upper compression platen:1');
#520=NEXT_ASSEMBLY_USAGE_OCCURRENCE('Scale pointer:1','Scale pointer:1',
'Scale pointer:1',#43905,#43911,'Scale pointer:1');
#521=NEXT_ASSEMBLY_USAGE_OCCURRENCE(
'Linear Ball Bushing - 12 x 21 x 30 mm:2',
'Linear Ball Bushing - 12 x 21 x 30 mm:2',
'Linear Ball Bushing - 12 x 21 x 30 mm:2',#43905,#43912,
'Linear Ball Bushing - 12 x 21 x 30 mm:2');
#522=NEXT_ASSEMBLY_USAGE_OCCURRENCE('Cap Screw - M4x16:6',
'Cap Screw - M4x16:6','Cap Screw - M4x16:6',#43905,#43917,
'Cap Screw - M4x16:6');
#523=NEXT_ASSEMBLY_USAGE_OCCURRENCE('Cap Screw - M4x16:7',
'Cap Screw - M4x16:7','Cap Screw - M4x16:7',#43905,#43917,
'Cap Screw - M4x16:7');
#524=NEXT_ASSEMBLY_USAGE_OCCURRENCE('Cap Screw - M4x16:8',
'Cap Screw - M4x16:8','Cap Screw - M4x16:8',#43905,#43917,
'Cap Screw - M4x16:8');
#525=NEXT_ASSEMBLY_USAGE_OCCURRENCE('Cap Screw - M4x16:9',
'Cap Screw - M4x16:9','Cap Screw - M4x16:9',#43905,#43917,
'Cap Screw - M4x16:9');
#526=NEXT_ASSEMBLY_USAGE_OCCURRENCE(
'Linear Ball Bushing - 12 x 21 x 30 mm:3',
'Linear Ball Bushing - 12 x 21 x 30 mm:3',
'Linear Ball Bushing - 12 x 21 x 30 mm:3',#43905,#43912,
'Linear Ball Bushing - 12 x 21 x 30 mm:3');
#527=NEXT_ASSEMBLY_USAGE_OCCURRENCE('Cap Screw - M4x16:10',
'Cap Screw - M4x16:10','Cap Screw - M4x16:10',#43905,#43917,
'Cap Screw - M4x16:10');
#528=NEXT_ASSEMBLY_USAGE_OCCURRENCE('Cap Screw - M4x16:11',
'Cap Screw - M4x16:11','Cap Screw - M4x16:11',#43905,#43917,
'Cap Screw - M4x16:11');
#529=NEXT_ASSEMBLY_USAGE_OCCURRENCE('Cap Screw - M4x16:12',
'Cap Screw - M4x16:12','Cap Screw - M4x16:12',#43905,#43917,
'Cap Screw - M4x16:12');
#530=NEXT_ASSEMBLY_USAGE_OCCURRENCE('Cap Screw - M4x16:13',
'Cap Screw - M4x16:13','Cap Screw - M4x16:13',#43905,#43917,
'Cap Screw - M4x16:13');
#531=NEXT_ASSEMBLY_USAGE_OCCURRENCE('Flanged lead nut:2',
'Flanged lead nut:2','Flanged lead nut:2',#43905,#43915,
'Flanged lead nut:2');
#532=NEXT_ASSEMBLY_USAGE_OCCURRENCE('M4x30 nut screw:2',
'M4x30 nut screw:2','M4x30 nut screw:2',#43905,#43916,
'M4x30 nut screw:2');
#533=NEXT_ASSEMBLY_USAGE_OCCURRENCE('M4x30 nut screw:3',
'M4x30 nut screw:3','M4x30 nut screw:3',#43905,#43916,
'M4x30 nut screw:3');
#534=NEXT_ASSEMBLY_USAGE_OCCURRENCE('M4x30 nut screw:4',
'M4x30 nut screw:4','M4x30 nut screw:4',#43905,#43916,
'M4x30 nut screw:4');
#535=NEXT_ASSEMBLY_USAGE_OCCURRENCE('Cap Screw - M4x16:20',
'Cap Screw - M4x16:20','Cap Screw - M4x16:20',#43905,#43917,
'Cap Screw - M4x16:20');
#536=NEXT_ASSEMBLY_USAGE_OCCURRENCE('Cap Screw - M4x16:21',
'Cap Screw - M4x16:21','Cap Screw - M4x16:21',#43905,#43917,
'Cap Screw - M4x16:21');
#537=NEXT_ASSEMBLY_USAGE_OCCURRENCE('Cap Screw - M4x16:22',
'Cap Screw - M4x16:22','Cap Screw - M4x16:22',#43905,#43917,
'Cap Screw - M4x16:22');
#538=NEXT_ASSEMBLY_USAGE_OCCURRENCE('Cap Screw - M4x16:23',
'Cap Screw - M4x16:23','Cap Screw - M4x16:23',#43905,#43917,
'Cap Screw - M4x16:23');
#539=NEXT_ASSEMBLY_USAGE_OCCURRENCE('Supported TR12x3 screw:2',
'Supported TR12x3 screw:2','Supported TR12x3 screw:2',#43918,#43919,
'Supported TR12x3 screw:2');
#540=NEXT_ASSEMBLY_USAGE_OCCURRENCE('Inner race spacer:2',
'Inner race spacer:2','Inner race spacer:2',#43918,#43920,
'Inner race spacer:2');
#541=NEXT_ASSEMBLY_USAGE_OCCURRENCE('Shaft retaining collar:2',
'Shaft retaining collar:2','Shaft retaining collar:2',#43918,#43921,
'Shaft retaining collar:2');
#542=NEXT_ASSEMBLY_USAGE_OCCURRENCE('Handwheel:2','Handwheel:2',
'Handwheel:2',#43918,#43922,'Handwheel:2');
#543=NEXT_ASSEMBLY_USAGE_OCCURRENCE('Handle pivot sleeve:2',
'Handle pivot sleeve:2','Handle pivot sleeve:2',#43918,#43923,
'Handle pivot sleeve:2');
#544=NEXT_ASSEMBLY_USAGE_OCCURRENCE('Revolving handle:2',
'Revolving handle:2','Revolving handle:2',#43918,#43924,
'Revolving handle:2');
#545=NEXT_ASSEMBLY_USAGE_OCCURRENCE('Key 6x6x20:2','Key 6x6x20:2',
'Key 6x6x20:2',#43918,#43925,'Key 6x6x20:2');
#546=NEXT_ASSEMBLY_USAGE_OCCURRENCE('Socket Set Screw - M5x8:2',
'Socket Set Screw - M5x8:2','Socket Set Screw - M5x8:2',#43918,#43926,
'Socket Set Screw - M5x8:2');
#547=NEXT_ASSEMBLY_USAGE_OCCURRENCE('Socket Set Screw - M5x8:3',
'Socket Set Screw - M5x8:3','Socket Set Screw - M5x8:3',#43918,#43926,
'Socket Set Screw - M5x8:3');
#548=NEXT_ASSEMBLY_USAGE_OCCURRENCE('Flat Washer - M6:2',
'Flat Washer - M6:2','Flat Washer - M6:2',#43918,#43927,
'Flat Washer - M6:2');
#549=NEXT_ASSEMBLY_USAGE_OCCURRENCE('Cap Screw - M6x25:2',
'Cap Screw - M6x25:2','Cap Screw - M6x25:2',#43918,#43928,
'Cap Screw - M6x25:2');
#550=NEXT_ASSEMBLY_USAGE_OCCURRENCE('Guide frame and screw bearings:1',
'Guide frame and screw bearings:1','Guide frame and screw bearings:1',#43862,
#43863,'Guide frame and screw bearings:1');
#551=NEXT_ASSEMBLY_USAGE_OCCURRENCE('Platform and lead nut:1',
'Platform and lead nut:1','Platform and lead nut:1',#43862,#43905,
'Platform and lead nut:1');
#552=NEXT_ASSEMBLY_USAGE_OCCURRENCE('Vertical screw and handwheel:1',
'Vertical screw and handwheel:1','Vertical screw and handwheel:1',#43862,
#43918,'Vertical screw and handwheel:1');
#553=B_SPLINE_CURVE_WITH_KNOTS('',3,(#28592,#28593,#28594,#28595,#28596,
#28597,#28598,#28599,#28600,#28601,#28602,#28603,#28604,#28605,#28606,#28607,
#28608,#28609,#28610,#28611,#28612,#28613),.UNSPECIFIED.,.F.,.F.,(4,2,2,
2,2,2,2,2,2,2,4),(0.0591825211272536,0.157966726598481,0.236950089897721,
0.315933453196962,0.391576304923761,0.46721915665056,0.54286200837736,0.618504860104159,
0.697488223403399,0.77647158670264,0.875255792173867),.UNSPECIFIED.);
#554=B_SPLINE_CURVE_WITH_KNOTS('',3,(#28617,#28618,#28619,#28620,#28621,
#28622,#28623,#28624,#28625,#28626,#28627,#28628,#28629,#28630,#28631,#28632,
#28633,#28634,#28635,#28636,#28637,#28638),.UNSPECIFIED.,.F.,.F.,(4,2,2,
2,2,2,2,2,2,2,4),(0.0581119756758434,0.106553146291161,0.213106292582322,
0.30849933801665,0.386091982889075,0.4636846277615,0.541277272633925,0.61886991750635,
0.714262962940678,0.820816109231839,0.869257279847157),.UNSPECIFIED.);
#555=B_SPLINE_CURVE_WITH_KNOTS('',3,(#28644,#28645,#28646,#28647,#28648,
#28649,#28650,#28651,#28652,#28653,#28654,#28655,#28656,#28657,#28658,#28659,
#28660,#28661,#28662,#28663,#28664,#28665),.UNSPECIFIED.,.F.,.F.,(4,2,2,
2,2,2,2,2,2,2,4),(0.0581119756758434,0.106553146291161,0.213106292582322,
0.30849933801665,0.386091982889075,0.4636846277615,0.541277272633925,0.61886991750635,
0.714262962940679,0.820816109231839,0.869257279847157),.UNSPECIFIED.);
#556=B_SPLINE_CURVE_WITH_KNOTS('',3,(#28669,#28670,#28671,#28672,#28673,
#28674,#28675,#28676,#28677,#28678,#28679,#28680,#28681,#28682,#28683,#28684,
#28685,#28686,#28687,#28688,#28689,#28690),.UNSPECIFIED.,.F.,.F.,(4,2,2,
2,2,2,2,2,2,2,4),(0.0581119756758433,0.106553146291161,0.213106292582322,
0.308499338016649,0.386091982889075,0.4636846277615,0.541277272633925,0.61886991750635,
0.714262962940678,0.820816109231839,0.869257279847157),.UNSPECIFIED.);
#557=B_SPLINE_CURVE_WITH_KNOTS('',3,(#28699,#28700,#28701,#28702,#28703,
#28704,#28705,#28706,#28707,#28708,#28709,#28710,#28711,#28712,#28713,#28714,
#28715,#28716,#28717,#28718,#28719,#28720),.UNSPECIFIED.,.F.,.F.,(4,2,2,
2,2,2,2,2,2,2,4),(0.0581119756758433,0.106553146291161,0.213106292582322,
0.30849933801665,0.386091982889075,0.4636846277615,0.541277272633925,0.61886991750635,
0.714262962940678,0.820816109231839,0.869257279847157),.UNSPECIFIED.);
#558=B_SPLINE_CURVE_WITH_KNOTS('',3,(#28724,#28725,#28726,#28727,#28728,
#28729,#28730,#28731,#28732,#28733,#28734,#28735,#28736,#28737,#28738,#28739,
#28740,#28741,#28742,#28743,#28744,#28745),.UNSPECIFIED.,.F.,.F.,(4,2,2,
2,2,2,2,2,2,2,4),(0.0581119756758434,0.106553146291161,0.213106292582322,
0.30849933801665,0.386091982889075,0.4636846277615,0.541277272633925,0.61886991750635,
0.714262962940678,0.820816109231839,0.869257279847157),.UNSPECIFIED.);
#559=B_SPLINE_CURVE_WITH_KNOTS('',3,(#28749,#28750,#28751,#28752,#28753,
#28754,#28755,#28756,#28757,#28758,#28759,#28760,#28761,#28762,#28763,#28764,
#28765,#28766,#28767,#28768,#28769,#28770),.UNSPECIFIED.,.F.,.F.,(4,2,2,
2,2,2,2,2,2,2,4),(0.0581119756758434,0.106553146291161,0.213106292582322,
0.30849933801665,0.386091982889075,0.4636846277615,0.541277272633925,0.61886991750635,
0.714262962940678,0.820816109231839,0.869257279847157),.UNSPECIFIED.);
#560=B_SPLINE_CURVE_WITH_KNOTS('',3,(#28774,#28775,#28776,#28777,#28778,
#28779,#28780,#28781,#28782,#28783,#28784,#28785,#28786,#28787,#28788,#28789,
#28790,#28791,#28792,#28793,#28794,#28795),.UNSPECIFIED.,.F.,.F.,(4,2,2,
2,2,2,2,2,2,2,4),(0.0581119756758433,0.106553146291161,0.213106292582322,
0.30849933801665,0.386091982889075,0.4636846277615,0.541277272633925,0.61886991750635,
0.714262962940678,0.820816109231839,0.869257279847157),.UNSPECIFIED.);
#561=B_SPLINE_CURVE_WITH_KNOTS('',3,(#28803,#28804,#28805,#28806,#28807,
#28808,#28809,#28810,#28811,#28812,#28813,#28814,#28815,#28816,#28817,#28818,
#28819,#28820,#28821,#28822,#28823,#28824),.UNSPECIFIED.,.F.,.F.,(4,2,2,
2,2,2,2,2,2,2,4),(0.0591825211272536,0.157966726598481,0.236950089897721,
0.315933453196962,0.391576304923761,0.467219156650561,0.54286200837736,
0.618504860104159,0.697488223403399,0.77647158670264,0.875255792173867),
 .UNSPECIFIED.);
#562=B_SPLINE_CURVE_WITH_KNOTS('',3,(#28832,#28833,#28834,#28835,#28836,
#28837,#28838,#28839,#28840,#28841,#28842,#28843,#28844,#28845,#28846,#28847,
#28848,#28849,#28850,#28851,#28852,#28853),.UNSPECIFIED.,.F.,.F.,(4,2,2,
2,2,2,2,2,2,2,4),(0.0591825211272536,0.157966726598481,0.236950089897722,
0.315933453196962,0.391576304923761,0.467219156650561,0.54286200837736,
0.618504860104159,0.697488223403399,0.77647158670264,0.875255792173867),
 .UNSPECIFIED.);
#563=B_SPLINE_CURVE_WITH_KNOTS('',3,(#28863,#28864,#28865,#28866,#28867,
#28868,#28869,#28870,#28871,#28872,#28873,#28874,#28875,#28876,#28877,#28878,
#28879,#28880,#28881,#28882,#28883,#28884),.UNSPECIFIED.,.F.,.F.,(4,2,2,
2,2,2,2,2,2,2,4),(0.0591825211272536,0.157966726598481,0.236950089897721,
0.315933453196962,0.391576304923761,0.46721915665056,0.54286200837736,0.618504860104159,
0.697488223403399,0.77647158670264,0.875255792173867),.UNSPECIFIED.);
#564=B_SPLINE_CURVE_WITH_KNOTS('',3,(#28892,#28893,#28894,#28895,#28896,
#28897,#28898,#28899,#28900,#28901,#28902,#28903,#28904,#28905,#28906,#28907,
#28908,#28909,#28910,#28911,#28912,#28913),.UNSPECIFIED.,.F.,.F.,(4,2,2,
2,2,2,2,2,2,2,4),(0.0591825211272536,0.157966726598481,0.236950089897721,
0.315933453196962,0.391576304923761,0.46721915665056,0.542862008377359,
0.618504860104159,0.697488223403399,0.776471586702639,0.875255792173867),
 .UNSPECIFIED.);
#565=B_SPLINE_CURVE_WITH_KNOTS('',3,(#28921,#28922,#28923,#28924,#28925,
#28926,#28927,#28928,#28929,#28930,#28931,#28932,#28933,#28934,#28935,#28936,
#28937,#28938,#28939,#28940,#28941,#28942),.UNSPECIFIED.,.F.,.F.,(4,2,2,
2,2,2,2,2,2,2,4),(0.0591825211272536,0.157966726598481,0.236950089897721,
0.315933453196962,0.391576304923761,0.46721915665056,0.54286200837736,0.618504860104159,
0.697488223403399,0.77647158670264,0.875255792173867),.UNSPECIFIED.);
#566=B_SPLINE_CURVE_WITH_KNOTS('',3,(#28951,#28952,#28953,#28954,#28955,
#28956,#28957,#28958,#28959,#28960,#28961,#28962,#28963,#28964,#28965,#28966,
#28967,#28968,#28969,#28970,#28971,#28972),.UNSPECIFIED.,.F.,.F.,(4,2,2,
2,2,2,2,2,2,2,4),(0.0591825211272536,0.157966726598481,0.236950089897721,
0.315933453196962,0.391576304923761,0.46721915665056,0.542862008377359,
0.618504860104159,0.697488223403399,0.776471586702639,0.875255792173867),
 .UNSPECIFIED.);
#567=B_SPLINE_CURVE_WITH_KNOTS('',3,(#29122,#29123,#29124,#29125,#29126,
#29127,#29128,#29129,#29130,#29131,#29132,#29133,#29134,#29135,#29136,#29137,
#29138,#29139,#29140,#29141,#29142,#29143),.UNSPECIFIED.,.F.,.F.,(4,2,2,
2,2,2,2,2,2,2,4),(0.0789094028588958,0.210573405340968,0.315860108011452,
0.421146810681936,0.522142632548711,0.623138454415485,0.72413427628226,
0.825130098149035,0.930416800819519,1.03570350349,1.16736750597208),
 .UNSPECIFIED.);
#568=B_SPLINE_CURVE_WITH_KNOTS('',3,(#29147,#29148,#29149,#29150,#29151,
#29152,#29153,#29154,#29155,#29156,#29157,#29158,#29159,#29160,#29161,#29162,
#29163,#29164,#29165,#29166,#29167,#29168),.UNSPECIFIED.,.F.,.F.,(4,2,2,
2,2,2,2,2,2,2,4),(0.0774793363974613,0.142088896491891,0.284177792983782,
0.411119756996526,0.514392970548519,0.617666184100513,0.720939397652506,
0.8242126112045,0.951154575217244,1.09324347170913,1.15785303180356),
 .UNSPECIFIED.);
#569=B_SPLINE_CURVE_WITH_KNOTS('',3,(#29174,#29175,#29176,#29177,#29178,
#29179,#29180,#29181,#29182,#29183,#29184,#29185,#29186,#29187,#29188,#29189,
#29190,#29191,#29192,#29193,#29194,#29195),.UNSPECIFIED.,.F.,.F.,(4,2,2,
2,2,2,2,2,2,2,4),(0.0774793363974613,0.142088896491891,0.284177792983782,
0.411119756996525,0.514392970548519,0.617666184100513,0.720939397652506,
0.8242126112045,0.951154575217243,1.09324347170913,1.15785303180356),
 .UNSPECIFIED.);
#570=B_SPLINE_CURVE_WITH_KNOTS('',3,(#29199,#29200,#29201,#29202,#29203,
#29204,#29205,#29206,#29207,#29208,#29209,#29210,#29211,#29212,#29213,#29214,
#29215,#29216,#29217,#29218,#29219,#29220),.UNSPECIFIED.,.F.,.F.,(4,2,2,
2,2,2,2,2,2,2,4),(0.0774793363974614,0.142088896491891,0.284177792983781,
0.411119756996525,0.514392970548519,0.617666184100512,0.720939397652506,
0.824212611204499,0.951154575217243,1.09324347170913,1.15785303180356),
 .UNSPECIFIED.);
#571=B_SPLINE_CURVE_WITH_KNOTS('',3,(#29224,#29225,#29226,#29227,#29228,
#29229,#29230,#29231,#29232,#29233,#29234,#29235),.UNSPECIFIED.,.F.,.F.,
(4,2,2,2,2,4),(0.0774793363974613,0.142088896491891,0.284177792983781,0.411119756996525,
0.514392970548519,0.617666184100512),.UNSPECIFIED.);
#572=B_SPLINE_CURVE_WITH_KNOTS('',3,(#29240,#29241,#29242,#29243,#29244,
#29245,#29246,#29247,#29248,#29249,#29250,#29251),.UNSPECIFIED.,.F.,.F.,
(4,2,2,2,2,4),(0.617666184100512,0.720939397652506,0.824212611204499,0.951154575217243,
1.09324347170913,1.15785303180356),.UNSPECIFIED.);
#573=B_SPLINE_CURVE_WITH_KNOTS('',3,(#29255,#29256,#29257,#29258,#29259,
#29260,#29261,#29262,#29263,#29264,#29265,#29266,#29267,#29268,#29269,#29270,
#29271,#29272,#29273,#29274,#29275,#29276),.UNSPECIFIED.,.F.,.F.,(4,2,2,
2,2,2,2,2,2,2,4),(0.0774793363974613,0.142088896491891,0.284177792983782,
0.411119756996526,0.514392970548519,0.617666184100513,0.720939397652507,
0.8242126112045,0.951154575217245,1.09324347170914,1.15785303180356),
 .UNSPECIFIED.);
#574=B_SPLINE_CURVE_WITH_KNOTS('',3,(#29280,#29281,#29282,#29283,#29284,
#29285,#29286,#29287,#29288,#29289,#29290,#29291,#29292,#29293,#29294,#29295,
#29296,#29297,#29298,#29299,#29300,#29301),.UNSPECIFIED.,.F.,.F.,(4,2,2,
2,2,2,2,2,2,2,4),(0.0774793363974613,0.142088896491891,0.284177792983782,
0.411119756996526,0.514392970548519,0.617666184100513,0.720939397652506,
0.824212611204499,0.951154575217243,1.09324347170913,1.15785303180356),
 .UNSPECIFIED.);
#575=B_SPLINE_CURVE_WITH_KNOTS('',3,(#29305,#29306,#29307,#29308,#29309,
#29310,#29311,#29312,#29313,#29314,#29315,#29316,#29317,#29318,#29319,#29320,
#29321,#29322,#29323,#29324,#29325,#29326),.UNSPECIFIED.,.F.,.F.,(4,2,2,
2,2,2,2,2,2,2,4),(0.0774793363974613,0.142088896491891,0.284177792983782,
0.411119756996526,0.514392970548519,0.617666184100513,0.720939397652506,
0.8242126112045,0.951154575217244,1.09324347170913,1.15785303180356),
 .UNSPECIFIED.);
#576=B_SPLINE_CURVE_WITH_KNOTS('',3,(#29330,#29331,#29332,#29333,#29334,
#29335,#29336,#29337,#29338,#29339,#29340,#29341,#29342,#29343,#29344,#29345,
#29346,#29347,#29348,#29349,#29350,#29351),.UNSPECIFIED.,.F.,.F.,(4,2,2,
2,2,2,2,2,2,2,4),(0.0774793363974613,0.142088896491891,0.284177792983782,
0.411119756996526,0.514392970548519,0.617666184100513,0.720939397652506,
0.8242126112045,0.951154575217243,1.09324347170913,1.15785303180356),
 .UNSPECIFIED.);
#577=B_SPLINE_CURVE_WITH_KNOTS('',3,(#29359,#29360,#29361,#29362,#29363,
#29364,#29365,#29366,#29367,#29368,#29369,#29370,#29371,#29372,#29373,#29374,
#29375,#29376,#29377,#29378,#29379,#29380),.UNSPECIFIED.,.F.,.F.,(4,2,2,
2,2,2,2,2,2,2,4),(0.0789094028588958,0.210573405340968,0.315860108011452,
0.421146810681936,0.522142632548711,0.623138454415485,0.72413427628226,
0.825130098149035,0.930416800819519,1.03570350349,1.16736750597208),
 .UNSPECIFIED.);
#578=B_SPLINE_CURVE_WITH_KNOTS('',3,(#29388,#29389,#29390,#29391,#29392,
#29393,#29394,#29395,#29396,#29397,#29398,#29399,#29400,#29401,#29402,#29403,
#29404,#29405,#29406,#29407,#29408,#29409),.UNSPECIFIED.,.F.,.F.,(4,2,2,
2,2,2,2,2,2,2,4),(0.0789094028588958,0.210573405340969,0.315860108011453,
0.421146810681937,0.522142632548712,0.623138454415486,0.724134276282261,
0.825130098149035,0.930416800819519,1.03570350349,1.16736750597208),
 .UNSPECIFIED.);
#579=B_SPLINE_CURVE_WITH_KNOTS('',3,(#29418,#29419,#29420,#29421,#29422,
#29423,#29424,#29425,#29426,#29427,#29428,#29429),.UNSPECIFIED.,.F.,.F.,
(4,2,2,2,2,4),(0.0789094028588958,0.210573405340968,0.315860108011452,0.421146810681937,
0.522142632548711,0.623138454415486),.UNSPECIFIED.);
#580=B_SPLINE_CURVE_WITH_KNOTS('',3,(#29431,#29432,#29433,#29434,#29435,
#29436,#29437,#29438,#29439,#29440,#29441,#29442),.UNSPECIFIED.,.F.,.F.,
(4,2,2,2,2,4),(0.623138454415486,0.72413427628226,0.825130098149035,0.930416800819519,
1.03570350349,1.16736750597208),.UNSPECIFIED.);
#581=B_SPLINE_CURVE_WITH_KNOTS('',3,(#29449,#29450,#29451,#29452,#29453,
#29454,#29455,#29456,#29457,#29458,#29459,#29460,#29461,#29462,#29463,#29464,
#29465,#29466,#29467,#29468,#29469,#29470),.UNSPECIFIED.,.F.,.F.,(4,2,2,
2,2,2,2,2,2,2,4),(0.0789094028588958,0.210573405340968,0.315860108011452,
0.421146810681936,0.522142632548711,0.623138454415486,0.72413427628226,
0.825130098149035,0.930416800819519,1.03570350349,1.16736750597208),
 .UNSPECIFIED.);
#582=B_SPLINE_CURVE_WITH_KNOTS('',3,(#29478,#29479,#29480,#29481,#29482,
#29483,#29484,#29485,#29486,#29487,#29488,#29489,#29490,#29491,#29492,#29493,
#29494,#29495,#29496,#29497,#29498,#29499),.UNSPECIFIED.,.F.,.F.,(4,2,2,
2,2,2,2,2,2,2,4),(0.0789094028588957,0.210573405340968,0.315860108011452,
0.421146810681936,0.522142632548711,0.623138454415485,0.72413427628226,
0.825130098149035,0.930416800819519,1.03570350349,1.16736750597207),
 .UNSPECIFIED.);
#583=B_SPLINE_CURVE_WITH_KNOTS('',3,(#29507,#29508,#29509,#29510,#29511,
#29512,#29513,#29514,#29515,#29516,#29517,#29518,#29519,#29520,#29521,#29522,
#29523,#29524,#29525,#29526,#29527,#29528),.UNSPECIFIED.,.F.,.F.,(4,2,2,
2,2,2,2,2,2,2,4),(0.0789094028588958,0.210573405340968,0.315860108011452,
0.421146810681936,0.522142632548711,0.623138454415486,0.72413427628226,
0.825130098149035,0.930416800819519,1.03570350349,1.16736750597208),
 .UNSPECIFIED.);
#584=B_SPLINE_CURVE_WITH_KNOTS('',3,(#29537,#29538,#29539,#29540,#29541,
#29542,#29543,#29544,#29545,#29546,#29547,#29548,#29549,#29550,#29551,#29552,
#29553,#29554,#29555,#29556,#29557,#29558),.UNSPECIFIED.,.F.,.F.,(4,2,2,
2,2,2,2,2,2,2,4),(0.0789094028588958,0.210573405340968,0.315860108011452,
0.421146810681936,0.522142632548711,0.623138454415485,0.72413427628226,
0.825130098149035,0.930416800819519,1.03570350349,1.16736750597208),
 .UNSPECIFIED.);
#585=B_SPLINE_CURVE_WITH_KNOTS('',3,(#30811,#30812,#30813,#30814,#30815,
#30816,#30817,#30818,#30819,#30820,#30821,#30822,#30823,#30824,#30825,#30826,
#30827,#30828,#30829,#30830,#30831,#30832,#30833,#30834,#30835),
 .UNSPECIFIED.,.F.,.F.,(4,3,3,3,3,3,3,3,4),(-3.56038179279204,-3.46201024481372,
-2.96743735269747,-2.47286446058123,-1.97829156846498,-1.48371867634874,
-0.989145784232491,-0.494572892116246,0.),.UNSPECIFIED.);
#586=B_SPLINE_CURVE_WITH_KNOTS('',3,(#30838,#30839,#30840,#30841,#30842,
#30843,#30844,#30845,#30846,#30847,#30848,#30849,#30850,#30851,#30852,#30853,
#30854,#30855,#30856,#30857,#30858,#30859,#30860,#30861,#30862,#30863,#30864,
#30865,#30866,#30867,#30868,#30869,#30870,#30871,#30872,#30873,#30874,#30875,
#30876,#30877),.UNSPECIFIED.,.F.,.F.,(4,3,3,3,3,3,3,3,3,3,3,3,3,4),(0.937891254796418,
0.989145784232494,1.48371867634874,1.97829156846498,2.47286446058123,2.96743735269748,
3.46201024481372,3.95658313692997,4.45115602904621,4.94572892116246,5.44030181327871,
5.93487470539495,6.42944759751119,6.80228742277363),.UNSPECIFIED.);
#587=B_SPLINE_CURVE_WITH_KNOTS('',3,(#30882,#30883,#30884,#30885,#30886,
#30887,#30888,#30889,#30890,#30891,#30892,#30893,#30894,#30895,#30896,#30897,
#30898,#30899,#30900,#30901,#30902,#30903,#30904,#30905,#30906,#30907,#30908,
#30909,#30910,#30911,#30912,#30913,#30914,#30915,#30916,#30917,#30918,#30919,
#30920,#30921),.UNSPECIFIED.,.F.,.F.,(4,3,3,3,3,3,3,3,3,3,3,3,3,4),(-9.8435670999716,
-9.39688495020867,-8.90231205809242,-8.40773916597618,-7.91316627385993,
-7.41859338174369,-6.92402048962744,-6.42944759751119,-5.93487470539495,
-5.4403018132787,-4.94572892116246,-4.45115602904621,-3.95658313692996,
-3.56038179279204),.UNSPECIFIED.);
#588=B_SPLINE_CURVE_WITH_KNOTS('',3,(#30922,#30923,#30924,#30925,#30926,
#30927,#30928,#30929,#30930,#30931,#30932,#30933,#30934,#30935,#30936,#30937,
#30938,#30939,#30940,#30941,#30942,#30943,#30944,#30945,#30946,#30947,#30948,
#30949,#30950,#30951,#30952,#30953,#30954,#30955,#30956,#30957,#30958,#30959,
#30960,#30961,#30962,#30963,#30964),.UNSPECIFIED.,.F.,.F.,(4,3,3,3,3,3,
3,3,3,3,3,3,3,3,4),(6.80228742277363,6.92402048962744,7.41859338174369,
7.91316627385993,8.40773916597617,8.90231205809242,9.39688495020867,9.89145784232491,
10.3860307344412,10.8806036265574,11.3751765186736,11.8697494107899,12.3643223029061,
12.8588951950224,13.0854727299532),.UNSPECIFIED.);
#589=B_SPLINE_CURVE_WITH_KNOTS('',3,(#30969,#30970,#30971,#30972,#30973,
#30974,#30975,#30976,#30977,#30978,#30979,#30980,#30981,#30982,#30983,#30984,
#30985,#30986,#30987,#30988,#30989,#30990,#30991,#30992,#30993,#30994,#30995,
#30996,#30997,#30998,#30999,#31000,#31001,#31002,#31003,#31004,#31005,#31006,
#31007,#31008,#31009,#31010,#31011),.UNSPECIFIED.,.F.,.F.,(4,3,3,3,3,3,
3,3,3,3,3,3,3,3,4),(-16.1267524071512,-15.8263325477199,-15.3317596556036,
-14.8371867634874,-14.3426138713711,-13.8480409792549,-13.3534680871386,
-12.8588951950224,-12.3643223029061,-11.8697494107899,-11.3751765186736,
-10.8806036265574,-10.3860307344412,-9.89145784232491,-9.8435670999716),
 .UNSPECIFIED.);
#590=B_SPLINE_CURVE_WITH_KNOTS('',3,(#31012,#31013,#31014,#31015,#31016,
#31017,#31018,#31019,#31020,#31021,#31022,#31023,#31024,#31025,#31026,#31027,
#31028,#31029,#31030,#31031,#31032,#31033,#31034,#31035,#31036,#31037,#31038,
#31039,#31040,#31041,#31042,#31043,#31044,#31045,#31046,#31047,#31048,#31049,
#31050,#31051,#31052,#31053,#31054),.UNSPECIFIED.,.F.,.F.,(4,3,3,3,3,3,
3,3,3,3,3,3,3,3,4),(13.0854727299532,13.3534680871386,13.8480409792549,
14.3426138713711,14.8371867634874,15.3317596556036,15.8263325477199,16.3209054398361,
16.8154783319523,17.3100512240686,17.8046241161848,18.2991970083011,18.7937699004173,
19.2883427925336,19.3686580371328),.UNSPECIFIED.);
#591=B_SPLINE_CURVE_WITH_KNOTS('',3,(#31059,#31060,#31061,#31062,#31063,
#31064,#31065,#31066,#31067,#31068,#31069,#31070,#31071,#31072,#31073,#31074,
#31075,#31076,#31077,#31078,#31079,#31080,#31081,#31082,#31083,#31084,#31085,
#31086,#31087,#31088,#31089,#31090,#31091,#31092,#31093,#31094,#31095,#31096,
#31097,#31098,#31099,#31100,#31101),.UNSPECIFIED.,.F.,.F.,(4,3,3,3,3,3,
3,3,3,3,3,3,3,3,4),(-22.4099377143308,-22.2557801452311,-21.7612072531148,
-21.2666343609986,-20.7720614688823,-20.2774885767661,-19.7829156846498,
-19.2883427925336,-18.7937699004173,-18.2991970083011,-17.8046241161848,
-17.3100512240686,-16.8154783319523,-16.3209054398361,-16.1267524071512),
 .UNSPECIFIED.);
#592=B_SPLINE_CURVE_WITH_KNOTS('',3,(#31102,#31103,#31104,#31105,#31106,
#31107,#31108,#31109,#31110,#31111,#31112,#31113,#31114,#31115,#31116,#31117,
#31118,#31119,#31120,#31121,#31122,#31123,#31124,#31125,#31126,#31127,#31128,
#31129,#31130,#31131,#31132,#31133,#31134,#31135,#31136,#31137,#31138,#31139,
#31140,#31141),.UNSPECIFIED.,.F.,.F.,(4,3,3,3,3,3,3,3,3,3,3,3,3,4),(19.3686580371328,
19.7829156846498,20.2774885767661,20.7720614688823,21.2666343609986,21.7612072531148,
22.255780145231,22.7503530373473,23.2449259294635,23.7394988215798,24.234071713696,
24.7286446058123,25.2232174979285,25.6518433443124),.UNSPECIFIED.);
#593=B_SPLINE_CURVE_WITH_KNOTS('',3,(#31146,#31147,#31148,#31149,#31150,
#31151,#31152,#31153,#31154,#31155,#31156,#31157,#31158,#31159,#31160,#31161,
#31162,#31163,#31164,#31165,#31166,#31167,#31168,#31169,#31170,#31171,#31172,
#31173,#31174,#31175,#31176,#31177,#31178,#31179,#31180,#31181,#31182,#31183,
#31184,#31185,#31186,#31187,#31188),.UNSPECIFIED.,.F.,.F.,(4,3,3,3,3,3,
3,3,3,3,3,3,3,3,4),(-28.6931230215104,-28.6852277427422,-28.190654850626,
-27.6960819585097,-27.2015090663935,-26.7069361742773,-26.212363282161,
-25.7177903900448,-25.2232174979285,-24.7286446058123,-24.234071713696,
-23.7394988215798,-23.2449259294635,-22.7503530373473,-22.4099377143308),
 .UNSPECIFIED.);
#594=B_SPLINE_CURVE_WITH_KNOTS('',3,(#31189,#31190,#31191,#31192,#31193,
#31194,#31195,#31196,#31197,#31198,#31199,#31200,#31201,#31202,#31203,#31204,
#31205,#31206,#31207,#31208,#31209,#31210,#31211,#31212,#31213,#31214,#31215,
#31216,#31217,#31218,#31219,#31220,#31221,#31222,#31223,#31224,#31225,#31226,
#31227,#31228,#31229,#31230,#31231),.UNSPECIFIED.,.F.,.F.,(4,3,3,3,3,3,
3,3,3,3,3,3,3,3,4),(25.6518433443124,25.7177903900448,26.212363282161,26.7069361742773,
27.2015090663935,27.6960819585097,28.190654850626,28.6852277427422,29.1798006348585,
29.6743735269747,30.168946419091,30.6635193112072,31.1580922033235,31.6526650954397,
31.935028651492),.UNSPECIFIED.);
#595=B_SPLINE_CURVE_WITH_KNOTS('',3,(#31236,#31237,#31238,#31239,#31240,
#31241,#31242,#31243,#31244,#31245,#31246,#31247,#31248,#31249,#31250,#31251,
#31252,#31253,#31254,#31255,#31256,#31257,#31258,#31259,#31260,#31261,#31262,
#31263,#31264,#31265,#31266,#31267,#31268,#31269,#31270,#31271,#31272,#31273,
#31274,#31275),.UNSPECIFIED.,.F.,.F.,(4,3,3,3,3,3,3,3,3,3,3,3,3,4),(-34.97630832869,
-34.6201024481372,-34.1255295560209,-33.6309566639047,-33.1363837717884,
-32.6418108796722,-32.147237987556,-31.6526650954397,-31.1580922033235,
-30.6635193112072,-30.168946419091,-29.6743735269747,-29.1798006348585,
-28.6931230215104),.UNSPECIFIED.);
#596=B_SPLINE_CURVE_WITH_KNOTS('',3,(#31276,#31277,#31278,#31279,#31280,
#31281,#31282,#31283,#31284,#31285,#31286,#31287,#31288,#31289,#31290,#31291,
#31292,#31293,#31294,#31295,#31296,#31297,#31298,#31299,#31300,#31301,#31302,
#31303,#31304,#31305,#31306,#31307,#31308,#31309,#31310,#31311,#31312,#31313,
#31314,#31315,#31316,#31317,#31318),.UNSPECIFIED.,.F.,.F.,(4,3,3,3,3,3,
3,3,3,3,3,3,3,3,4),(31.935028651492,32.147237987556,32.6418108796722,33.1363837717885,
33.6309566639047,34.1255295560209,34.6201024481372,35.1146753402534,35.6092482323697,
36.1038211244859,36.5983940166022,37.0929669087184,37.5875398008347,38.0821126929509,
38.2182139586716),.UNSPECIFIED.);
#597=B_SPLINE_CURVE_WITH_KNOTS('',3,(#31323,#31324,#31325,#31326,#31327,
#31328,#31329,#31330,#31331,#31332,#31333,#31334,#31335,#31336,#31337,#31338,
#31339,#31340,#31341,#31342,#31343,#31344,#31345,#31346,#31347,#31348,#31349,
#31350,#31351,#31352,#31353,#31354,#31355,#31356,#31357,#31358,#31359,#31360,
#31361,#31362,#31363,#31364,#31365),.UNSPECIFIED.,.F.,.F.,(4,3,3,3,3,3,
3,3,3,3,3,3,3,3,4),(-41.2594936358696,-41.0495500456484,-40.5549771535321,
-40.0604042614159,-39.5658313692996,-39.0712584771834,-38.5766855850671,
-38.0821126929509,-37.5875398008347,-37.0929669087184,-36.5983940166022,
-36.1038211244859,-35.6092482323697,-35.1146753402534,-34.97630832869),
 .UNSPECIFIED.);
#598=B_SPLINE_CURVE_WITH_KNOTS('',3,(#31366,#31367,#31368,#31369,#31370,
#31371,#31372,#31373,#31374,#31375,#31376,#31377,#31378,#31379,#31380,#31381,
#31382,#31383,#31384,#31385,#31386,#31387,#31388,#31389,#31390,#31391,#31392,
#31393,#31394,#31395,#31396,#31397,#31398,#31399,#31400,#31401,#31402,#31403,
#31404,#31405),.UNSPECIFIED.,.F.,.F.,(4,3,3,3,3,3,3,3,3,3,3,3,3,4),(38.2182139586716,
38.5766855850671,39.0712584771834,39.5658313692996,40.0604042614159,40.5549771535321,
41.0495500456484,41.5441229377646,42.0386958298809,42.5332687219971,43.0278416141134,
43.5224145062296,44.0169873983459,44.5013992658512),.UNSPECIFIED.);
#599=B_SPLINE_CURVE_WITH_KNOTS('',3,(#31410,#31411,#31412,#31413,#31414,
#31415,#31416,#31417,#31418,#31419,#31420,#31421,#31422,#31423,#31424,#31425,
#31426,#31427,#31428,#31429,#31430,#31431,#31432,#31433,#31434,#31435,#31436,
#31437,#31438,#31439,#31440,#31441,#31442,#31443,#31444,#31445,#31446,#31447,
#31448,#31449,#31450,#31451,#31452),.UNSPECIFIED.,.F.,.F.,(4,3,3,3,3,3,
3,3,3,3,3,3,3,3,4),(-47.5426789430491,-47.4789976431596,-46.9844247510433,
-46.4898518589271,-45.9952789668108,-45.5007060746946,-45.0061331825783,
-44.5115602904621,-44.0169873983458,-43.5224145062296,-43.0278416141134,
-42.5332687219971,-42.0386958298809,-41.5441229377646,-41.2594936358696),
 .UNSPECIFIED.);
#600=B_SPLINE_CURVE_WITH_KNOTS('',3,(#31453,#31454,#31455,#31456,#31457,
#31458,#31459,#31460,#31461,#31462,#31463,#31464,#31465,#31466,#31467,#31468,
#31469,#31470,#31471,#31472,#31473,#31474,#31475,#31476,#31477,#31478,#31479,
#31480,#31481,#31482,#31483,#31484,#31485,#31486,#31487,#31488,#31489,#31490,
#31491,#31492,#31493,#31494,#31495),.UNSPECIFIED.,.F.,.F.,(4,3,3,3,3,3,
3,3,3,3,3,3,3,3,4),(44.5013992658512,44.5115602904621,45.0061331825783,
45.5007060746946,45.9952789668108,46.4898518589271,46.9844247510433,47.4789976431596,
47.9735705352758,48.4681434273921,48.9627163195083,49.4572892116245,49.9518621037408,
50.446434995857,50.7845845730308),.UNSPECIFIED.);
#601=B_SPLINE_CURVE_WITH_KNOTS('',3,(#31502,#31503,#31504,#31505,#31506,
#31507,#31508,#31509,#31510,#31511),.UNSPECIFIED.,.F.,.F.,(4,3,3,4),(-54.4542726622231,
-54.403018132787,-53.9084452406708,-53.8258642502287),.UNSPECIFIED.);
#602=B_SPLINE_CURVE_WITH_KNOTS('',3,(#31517,#31518,#31519,#31520,#31521,
#31522,#31523),.UNSPECIFIED.,.F.,.F.,(4,1,1,1,4),(65.9734457253856,66.0560267158277,
66.5505996079439,67.0451725000601,67.5397453921764),.UNSPECIFIED.);
#603=B_SPLINE_CURVE_WITH_KNOTS('',3,(#31526,#31527,#31528,#31529,#31530,
#31531,#31532,#31533,#31534,#31535,#31536,#31537),.UNSPECIFIED.,.F.,.F.,
(4,1,1,1,1,1,1,1,1,4),(65.9734457253856,66.1298690403281,66.6244419324444,
67.1190148245607,67.6135877166769,68.1081606087931,68.6027335009094,69.0973063930256,
69.5918792851419,69.643133814578),.UNSPECIFIED.);
#604=B_SPLINE_CURVE_WITH_KNOTS('',3,(#31542,#31543,#31544,#31545,#31546,
#31547,#31548,#31549,#31550,#31551,#31552,#31553,#31554,#31555,#31556,#31557),
 .UNSPECIFIED.,.F.,.F.,(4,1,1,1,1,1,1,1,1,1,1,1,1,4),(59.6902604182061,
60.1211520104327,60.615724902549,61.1102977946652,61.6048706867815,62.0994435788977,
62.5940164710139,63.0885893631302,63.5831622552464,64.0777351473627,64.5723080394789,
65.0668809315952,65.5614538237114,65.9734457253856),.UNSPECIFIED.);
#605=B_SPLINE_CURVE_WITH_KNOTS('',3,(#31558,#31559,#31560,#31561,#31562,
#31563,#31564,#31565,#31566,#31567,#31568,#31569,#31570,#31571,#31572,#31573,
#31574),.UNSPECIFIED.,.F.,.F.,(4,1,1,1,1,1,1,1,1,1,1,1,1,1,4),(59.6902604182061,
59.700421442817,60.1949943349332,60.6895672270495,61.1841401191657,61.6787130112819,
62.1732859033982,62.6678587955144,63.1624316876307,63.6570045797469,64.1515774718632,
64.6461503639794,65.1407232560957,65.6352961482119,65.9734457253856),
 .UNSPECIFIED.);
#606=B_SPLINE_CURVE_WITH_KNOTS('',3,(#31579,#31580,#31581,#31582,#31583,
#31584,#31585,#31586,#31587,#31588,#31589,#31590,#31591,#31592,#31593,#31594,
#31595),.UNSPECIFIED.,.F.,.F.,(4,1,1,1,1,1,1,1,1,1,1,1,1,1,4),(53.4070751110264,
53.6917044129215,54.1862773050378,54.680850197154,55.1754230892703,55.6699959813865,
56.1645688735028,56.659141765619,57.1537146577353,57.6482875498515,58.1428604419677,
58.637433334084,59.1320062262002,59.6265791183165,59.6902604182061),
 .UNSPECIFIED.);
#607=B_SPLINE_CURVE_WITH_KNOTS('',3,(#31596,#31597,#31598,#31599,#31600,
#31601,#31602,#31603,#31604,#31605,#31606,#31607,#31608,#31609,#31610,#31611),
 .UNSPECIFIED.,.F.,.F.,(4,1,1,1,1,1,1,1,1,1,1,1,1,4),(53.4070751110264,
53.765546737422,54.2601196295383,54.7546925216545,55.2492654137708,55.743838305887,
56.2384111980032,56.7329840901195,57.2275569822357,57.722129874352,58.2167027664682,
58.7112756585845,59.2058485507007,59.6902604182061),.UNSPECIFIED.);
#608=B_SPLINE_CURVE_WITH_KNOTS('',3,(#31616,#31617,#31618,#31619,#31620,
#31621,#31622,#31623,#31624,#31625,#31626,#31627,#31628,#31629,#31630,#31631,
#31632),.UNSPECIFIED.,.F.,.F.,(4,1,1,1,1,1,1,1,1,1,1,1,1,1,4),(47.1238898038469,
47.2622568154103,47.7568297075266,48.2514025996428,48.7459754917591,49.2405483838753,
49.7351212759916,50.2296941681078,50.7242670602241,51.2188399523403,51.7134128444565,
52.2079857365728,52.702558628689,53.1971315208053,53.4070751110264),
 .UNSPECIFIED.);
#609=B_SPLINE_CURVE_WITH_KNOTS('',3,(#31633,#31634,#31635,#31636,#31637,
#31638,#31639,#31640,#31641,#31642,#31643,#31644,#31645,#31646,#31647,#31648,
#31649),.UNSPECIFIED.,.F.,.F.,(4,1,1,1,1,1,1,1,1,1,1,1,1,1,4),(47.1238898038469,
47.3360991399108,47.8306720320271,48.3252449241433,48.8198178162596,49.3143907083758,
49.8089636004921,50.3035364926083,50.7981093847245,51.2926822768408,51.787255168957,
52.2818280610733,52.7764009531895,53.2709738453058,53.4070751110264),
 .UNSPECIFIED.);
#610=B_SPLINE_CURVE_WITH_KNOTS('',3,(#31654,#31655,#31656,#31657,#31658,
#31659,#31660,#31661,#31662,#31663,#31664,#31665,#31666,#31667,#31668,#31669),
 .UNSPECIFIED.,.F.,.F.,(4,1,1,1,1,1,1,1,1,1,1,1,1,4),(40.8407044966673,
41.3273821100154,41.8219550021316,42.3165278942479,42.8111007863641,43.3056736784804,
43.8002465705966,44.2948194627129,44.7893923548291,45.2839652469454,45.7785381390616,
46.2731110311778,46.7676839232941,47.1238898038469),.UNSPECIFIED.);
#611=B_SPLINE_CURVE_WITH_KNOTS('',3,(#31670,#31671,#31672,#31673,#31674,
#31675,#31676,#31677,#31678,#31679,#31680,#31681,#31682,#31683,#31684,#31685,
#31686),.UNSPECIFIED.,.F.,.F.,(4,1,1,1,1,1,1,1,1,1,1,1,1,1,4),(40.8407044966673,
40.9066515423996,41.4012244345159,41.8957973266321,42.3903702187484,42.8849431108646,
43.3795160029809,43.8740888950971,44.3686617872134,44.8632346793296,45.3578075714458,
45.8523804635621,46.3469533556783,46.8415262477946,47.1238898038469),
 .UNSPECIFIED.);
#612=B_SPLINE_CURVE_WITH_KNOTS('',3,(#31691,#31692,#31693,#31694,#31695,
#31696,#31697,#31698,#31699,#31700,#31701,#31702,#31703,#31704,#31705,#31706,
#31707),.UNSPECIFIED.,.F.,.F.,(4,1,1,1,1,1,1,1,1,1,1,1,1,1,4),(34.5575191894877,
34.8979345125042,35.3925074046204,35.8870802967367,36.3816531888529,36.8762260809692,
37.3707989730854,37.8653718652017,38.3599447573179,38.8545176494342,39.3490905415504,
39.8436634336667,40.3382363257829,40.8328092178991,40.8407044966673),
 .UNSPECIFIED.);
#613=B_SPLINE_CURVE_WITH_KNOTS('',3,(#31708,#31709,#31710,#31711,#31712,
#31713,#31714,#31715,#31716,#31717,#31718,#31719,#31720,#31721,#31722,#31723),
 .UNSPECIFIED.,.F.,.F.,(4,1,1,1,1,1,1,1,1,1,1,1,1,4),(34.5575191894877,
34.9717768370047,35.4663497291209,35.9609226212372,36.4554955133534,36.9500684054697,
37.4446412975859,37.9392141897022,38.4337870818184,38.9283599739347,39.4229328660509,
39.9175057581671,40.4120786502834,40.8407044966673),.UNSPECIFIED.);
#614=B_SPLINE_CURVE_WITH_KNOTS('',3,(#31728,#31729,#31730,#31731,#31732,
#31733,#31734,#31735,#31736,#31737,#31738,#31739,#31740,#31741,#31742,#31743,
#31744),.UNSPECIFIED.,.F.,.F.,(4,1,1,1,1,1,1,1,1,1,1,1,1,1,4),(28.2743338823081,
28.468486914993,28.9630598071093,29.4576326992255,29.9522055913417,30.446778483458,
30.9413513755742,31.4359242676905,31.9304971598067,32.425070051923,32.9196429440392,
33.4142158361555,33.9087887282717,34.403361620388,34.5575191894877),
 .UNSPECIFIED.);
#615=B_SPLINE_CURVE_WITH_KNOTS('',3,(#31745,#31746,#31747,#31748,#31749,
#31750,#31751,#31752,#31753,#31754,#31755,#31756,#31757,#31758,#31759,#31760,
#31761),.UNSPECIFIED.,.F.,.F.,(4,1,1,1,1,1,1,1,1,1,1,1,1,1,4),(28.2743338823081,
28.5423292394935,29.0369021316097,29.531475023726,30.0260479158422,30.5206208079585,
31.0151937000747,31.509766592191,32.0043394843072,32.4989123764235,32.9934852685397,
33.488058160656,33.9826310527722,34.4772039448884,34.5575191894877),
 .UNSPECIFIED.);
#616=B_SPLINE_CURVE_WITH_KNOTS('',3,(#31766,#31767,#31768,#31769,#31770,
#31771,#31772,#31773,#31774,#31775,#31776,#31777,#31778,#31779,#31780,#31781,
#31782),.UNSPECIFIED.,.F.,.F.,(4,1,1,1,1,1,1,1,1,1,1,1,1,1,4),(21.9911485751285,
22.0390393174818,22.5336122095981,23.0281851017143,23.5227579938306,24.0173308859468,
24.511903778063,25.0064766701793,25.5010495622955,25.9956224544118,26.490195346528,
26.9847682386443,27.4793411307605,27.9739140228768,28.2743338823081),
 .UNSPECIFIED.);
#617=B_SPLINE_CURVE_WITH_KNOTS('',3,(#31783,#31784,#31785,#31786,#31787,
#31788,#31789,#31790,#31791,#31792,#31793,#31794,#31795,#31796,#31797,#31798,
#31799),.UNSPECIFIED.,.F.,.F.,(4,1,1,1,1,1,1,1,1,1,1,1,1,1,4),(21.9911485751285,
22.1128816419823,22.6074545340986,23.1020274262148,23.596600318331,24.0911732104473,
24.5857461025635,25.0803189946798,25.574891886796,26.0694647789123,26.5640376710285,
27.0586105631448,27.553183455261,28.0477563473773,28.2743338823081),
 .UNSPECIFIED.);
#618=B_SPLINE_CURVE_WITH_KNOTS('',3,(#31805,#31806,#31807,#31808,#31809),
 .UNSPECIFIED.,.F.,.F.,(4,1,4),(15.1888611523549,15.6834340444711,15.7079632679489),
 .UNSPECIFIED.);
#619=B_SPLINE_CURVE_WITH_KNOTS('',3,(#31812,#31813,#31814,#31815,#31816,
#31817,#31818,#31819,#31820,#31821),.UNSPECIFIED.,.F.,.F.,(4,1,1,1,1,1,
1,4),(13.0854727299533,13.1367272593894,13.6313001515056,14.1258730436219,
14.6204459357381,15.1150188278544,15.6095917199706,15.7079632679489),
 .UNSPECIFIED.);
#620=B_SPLINE_CURVE_WITH_KNOTS('',3,(#31823,#31824,#31825,#31826,#31827,
#31828,#31829,#31830,#31831,#31832,#31833,#31834,#31835,#31836,#31837,#31838),
 .UNSPECIFIED.,.F.,.F.,(4,1,1,1,1,1,1,1,1,1,1,1,1,4),(15.7079632679489,
16.1041646120869,16.5987375042031,17.0933103963194,17.5878832884356,18.0824561805519,
18.5770290726681,19.0716019647843,19.5661748569006,20.0607477490168,20.5553206411331,
21.0498935332493,21.5444664253656,21.9911485751285),.UNSPECIFIED.);
#621=B_SPLINE_CURVE_WITH_KNOTS('',3,(#31839,#31840,#31841,#31842,#31843,
#31844,#31845,#31846,#31847,#31848,#31849,#31850,#31851,#31852,#31853,#31854),
 .UNSPECIFIED.,.F.,.F.,(4,1,1,1,1,1,1,1,1,1,1,1,1,4),(15.7079632679489,
16.1780069365874,16.6725798287036,17.1671527208199,17.6617256129361,18.1562985050523,
18.6508713971686,19.1454442892848,19.6400171814011,20.1345900735173,20.6291629656336,
21.1237358577498,21.6183087498661,21.9911485751285),.UNSPECIFIED.);
#622=B_SPLINE_CURVE_WITH_KNOTS('',3,(#32315,#32316,#32317,#32318,#32319,
#32320,#32321,#32322,#32323,#32324,#32325,#32326,#32327,#32328,#32329,#32330,
#32331,#32332,#32333,#32334,#32335,#32336,#32337,#32338,#32339,#32340,#32341,
#32342,#32343,#32344,#32345),.UNSPECIFIED.,.F.,.F.,(4,3,3,3,3,3,3,3,3,3,
4),(0.,0.0822466706468383,0.162608105240606,0.216579893838171,0.23924274204394,
0.301838371937517,0.36076250940623,0.388067588559334,0.409537377502954,
0.476290104322315,0.53753492181237),.UNSPECIFIED.);
#623=B_SPLINE_CURVE_WITH_KNOTS('',3,(#32346,#32347,#32348,#32349,#32350,
#32351,#32352,#32353,#32354,#32355,#32356,#32357,#32358,#32359,#32360,#32361,
#32362,#32363,#32364,#32365,#32366,#32367,#32368,#32369,#32370,#32371,#32372,
#32373),.UNSPECIFIED.,.F.,.F.,(4,3,3,3,3,3,3,3,3,4),(0.,0.0665230127441691,
0.13429495842692,0.176258819244205,0.195926107024299,0.263526952009386,
0.33682854572103,0.365338415901403,0.449700157257057,0.534061898612711),
 .UNSPECIFIED.);
#624=B_SPLINE_CURVE_WITH_KNOTS('',3,(#32374,#32375,#32376,#32377,#32378,
#32379,#32380,#32381,#32382,#32383,#32384,#32385,#32386,#32387,#32388,#32389,
#32390,#32391,#32392,#32393,#32394,#32395,#32396,#32397,#32398,#32399,#32400,
#32401,#32402,#32403,#32404,#32405,#32406,#32407,#32408,#32409,#32410,#32411,
#32412,#32413),.UNSPECIFIED.,.F.,.F.,(4,3,3,3,3,3,3,3,3,3,3,3,3,4),(-53.8258642502287,
-53.4138723485545,-52.9192994564383,-52.424726564322,-51.9301536722058,
-51.4355807800895,-50.9410078879733,-50.446434995857,-49.9518621037408,
-49.4572892116245,-48.9627163195083,-48.4681434273921,-47.9735705352758,
-47.5426789430491),.UNSPECIFIED.);
#625=B_SPLINE_CURVE_WITH_KNOTS('',3,(#32875,#32876,#32877,#32878,#32879,
#32880,#32881,#32882,#32883,#32884,#32885,#32886,#32887,#32888,#32889,#32890,
#32891,#32892,#32893,#32894,#32895,#32896,#32897,#32898,#32899,#32900,#32901,
#32902),.UNSPECIFIED.,.F.,.F.,(4,3,3,3,3,3,3,3,3,4),(0.,0.0665230199567328,
0.134294967830964,0.176258831509978,0.195926124443112,0.263526952009376,
0.336828549458816,0.365338416771381,0.449700157692121,0.534061898612861),
 .UNSPECIFIED.);
#626=B_SPLINE_CURVE_WITH_KNOTS('',3,(#32903,#32904,#32905,#32906,#32907,
#32908,#32909,#32910,#32911,#32912,#32913,#32914,#32915,#32916,#32917,#32918,
#32919,#32920,#32921,#32922,#32923,#32924,#32925,#32926,#32927,#32928,#32929,
#32930,#32931,#32932,#32933),.UNSPECIFIED.,.F.,.F.,(4,3,3,3,3,3,3,3,3,3,
4),(50.7845845730308,50.9410078879733,51.4355807800895,51.9301536722058,
52.424726564322,52.9192994564383,53.4138723485545,53.9084452406708,54.403018132787,
54.8975910249033,55.3921639170195),.UNSPECIFIED.);
#627=B_SPLINE_CURVE_WITH_KNOTS('',3,(#32934,#32935,#32936,#32937,#32938,
#32939,#32940,#32941,#32942,#32943,#32944,#32945,#32946,#32947,#32948,#32949,
#32950,#32951,#32952,#32953,#32954,#32955,#32956,#32957,#32958,#32959,#32960,
#32961,#32962,#32963,#32964),.UNSPECIFIED.,.F.,.F.,(4,3,3,3,3,3,3,3,3,3,
4),(0.,0.0822466663612967,0.162608100396307,0.216579890867136,0.239242742625966,
0.301838371937549,0.360762509406336,0.388067584071394,0.409537375230468,
0.476290092032249,0.537534921812695),.UNSPECIFIED.);
#628=B_SPLINE_CURVE_WITH_KNOTS('',3,(#33264,#33265,#33266,#33267,#33268,
#33269,#33270,#33271,#33272,#33273,#33274,#33275,#33276,#33277,#33278,#33279,
#33280,#33281,#33282),.UNSPECIFIED.,.F.,.F.,(4,3,3,3,3,3,4),(-3.69871549170445,
-3.49775346748116,-2.99807440069814,-2.49839533391511,-1.99871626713209,
-1.49903720034907,-1.00018350866767),.UNSPECIFIED.);
#629=B_SPLINE_CURVE_WITH_KNOTS('',3,(#33285,#33286,#33287,#33288),
 .UNSPECIFIED.,.F.,.F.,(4,4),(0.,0.443060670554495),.UNSPECIFIED.);
#630=B_SPLINE_CURVE_WITH_KNOTS('',3,(#33293,#33294,#33295,#33296,#33297,
#33298,#33299,#33300,#33301,#33302,#33303,#33304,#33305,#33306,#33307,#33308,
#33309,#33310,#33311,#33312,#33313,#33314,#33315,#33316,#33317,#33318,#33319,
#33320,#33321,#33322,#33323,#33324,#33325,#33326,#33327,#33328,#33329,#33330,
#33331,#33332),.UNSPECIFIED.,.F.,.F.,(4,3,3,3,3,3,3,3,3,3,3,3,3,4),(-9.98190079888403,
-9.49390226887744,-8.99422320209442,-8.4945441353114,-7.99486506852837,
-7.49518600174535,-6.99550693496233,-6.4958278681793,-5.99614880139628,
-5.49646973461325,-4.99679066783023,-4.49711160104721,-3.99743253426419,
-3.69871549170445),.UNSPECIFIED.);
#631=B_SPLINE_CURVE_WITH_KNOTS('',3,(#33333,#33334,#33335,#33336,#33337,
#33338,#33339,#33340,#33341,#33342,#33343,#33344,#33345,#33346,#33347,#33348,
#33349,#33350,#33351,#33352,#33353,#33354,#33355,#33356,#33357,#33358,#33359,
#33360,#33361,#33362,#33363,#33364,#33365,#33366,#33367,#33368,#33369,#33370,
#33371,#33372,#33373,#33374,#33375),.UNSPECIFIED.,.F.,.F.,(4,3,3,3,3,3,
3,3,3,3,3,3,3,3,4),(0.443060670554495,0.49967906678306,0.999358133566079,
1.4990372003491,1.99871626713212,2.49839533391514,2.99807440069816,3.49775346748117,
3.99743253426419,4.49711160104721,4.99679066783023,5.49646973461325,5.99614880139627,
6.49582786817929,6.72624597773408),.UNSPECIFIED.);
#632=B_SPLINE_CURVE_WITH_KNOTS('',3,(#33380,#33381,#33382,#33383,#33384,
#33385,#33386,#33387,#33388,#33389,#33390,#33391,#33392,#33393,#33394,#33395,
#33396,#33397,#33398,#33399,#33400,#33401,#33402,#33403,#33404,#33405,#33406,
#33407,#33408,#33409,#33410,#33411,#33412,#33413,#33414,#33415,#33416,#33417,
#33418,#33419,#33420,#33421,#33422),.UNSPECIFIED.,.F.,.F.,(4,3,3,3,3,3,
3,3,3,3,3,3,3,3,4),(-16.2650861060636,-15.9897301370567,-15.4900510702737,
-14.9903720034907,-14.4906929367077,-13.9910138699247,-13.4913348031416,
-12.9916557363586,-12.4919766695756,-11.9922976027926,-11.4926185360095,
-10.9929394692265,-10.4932604024435,-9.99358133566046,-9.98190079888403),
 .UNSPECIFIED.);
#633=B_SPLINE_CURVE_WITH_KNOTS('',3,(#33423,#33424,#33425,#33426,#33427,
#33428,#33429,#33430,#33431,#33432,#33433,#33434,#33435,#33436,#33437,#33438,
#33439,#33440,#33441,#33442,#33443,#33444,#33445,#33446,#33447,#33448,#33449,
#33450,#33451,#33452,#33453,#33454,#33455,#33456,#33457,#33458,#33459,#33460,
#33461,#33462,#33463,#33464,#33465),.UNSPECIFIED.,.F.,.F.,(4,3,3,3,3,3,
3,3,3,3,3,3,3,3,4),(6.72624597773408,6.99550693496231,7.49518600174534,
7.99486506852837,8.49454413531139,8.99422320209442,9.49390226887745,9.99358133566048,
10.4932604024435,10.9929394692265,11.4926185360096,11.9922976027926,12.4919766695756,
12.9916557363586,13.0094312849137),.UNSPECIFIED.);
#634=B_SPLINE_CURVE_WITH_KNOTS('',3,(#33470,#33471,#33472,#33473,#33474,
#33475,#33476,#33477,#33478,#33479,#33480,#33481,#33482,#33483,#33484,#33485,
#33486,#33487,#33488,#33489,#33490,#33491,#33492,#33493,#33494,#33495,#33496,
#33497,#33498,#33499,#33500,#33501,#33502,#33503,#33504,#33505,#33506,#33507,
#33508,#33509,#33510,#33511,#33512),.UNSPECIFIED.,.F.,.F.,(4,3,3,3,3,3,
3,3,3,3,3,3,3,3,4),(-22.5482714132432,-22.485558005236,-21.985878938453,
-21.48619987167,-20.986520804887,-20.486841738104,-19.9871626713209,-19.4874836045379,
-18.9878045377549,-18.4881254709719,-17.9884464041888,-17.4887673374058,
-16.9890882706228,-16.4894092038398,-16.2650861060636),.UNSPECIFIED.);
#635=B_SPLINE_CURVE_WITH_KNOTS('',3,(#33513,#33514,#33515,#33516,#33517,
#33518,#33519,#33520,#33521,#33522,#33523,#33524,#33525,#33526,#33527,#33528,
#33529,#33530,#33531,#33532,#33533,#33534,#33535,#33536,#33537,#33538,#33539,
#33540,#33541,#33542,#33543,#33544,#33545,#33546,#33547,#33548,#33549,#33550,
#33551,#33552),.UNSPECIFIED.,.F.,.F.,(4,3,3,3,3,3,3,3,3,3,3,3,3,4),(13.0094312849137,
13.4913348031417,13.9910138699247,14.4906929367077,14.9903720034907,15.4900510702737,
15.9897301370568,16.4894092038398,16.9890882706228,17.4887673374058,17.9884464041888,
18.4881254709718,18.9878045377549,19.2926165920933),.UNSPECIFIED.);
#636=B_SPLINE_CURVE_WITH_KNOTS('',3,(#33557,#33558,#33559,#33560,#33561,
#33562,#33563,#33564,#33565,#33566,#33567,#33568,#33569,#33570,#33571,#33572,
#33573,#33574,#33575,#33576,#33577,#33578,#33579,#33580,#33581,#33582,#33583,
#33584,#33585,#33586,#33587,#33588,#33589,#33590,#33591,#33592,#33593,#33594,
#33595,#33596),.UNSPECIFIED.,.F.,.F.,(4,3,3,3,3,3,3,3,3,3,3,3,3,4),(-28.8314567204228,
-28.4817068066323,-27.9820277398493,-27.4823486730663,-26.9826696062833,
-26.4829905395002,-25.9833114727172,-25.4836324059342,-24.9839533391512,
-24.4842742723681,-23.9845952055851,-23.4849161388021,-22.9852370720191,
-22.5482714132432),.UNSPECIFIED.);
#637=B_SPLINE_CURVE_WITH_KNOTS('',3,(#33597,#33598,#33599,#33600,#33601,
#33602,#33603,#33604,#33605,#33606,#33607,#33608,#33609,#33610,#33611,#33612,
#33613,#33614,#33615,#33616,#33617,#33618,#33619,#33620,#33621,#33622,#33623,
#33624,#33625,#33626,#33627,#33628,#33629,#33630,#33631,#33632,#33633,#33634,
#33635,#33636,#33637,#33638,#33639),.UNSPECIFIED.,.F.,.F.,(4,3,3,3,3,3,
3,3,3,3,3,3,3,3,4),(19.2926165920933,19.4874836045379,19.9871626713209,
20.4868417381039,20.986520804887,21.48619987167,21.985878938453,22.4855580052361,
22.9852370720191,23.4849161388021,23.9845952055851,24.4842742723682,24.9839533391512,
25.4836324059342,25.5758018992728),.UNSPECIFIED.);
#638=B_SPLINE_CURVE_WITH_KNOTS('',3,(#33644,#33645,#33646,#33647,#33648,
#33649,#33650,#33651,#33652,#33653,#33654,#33655,#33656,#33657,#33658,#33659,
#33660,#33661,#33662,#33663,#33664,#33665,#33666,#33667,#33668,#33669,#33670,
#33671,#33672,#33673,#33674,#33675,#33676,#33677,#33678,#33679,#33680,#33681,
#33682,#33683,#33684,#33685,#33686),.UNSPECIFIED.,.F.,.F.,(4,3,3,3,3,3,
3,3,3,3,3,3,3,3,4),(-35.1146420276024,-34.9775346748116,-34.4778556080286,
-33.9781765412456,-33.4784974744626,-32.9788184076795,-32.4791393408965,
-31.9794602741135,-31.4797812073305,-30.9801021405474,-30.4804230737644,
-29.9807440069814,-29.4810649401984,-28.9813858734153,-28.8314567204228),
 .UNSPECIFIED.);
#639=B_SPLINE_CURVE_WITH_KNOTS('',3,(#33687,#33688,#33689,#33690,#33691,
#33692,#33693,#33694,#33695,#33696,#33697,#33698,#33699,#33700,#33701,#33702,
#33703,#33704,#33705,#33706,#33707,#33708,#33709,#33710,#33711,#33712,#33713,
#33714,#33715,#33716,#33717,#33718,#33719,#33720,#33721,#33722,#33723,#33724,
#33725,#33726),.UNSPECIFIED.,.F.,.F.,(4,3,3,3,3,3,3,3,3,3,3,3,3,4),(25.5758018992728,
25.9833114727172,26.4829905395003,26.9826696062833,27.4823486730663,27.9820277398493,
28.4817068066324,28.9813858734154,29.4810649401984,29.9807440069814,30.4804230737645,
30.9801021405475,31.4797812073305,31.8589872064524),.UNSPECIFIED.);
#640=B_SPLINE_CURVE_WITH_KNOTS('',3,(#33731,#33732,#33733,#33734,#33735,
#33736,#33737,#33738,#33739,#33740,#33741,#33742,#33743,#33744,#33745,#33746,
#33747,#33748,#33749,#33750,#33751,#33752,#33753,#33754,#33755,#33756,#33757,
#33758,#33759,#33760,#33761,#33762,#33763,#33764,#33765,#33766,#33767,#33768,
#33769,#33770),.UNSPECIFIED.,.F.,.F.,(4,3,3,3,3,3,3,3,3,3,3,3,3,4),(-41.397827334782,
-40.9736834762079,-40.4740044094249,-39.9743253426419,-39.4746462758588,
-38.9749672090758,-38.4752881422928,-37.9756090755098,-37.4759300087267,
-36.9762509419437,-36.4765718751607,-35.9768928083777,-35.4772137415947,
-35.1146420276024),.UNSPECIFIED.);
#641=B_SPLINE_CURVE_WITH_KNOTS('',3,(#33771,#33772,#33773,#33774,#33775,
#33776,#33777,#33778,#33779,#33780,#33781,#33782,#33783,#33784,#33785,#33786,
#33787,#33788,#33789,#33790,#33791,#33792,#33793,#33794,#33795,#33796,#33797,
#33798,#33799,#33800,#33801,#33802,#33803,#33804,#33805,#33806,#33807,#33808,
#33809,#33810,#33811,#33812,#33813),.UNSPECIFIED.,.F.,.F.,(4,3,3,3,3,3,
3,3,3,3,3,3,3,3,4),(31.8589872064524,31.9794602741135,32.4791393408966,
32.9788184076796,33.4784974744626,33.9781765412456,34.4778556080286,34.9775346748117,
35.4772137415947,35.9768928083777,36.4765718751607,36.9762509419437,37.4759300087267,
37.9756090755098,38.142172513632),.UNSPECIFIED.);
#642=B_SPLINE_CURVE_WITH_KNOTS('',3,(#33818,#33819,#33820,#33821,#33822,
#33823,#33824,#33825,#33826,#33827,#33828,#33829,#33830,#33831,#33832,#33833,
#33834,#33835,#33836,#33837,#33838,#33839,#33840,#33841,#33842,#33843,#33844,
#33845,#33846,#33847,#33848,#33849,#33850,#33851,#33852,#33853,#33854,#33855,
#33856,#33857,#33858,#33859,#33860),.UNSPECIFIED.,.F.,.F.,(4,3,3,3,3,3,
3,3,3,3,3,3,3,3,4),(-47.6810126419616,-47.4695113443872,-46.9698322776042,
-46.4701532108212,-45.9704741440381,-45.4707950772551,-44.9711160104721,
-44.4714369436891,-43.971757876906,-43.472078810123,-42.97239974334,-42.472720676557,
-41.973041609774,-41.4733625429909,-41.397827334782),.UNSPECIFIED.);
#643=B_SPLINE_CURVE_WITH_KNOTS('',3,(#33861,#33862,#33863,#33864,#33865,
#33866,#33867,#33868,#33869,#33870,#33871,#33872,#33873,#33874,#33875,#33876,
#33877,#33878,#33879,#33880,#33881,#33882,#33883,#33884,#33885,#33886,#33887,
#33888,#33889,#33890,#33891,#33892,#33893,#33894,#33895,#33896,#33897,#33898,
#33899,#33900),.UNSPECIFIED.,.F.,.F.,(4,3,3,3,3,3,3,3,3,3,3,3,3,4),(38.142172513632,
38.4752881422928,38.9749672090758,39.4746462758589,39.9743253426419,40.4740044094249,
40.973683476208,41.473362542991,41.973041609774,42.472720676557,42.9723997433401,
43.4720788101231,43.9717578769061,44.4253578208116),.UNSPECIFIED.);
#644=B_SPLINE_CURVE_WITH_KNOTS('',3,(#33905,#33906,#33907,#33908,#33909,
#33910,#33911,#33912,#33913,#33914,#33915,#33916,#33917,#33918,#33919,#33920,
#33921,#33922,#33923,#33924,#33925,#33926,#33927,#33928,#33929,#33930,#33931,
#33932),.UNSPECIFIED.,.F.,.F.,(4,3,3,3,3,3,3,3,3,4),(-53.9641979491412,
-52.9659810790005,-51.9666229454344,-50.9672648118684,-49.9679066783023,
-49.4682276115193,-48.9685485447363,-48.4688694779533,-47.9691904111702,
-47.6810126419616),.UNSPECIFIED.);
#645=B_SPLINE_CURVE_WITH_KNOTS('',3,(#33933,#33934,#33935,#33936,#33937,
#33938,#33939,#33940,#33941,#33942,#33943,#33944,#33945,#33946,#33947,#33948,
#33949,#33950,#33951,#33952,#33953,#33954,#33955,#33956,#33957,#33958,#33959,
#33960,#33961,#33962,#33963,#33964,#33965,#33966,#33967,#33968,#33969,#33970,
#33971,#33972),.UNSPECIFIED.,.F.,.F.,(4,3,3,3,3,3,3,3,3,3,3,3,3,4),(44.4253578208116,
44.4714369436892,44.9711160104722,45.4707950772552,45.9704741440382,46.4701532108212,
46.9698322776042,47.4695113443873,47.9691904111703,48.4688694779533,48.9685485447363,
49.4682276115193,49.9679066783024,50.7085431279912),.UNSPECIFIED.);
#646=B_SPLINE_CURVE_WITH_KNOTS('',3,(#33977,#33978,#33979,#33980,#33981,
#33982,#33983,#33984,#33985,#33986,#33987,#33988,#33989,#33990,#33991,#33992,
#33993,#33994,#33995,#33996,#33997,#33998),.UNSPECIFIED.,.F.,.F.,(4,3,3,
3,3,3,3,4),(-60.2473832563207,-59.9614880139628,-58.9621298803968,-57.9627717468307,
-56.9634136132647,-55.9640554796986,-54.9646973461326,-53.9641979491412),
 .UNSPECIFIED.);
#647=B_SPLINE_CURVE_WITH_KNOTS('',3,(#33999,#34000,#34001,#34002,#34003,
#34004,#34005,#34006,#34007,#34008,#34009,#34010,#34011,#34012,#34013,#34014,
#34015,#34016,#34017,#34018,#34019,#34020,#34021,#34022,#34023),
 .UNSPECIFIED.,.F.,.F.,(4,3,3,3,3,3,3,3,4),(50.7085431279912,50.9672648118684,
51.9666229454345,52.9659810790005,53.9653392125666,54.9646973461326,55.9640554796987,
56.9634136132647,56.9917284351708),.UNSPECIFIED.);
#648=B_SPLINE_CURVE_WITH_KNOTS('',3,(#34028,#34029,#34030,#34031,#34032,
#34033,#34034,#34035,#34036,#34037,#34038,#34039,#34040,#34041,#34042,#34043,
#34044,#34045,#34046,#34047,#34048,#34049),.UNSPECIFIED.,.F.,.F.,(4,3,3,
3,3,3,3,4),(-66.5305685635003,-65.9576368153591,-64.958278681793,-63.958920548227,
-62.9595624146609,-61.9602042810949,-60.9608461475288,-60.2473832563207),
 .UNSPECIFIED.);
#649=B_SPLINE_CURVE_WITH_KNOTS('',3,(#34050,#34051,#34052,#34053,#34054,
#34055,#34056,#34057,#34058,#34059,#34060,#34061,#34062,#34063,#34064,#34065,
#34066,#34067,#34068,#34069,#34070,#34071),.UNSPECIFIED.,.F.,.F.,(4,3,3,
3,3,3,3,4),(56.9917284351708,57.9627717468308,58.9621298803968,59.9614880139629,
60.9608461475289,61.960204281095,62.959562414661,63.2749137423504),
 .UNSPECIFIED.);
#650=B_SPLINE_CURVE_WITH_KNOTS('',3,(#34076,#34077,#34078,#34079,#34080,
#34081,#34082,#34083,#34084,#34085,#34086,#34087,#34088,#34089,#34090,#34091,
#34092,#34093,#34094,#34095,#34096,#34097),.UNSPECIFIED.,.F.,.F.,(4,3,3,
3,3,3,3,4),(-72.8137538706799,-71.9537856167554,-70.9544274831893,-69.9550693496233,
-68.9557112160572,-67.9563530824912,-66.9569949489251,-66.5305685635003),
 .UNSPECIFIED.);
#651=B_SPLINE_CURVE_WITH_KNOTS('',3,(#34098,#34099,#34100,#34101,#34102,
#34103,#34104,#34105,#34106,#34107,#34108,#34109,#34110,#34111,#34112,#34113,
#34114,#34115,#34116,#34117,#34118,#34119),.UNSPECIFIED.,.F.,.F.,(4,3,3,
3,3,3,3,4),(63.2749137423504,63.958920548227,64.9582786817931,65.9576368153591,
66.9569949489252,67.9563530824912,68.9557112160573,69.55809904953),
 .UNSPECIFIED.);
#652=B_SPLINE_CURVE_WITH_KNOTS('',3,(#34124,#34125,#34126,#34127,#34128,
#34129,#34130,#34131,#34132,#34133,#34134,#34135,#34136,#34137,#34138,#34139,
#34140,#34141,#34142,#34143,#34144,#34145,#34146,#34147,#34148),
 .UNSPECIFIED.,.F.,.F.,(4,3,3,3,3,3,3,3,4),(-79.0969391778595,-78.9492925517177,
-77.9499344181516,-76.9505762845856,-75.9512181510195,-74.9518600174535,
-73.9525018838875,-72.9531437503214,-72.8137538706799),.UNSPECIFIED.);
#653=B_SPLINE_CURVE_WITH_KNOTS('',3,(#34149,#34150,#34151,#34152,#34153,
#34154,#34155,#34156,#34157,#34158,#34159,#34160,#34161,#34162,#34163,#34164,
#34165,#34166,#34167,#34168,#34169,#34170),.UNSPECIFIED.,.F.,.F.,(4,3,3,
3,3,3,3,4),(69.55809904953,69.9550693496233,70.9544274831893,71.9537856167554,
72.9531437503215,73.9525018838875,74.9518600174536,75.8412843567096),
 .UNSPECIFIED.);
#654=B_SPLINE_CURVE_WITH_KNOTS('',3,(#34175,#34176,#34177,#34178,#34179,
#34180,#34181,#34182,#34183,#34184,#34185,#34186,#34187,#34188,#34189,#34190,
#34191,#34192,#34193,#34194,#34195,#34196),.UNSPECIFIED.,.F.,.F.,(4,3,3,
3,3,3,3,4),(-85.3801244850391,-84.945441353114,-83.9460832195479,-82.9467250859819,
-81.9473669524158,-80.9480088188498,-79.9486506852837,-79.0969391778595),
 .UNSPECIFIED.);
#655=B_SPLINE_CURVE_WITH_KNOTS('',3,(#34197,#34198,#34199,#34200,#34201,
#34202,#34203,#34204,#34205,#34206,#34207,#34208,#34209,#34210,#34211,#34212,
#34213,#34214,#34215,#34216,#34217,#34218,#34219,#34220,#34221),
 .UNSPECIFIED.,.F.,.F.,(4,3,3,3,3,3,3,3,4),(75.8412843567096,75.9512181510196,
76.9505762845857,77.9499344181517,78.9492925517178,79.9486506852838,80.9480088188499,
81.9473669524159,82.1244696638892),.UNSPECIFIED.);
#656=B_SPLINE_CURVE_WITH_KNOTS('',3,(#34226,#34227,#34228,#34229,#34230,
#34231,#34232,#34233,#34234,#34235,#34236,#34237,#34238,#34239,#34240,#34241,
#34242,#34243,#34244,#34245,#34246,#34247),.UNSPECIFIED.,.F.,.F.,(4,3,3,
3,3,3,3,4),(-91.6633097922187,-90.9415901545102,-89.9422320209442,-88.9428738873782,
-87.9435157538121,-86.944157620246,-85.94479948668,-85.3801244850391),
 .UNSPECIFIED.);
#657=B_SPLINE_CURVE_WITH_KNOTS('',3,(#34248,#34249,#34250,#34251,#34252,
#34253,#34254,#34255,#34256,#34257,#34258,#34259,#34260,#34261,#34262,#34263,
#34264,#34265,#34266,#34267,#34268,#34269),.UNSPECIFIED.,.F.,.F.,(4,3,3,
3,3,3,3,4),(82.1244696638892,82.946725085982,83.946083219548,84.9454413531141,
85.9447994866801,86.9441576202461,87.9435157538122,88.4076549710687),
 .UNSPECIFIED.);
#658=B_SPLINE_CURVE_WITH_KNOTS('',3,(#34274,#34275,#34276,#34277,#34278,
#34279,#34280,#34281,#34282,#34283,#34284,#34285,#34286,#34287,#34288,#34289,
#34290,#34291,#34292,#34293,#34294,#34295,#34296,#34297,#34298),
 .UNSPECIFIED.,.F.,.F.,(4,3,3,3,3,3,3,3,4),(-97.9464950993983,-97.9370970894726,
-96.9377389559065,-95.9383808223405,-94.9390226887744,-93.9396645552084,
-92.9403064216423,-91.9409482880763,-91.6633097922187),.UNSPECIFIED.);
#659=B_SPLINE_CURVE_WITH_KNOTS('',3,(#34299,#34300,#34301,#34302,#34303,
#34304,#34305,#34306,#34307,#34308,#34309,#34310,#34311,#34312,#34313,#34314,
#34315,#34316,#34317,#34318,#34319,#34320),.UNSPECIFIED.,.F.,.F.,(4,3,3,
3,3,3,3,4),(88.4076549710687,88.9428738873782,89.9422320209442,90.9415901545103,
91.9409482880763,92.9403064216424,93.9396645552084,94.6908402782483),
 .UNSPECIFIED.);
#660=B_SPLINE_CURVE_WITH_KNOTS('',3,(#34325,#34326,#34327,#34328,#34329,
#34330,#34331,#34332,#34333,#34334,#34335,#34336,#34337,#34338,#34339,#34340,
#34341,#34342,#34343,#34344,#34345,#34346),.UNSPECIFIED.,.F.,.F.,(4,3,3,
3,3,3,3,4),(-104.229680406578,-103.933245890869,-102.933887757303,-101.934529623737,
-100.935171490171,-99.9358133566047,-98.9364552230386,-97.9464950993983),
 .UNSPECIFIED.);
#661=B_SPLINE_CURVE_WITH_KNOTS('',3,(#34347,#34348,#34349,#34350,#34351,
#34352,#34353,#34354,#34355,#34356,#34357,#34358,#34359,#34360,#34361,#34362,
#34363,#34364,#34365,#34366,#34367,#34368,#34369,#34370,#34371),
 .UNSPECIFIED.,.F.,.F.,(4,3,3,3,3,3,3,3,4),(94.6908402782483,94.9390226887745,
95.9383808223405,96.9377389559065,97.9370970894726,98.9364552230386,99.9358133566047,
100.935171490171,100.974025585428),.UNSPECIFIED.);
#662=B_SPLINE_CURVE_WITH_KNOTS('',3,(#34376,#34377,#34378,#34379,#34380,
#34381,#34382,#34383,#34384,#34385,#34386,#34387,#34388,#34389,#34390,#34391,
#34392,#34393,#34394,#34395,#34396,#34397),.UNSPECIFIED.,.F.,.F.,(4,3,3,
3,3,3,3,4),(-110.512865713757,-109.929394692265,-108.930036558699,-107.930678425133,
-106.931320291567,-105.931962158001,-104.932604024435,-104.229680406578),
 .UNSPECIFIED.);
#663=B_SPLINE_CURVE_WITH_KNOTS('',3,(#34398,#34399,#34400,#34401,#34402,
#34403,#34404,#34405,#34406,#34407,#34408,#34409,#34410,#34411,#34412,#34413,
#34414,#34415,#34416,#34417,#34418,#34419),.UNSPECIFIED.,.F.,.F.,(4,3,3,
3,3,3,3,4),(100.974025585428,101.934529623737,102.933887757303,103.933245890869,
104.932604024435,105.931962158001,106.931320291567,107.257210892608),
 .UNSPECIFIED.);
#664=B_SPLINE_CURVE_WITH_KNOTS('',3,(#34424,#34425,#34426,#34427,#34428,
#34429,#34430,#34431,#34432,#34433,#34434,#34435,#34436,#34437,#34438,#34439,
#34440,#34441,#34442,#34443,#34444,#34445),.UNSPECIFIED.,.F.,.F.,(4,3,3,
3,3,3,3,4),(-116.796051020937,-115.925543493661,-114.926185360095,-113.926827226529,
-112.927469092963,-111.928110959397,-110.928752825831,-110.512865713757),
 .UNSPECIFIED.);
#665=B_SPLINE_CURVE_WITH_KNOTS('',3,(#34446,#34447,#34448,#34449,#34450,
#34451,#34452,#34453,#34454,#34455,#34456,#34457,#34458,#34459,#34460,#34461,
#34462,#34463,#34464,#34465,#34466,#34467),.UNSPECIFIED.,.F.,.F.,(4,3,3,
3,3,3,3,4),(107.257210892608,107.930678425133,108.930036558699,109.929394692265,
110.928752825831,111.928110959397,112.927469092963,113.540396199787),
 .UNSPECIFIED.);
#666=B_SPLINE_CURVE_WITH_KNOTS('',3,(#34472,#34473,#34474,#34475,#34476,
#34477,#34478,#34479,#34480,#34481,#34482,#34483,#34484,#34485,#34486,#34487,
#34488,#34489,#34490,#34491,#34492,#34493,#34494,#34495,#34496),
 .UNSPECIFIED.,.F.,.F.,(4,3,3,3,3,3,3,3,4),(-123.079236328117,-122.921050428624,
-121.921692295058,-120.922334161492,-119.922976027926,-118.92361789436,
-117.924259760793,-116.924901627227,-116.796051020937),.UNSPECIFIED.);
#667=B_SPLINE_CURVE_WITH_KNOTS('',3,(#34497,#34498,#34499,#34500,#34501,
#34502,#34503,#34504,#34505,#34506,#34507,#34508,#34509,#34510,#34511,#34512,
#34513,#34514,#34515,#34516,#34517,#34518),.UNSPECIFIED.,.F.,.F.,(4,3,3,
3,3,3,3,4),(113.540396199787,113.926827226529,114.926185360095,115.925543493661,
116.924901627228,117.924259760794,118.92361789436,119.823581506967),
 .UNSPECIFIED.);
#668=B_SPLINE_CURVE_WITH_KNOTS('',3,(#34523,#34524,#34525,#34526,#34527,
#34528,#34529,#34530,#34531,#34532,#34533,#34534,#34535,#34536,#34537,#34538,
#34539,#34540,#34541,#34542,#34543,#34544),.UNSPECIFIED.,.F.,.F.,(4,3,3,
3,3,3,3,4),(-129.362421635296,-128.91719923002,-127.917841096454,-126.918482962888,
-125.919124829322,-124.919766695756,-123.92040856219,-123.079236328117),
 .UNSPECIFIED.);
#669=B_SPLINE_CURVE_WITH_KNOTS('',3,(#34545,#34546,#34547,#34548,#34549,
#34550,#34551,#34552,#34553,#34554,#34555,#34556,#34557,#34558,#34559,#34560,
#34561,#34562,#34563,#34564,#34565,#34566,#34567,#34568,#34569),
 .UNSPECIFIED.,.F.,.F.,(4,3,3,3,3,3,3,3,4),(119.823581506967,119.922976027926,
120.922334161492,121.921692295058,122.921050428624,123.92040856219,124.919766695756,
125.919124829322,126.106766814146),.UNSPECIFIED.);
#670=B_SPLINE_CURVE_WITH_KNOTS('',3,(#34574,#34575,#34576,#34577,#34578,
#34579,#34580,#34581,#34582,#34583,#34584,#34585,#34586,#34587,#34588,#34589,
#34590,#34591,#34592,#34593,#34594,#34595),.UNSPECIFIED.,.F.,.F.,(4,3,3,
3,3,3,3,4),(-135.645606942476,-134.913348031416,-133.91398989785,-132.914631764284,
-131.915273630718,-130.915915497152,-129.916557363586,-129.362421635296),
 .UNSPECIFIED.);
#671=B_SPLINE_CURVE_WITH_KNOTS('',3,(#34596,#34597,#34598,#34599,#34600,
#34601,#34602,#34603,#34604,#34605,#34606,#34607,#34608,#34609,#34610,#34611,
#34612,#34613,#34614,#34615,#34616,#34617),.UNSPECIFIED.,.F.,.F.,(4,3,3,
3,3,3,3,4),(126.106766814146,126.918482962888,127.917841096454,128.91719923002,
129.916557363586,130.915915497152,131.915273630718,132.389952121326),
 .UNSPECIFIED.);
#672=B_SPLINE_CURVE_WITH_KNOTS('',3,(#34622,#34623,#34624,#34625,#34626,
#34627,#34628,#34629,#34630,#34631,#34632,#34633,#34634,#34635,#34636,#34637,
#34638,#34639,#34640,#34641,#34642,#34643,#34644,#34645,#34646),
 .UNSPECIFIED.,.F.,.F.,(4,3,3,3,3,3,3,3,4),(-141.928792249655,-141.908854966379,
-140.909496832813,-139.910138699247,-138.91078056568,-137.911422432114,
-136.912064298548,-135.912706164982,-135.645606942476),.UNSPECIFIED.);
#673=B_SPLINE_CURVE_WITH_KNOTS('',3,(#34647,#34648,#34649,#34650,#34651,
#34652,#34653,#34654,#34655,#34656,#34657,#34658,#34659,#34660,#34661,#34662,
#34663,#34664,#34665,#34666,#34667,#34668),.UNSPECIFIED.,.F.,.F.,(4,3,3,
3,3,3,3,4),(132.389952121326,132.914631764284,133.91398989785,134.913348031416,
135.912706164982,136.912064298549,137.911422432115,138.673137428505),
 .UNSPECIFIED.);
#674=B_SPLINE_CURVE_WITH_KNOTS('',3,(#34673,#34674,#34675,#34676,#34677,
#34678,#34679,#34680,#34681,#34682,#34683,#34684,#34685,#34686,#34687,#34688,
#34689,#34690,#34691,#34692,#34693,#34694),.UNSPECIFIED.,.F.,.F.,(4,3,3,
3,3,3,3,4),(-148.211977556835,-147.905003767775,-146.905645634209,-145.906287500643,
-144.906929367077,-143.907571233511,-142.908213099945,-141.928792249655),
 .UNSPECIFIED.);
#675=B_SPLINE_CURVE_WITH_KNOTS('',3,(#34695,#34696,#34697,#34698,#34699,
#34700,#34701,#34702,#34703,#34704,#34705,#34706,#34707,#34708,#34709,#34710,
#34711,#34712,#34713,#34714,#34715,#34716,#34717,#34718,#34719),
 .UNSPECIFIED.,.F.,.F.,(4,3,3,3,3,3,3,3,4),(138.673137428505,138.910780565681,
139.910138699247,140.909496832813,141.908854966379,142.908213099945,143.907571233511,
144.906929367077,144.956322735685),.UNSPECIFIED.);
#676=B_SPLINE_CURVE_WITH_KNOTS('',3,(#34724,#34725,#34726,#34727,#34728,
#34729,#34730,#34731,#34732,#34733,#34734,#34735,#34736,#34737,#34738,#34739,
#34740,#34741,#34742,#34743,#34744,#34745),.UNSPECIFIED.,.F.,.F.,(4,3,3,
3,3,3,3,4),(-154.495162864015,-153.901152569171,-152.901794435605,-151.902436302039,
-150.903078168473,-149.903720034907,-148.904361901341,-148.211977556835),
 .UNSPECIFIED.);
#677=B_SPLINE_CURVE_WITH_KNOTS('',3,(#34746,#34747,#34748,#34749,#34750,
#34751,#34752,#34753,#34754,#34755,#34756,#34757,#34758,#34759,#34760,#34761,
#34762,#34763,#34764,#34765,#34766,#34767),.UNSPECIFIED.,.F.,.F.,(4,3,3,
3,3,3,3,4),(144.956322735685,145.906287500643,146.905645634209,147.905003767775,
148.904361901341,149.903720034907,150.903078168473,151.239508042865),
 .UNSPECIFIED.);
#678=B_SPLINE_CURVE_WITH_KNOTS('',3,(#34772,#34773,#34774,#34775,#34776,
#34777,#34778,#34779,#34780,#34781,#34782,#34783,#34784,#34785,#34786,#34787,
#34788,#34789,#34790,#34791,#34792,#34793),.UNSPECIFIED.,.F.,.F.,(4,3,3,
3,3,3,3,4),(-160.778348171194,-159.897301370567,-158.897943237001,-157.898585103435,
-156.899226969869,-155.899868836303,-154.900510702737,-154.495162864015),
 .UNSPECIFIED.);
#679=B_SPLINE_CURVE_WITH_KNOTS('',3,(#34794,#34795,#34796,#34797,#34798,
#34799,#34800,#34801,#34802,#34803,#34804,#34805,#34806,#34807,#34808,#34809,
#34810,#34811,#34812,#34813,#34814,#34815),.UNSPECIFIED.,.F.,.F.,(4,3,3,
3,3,3,3,4),(151.239508042865,151.902436302039,152.901794435605,153.901152569171,
154.900510702737,155.899868836303,156.899226969869,157.522693350044),
 .UNSPECIFIED.);
#680=B_SPLINE_CURVE_WITH_KNOTS('',3,(#34820,#34821,#34822,#34823,#34824,
#34825,#34826,#34827,#34828,#34829,#34830,#34831,#34832,#34833,#34834,#34835,
#34836,#34837,#34838,#34839,#34840,#34841,#34842,#34843,#34844),
 .UNSPECIFIED.,.F.,.F.,(4,3,3,3,3,3,3,3,4),(-167.061533478374,-166.89280830553,
-165.893450171964,-164.894092038398,-163.894733904832,-162.895375771266,
-161.8960176377,-160.896659504134,-160.778348171194),.UNSPECIFIED.);
#681=B_SPLINE_CURVE_WITH_KNOTS('',3,(#34845,#34846,#34847,#34848,#34849,
#34850,#34851,#34852,#34853,#34854,#34855,#34856,#34857,#34858,#34859,#34860,
#34861,#34862,#34863,#34864,#34865,#34866),.UNSPECIFIED.,.F.,.F.,(4,3,3,
3,3,3,3,4),(157.522693350044,157.898585103435,158.897943237002,159.897301370568,
160.896659504134,161.8960176377,162.895375771266,163.805878657224),
 .UNSPECIFIED.);
#682=B_SPLINE_CURVE_WITH_KNOTS('',3,(#34871,#34872,#34873,#34874,#34875,
#34876,#34877,#34878,#34879,#34880,#34881,#34882,#34883,#34884,#34885,#34886,
#34887,#34888,#34889,#34890,#34891,#34892),.UNSPECIFIED.,.F.,.F.,(4,3,3,
3,3,3,3,4),(-173.344718785553,-172.888957106926,-171.88959897336,-170.890240839794,
-169.890882706228,-168.891524572662,-167.892166439096,-167.061533478374),
 .UNSPECIFIED.);
#683=B_SPLINE_CURVE_WITH_KNOTS('',3,(#34893,#34894,#34895,#34896,#34897,
#34898,#34899,#34900,#34901,#34902,#34903,#34904,#34905,#34906,#34907,#34908,
#34909,#34910,#34911,#34912,#34913,#34914,#34915,#34916,#34917),
 .UNSPECIFIED.,.F.,.F.,(4,3,3,3,3,3,3,3,4),(163.805878657224,163.894733904832,
164.894092038398,165.893450171964,166.89280830553,167.892166439096,168.891524572662,
169.890882706228,170.089063964403),.UNSPECIFIED.);
#684=B_SPLINE_CURVE_WITH_KNOTS('',3,(#34922,#34923,#34924,#34925,#34926,
#34927,#34928,#34929,#34930,#34931,#34932,#34933,#34934,#34935,#34936,#34937,
#34938,#34939,#34940,#34941,#34942,#34943),.UNSPECIFIED.,.F.,.F.,(4,3,3,
3,3,3,3,4),(-179.627904092733,-178.885105908322,-177.885747774756,-176.88638964119,
-175.887031507624,-174.887673374058,-173.888315240492,-173.344718785553),
 .UNSPECIFIED.);
#685=B_SPLINE_CURVE_WITH_KNOTS('',3,(#34944,#34945,#34946,#34947,#34948,
#34949,#34950,#34951,#34952,#34953,#34954,#34955,#34956,#34957,#34958,#34959,
#34960,#34961,#34962,#34963,#34964,#34965),.UNSPECIFIED.,.F.,.F.,(4,3,3,
3,3,3,3,4),(170.089063964403,170.890240839794,171.88959897336,172.888957106926,
173.888315240492,174.887673374058,175.887031507624,176.372249271583),
 .UNSPECIFIED.);
#686=B_SPLINE_CURVE_WITH_KNOTS('',3,(#34970,#34971,#34972,#34973,#34974,
#34975,#34976,#34977,#34978,#34979,#34980,#34981,#34982,#34983,#34984,#34985,
#34986,#34987,#34988,#34989,#34990,#34991,#34992,#34993,#34994),
 .UNSPECIFIED.,.F.,.F.,(4,3,3,3,3,3,3,3,4),(-185.911089399912,-185.880612843285,
-184.881254709719,-183.881896576153,-182.882538442587,-181.88318030902,
-180.883822175454,-179.884464041888,-179.627904092733),.UNSPECIFIED.);
#687=B_SPLINE_CURVE_WITH_KNOTS('',3,(#34995,#34996,#34997,#34998,#34999,
#35000,#35001,#35002,#35003,#35004,#35005,#35006,#35007,#35008,#35009,#35010,
#35011,#35012,#35013,#35014,#35015,#35016),.UNSPECIFIED.,.F.,.F.,(4,3,3,
3,3,3,3,4),(176.372249271583,176.88638964119,177.885747774756,178.885105908322,
179.884464041889,180.883822175455,181.883180309021,182.655434578762),
 .UNSPECIFIED.);
#688=B_SPLINE_CURVE_WITH_KNOTS('',3,(#35021,#35022,#35023,#35024,#35025,
#35026,#35027,#35028,#35029,#35030,#35031,#35032,#35033,#35034,#35035,#35036,
#35037,#35038,#35039,#35040,#35041,#35042),.UNSPECIFIED.,.F.,.F.,(4,3,3,
3,3,3,3,4),(-192.194274707092,-191.876761644681,-190.877403511115,-189.878045377549,
-188.878687243983,-187.879329110417,-186.879970976851,-185.911089399912),
 .UNSPECIFIED.);
#689=B_SPLINE_CURVE_WITH_KNOTS('',3,(#35043,#35044,#35045,#35046,#35047,
#35048,#35049,#35050,#35051,#35052,#35053,#35054,#35055,#35056,#35057,#35058,
#35059,#35060,#35061,#35062,#35063,#35064,#35065,#35066,#35067),
 .UNSPECIFIED.,.F.,.F.,(4,3,3,3,3,3,3,3,4),(182.655434578762,182.882538442587,
183.881896576153,184.881254709719,185.880612843285,186.879970976851,187.879329110417,
188.878687243983,188.938619885942),.UNSPECIFIED.);
#690=B_SPLINE_CURVE_WITH_KNOTS('',3,(#35072,#35073,#35074,#35075,#35076,
#35077,#35078,#35079,#35080,#35081,#35082,#35083,#35084,#35085,#35086,#35087,
#35088,#35089,#35090,#35091,#35092,#35093),.UNSPECIFIED.,.F.,.F.,(4,3,3,
3,3,3,3,4),(-198.477460014271,-197.872910446077,-196.873552312511,-195.874194178945,
-194.874836045379,-193.875477911813,-192.876119778247,-192.194274707092),
 .UNSPECIFIED.);
#691=B_SPLINE_CURVE_WITH_KNOTS('',3,(#35094,#35095,#35096,#35097,#35098,
#35099,#35100,#35101,#35102,#35103,#35104,#35105,#35106,#35107,#35108,#35109,
#35110,#35111,#35112,#35113,#35114,#35115),.UNSPECIFIED.,.F.,.F.,(4,3,3,
3,3,3,3,4),(188.938619885942,189.878045377549,190.877403511115,191.876761644681,
192.876119778247,193.875477911813,194.874836045379,195.221805193122),
 .UNSPECIFIED.);
#692=B_SPLINE_CURVE_WITH_KNOTS('',3,(#35120,#35121,#35122,#35123,#35124,
#35125,#35126,#35127,#35128,#35129,#35130,#35131,#35132,#35133,#35134,#35135,
#35136,#35137,#35138,#35139,#35140,#35141),.UNSPECIFIED.,.F.,.F.,(4,3,3,
3,3,3,3,4),(-204.760645321451,-203.869059247473,-202.869701113907,-201.870342980341,
-200.870984846775,-199.871626713209,-198.872268579643,-198.477460014271),
 .UNSPECIFIED.);
#693=B_SPLINE_CURVE_WITH_KNOTS('',3,(#35142,#35143,#35144,#35145,#35146,
#35147,#35148,#35149,#35150,#35151,#35152,#35153,#35154,#35155,#35156,#35157,
#35158,#35159,#35160,#35161,#35162,#35163),.UNSPECIFIED.,.F.,.F.,(4,3,3,
3,3,3,3,4),(195.221805193122,195.874194178945,196.873552312511,197.872910446077,
198.872268579643,199.871626713209,200.870984846776,201.504990500301),
 .UNSPECIFIED.);
#694=B_SPLINE_CURVE_WITH_KNOTS('',3,(#35168,#35169,#35170,#35171,#35172,
#35173,#35174,#35175,#35176,#35177,#35178,#35179,#35180,#35181,#35182,#35183,
#35184,#35185,#35186,#35187,#35188,#35189,#35190,#35191,#35192),
 .UNSPECIFIED.,.F.,.F.,(4,3,3,3,3,3,3,3,4),(-211.043830628631,-210.864566182436,
-209.86520804887,-208.865849915304,-207.866491781738,-206.867133648172,
-205.867775514606,-204.86841738104,-204.760645321451),.UNSPECIFIED.);
#695=B_SPLINE_CURVE_WITH_KNOTS('',3,(#35193,#35194,#35195,#35196,#35197,
#35198,#35199,#35200,#35201,#35202,#35203,#35204,#35205,#35206,#35207,#35208,
#35209,#35210,#35211,#35212,#35213,#35214),.UNSPECIFIED.,.F.,.F.,(4,3,3,
3,3,3,3,4),(201.504990500301,201.870342980342,202.869701113908,203.869059247474,
204.86841738104,205.867775514606,206.867133648172,207.788175807481),
 .UNSPECIFIED.);
#696=B_SPLINE_CURVE_WITH_KNOTS('',3,(#35219,#35220,#35221,#35222,#35223,
#35224,#35225,#35226,#35227,#35228,#35229,#35230,#35231,#35232,#35233,#35234,
#35235,#35236,#35237,#35238,#35239,#35240),.UNSPECIFIED.,.F.,.F.,(4,3,3,
3,3,3,3,4),(-217.32701593581,-216.860714983832,-215.861356850266,-214.8619987167,
-213.862640583134,-212.863282449568,-211.863924316002,-211.043830628631),
 .UNSPECIFIED.);
#697=B_SPLINE_CURVE_WITH_KNOTS('',3,(#35241,#35242,#35243,#35244,#35245,
#35246,#35247,#35248,#35249,#35250,#35251,#35252,#35253,#35254,#35255,#35256,
#35257,#35258,#35259,#35260,#35261,#35262,#35263,#35264,#35265),
 .UNSPECIFIED.,.F.,.F.,(4,3,3,3,3,3,3,3,4),(207.788175807481,207.866491781738,
208.865849915304,209.86520804887,210.864566182436,211.863924316002,212.863282449568,
213.862640583134,214.07136111466),.UNSPECIFIED.);
#698=B_SPLINE_CURVE_WITH_KNOTS('',3,(#35270,#35271,#35272,#35273,#35274,
#35275,#35276,#35277,#35278,#35279,#35280,#35281,#35282,#35283,#35284,#35285,
#35286,#35287,#35288,#35289,#35290,#35291),.UNSPECIFIED.,.F.,.F.,(4,3,3,
3,3,3,3,4),(-223.61020124299,-222.856863785228,-221.857505651662,-220.858147518096,
-219.85878938453,-218.859431250964,-217.860073117398,-217.32701593581),
 .UNSPECIFIED.);
#699=B_SPLINE_CURVE_WITH_KNOTS('',3,(#35292,#35293,#35294,#35295,#35296,
#35297,#35298,#35299,#35300,#35301,#35302,#35303,#35304,#35305,#35306,#35307,
#35308,#35309,#35310,#35311,#35312,#35313),.UNSPECIFIED.,.F.,.F.,(4,3,3,
3,3,3,3,4),(214.07136111466,214.8619987167,215.861356850266,216.860714983832,
217.860073117398,218.859431250964,219.85878938453,220.35454642184),
 .UNSPECIFIED.);
#700=B_SPLINE_CURVE_WITH_KNOTS('',3,(#35318,#35319,#35320,#35321,#35322,
#35323,#35324,#35325,#35326,#35327,#35328,#35329,#35330,#35331,#35332,#35333,
#35334,#35335,#35336,#35337,#35338,#35339,#35340,#35341,#35342),
 .UNSPECIFIED.,.F.,.F.,(4,3,3,3,3,3,3,3,4),(-229.893386550169,-229.852370720191,
-228.853012586625,-227.853654453059,-226.854296319493,-225.854938185927,
-224.85558005236,-223.856221918794,-223.61020124299),.UNSPECIFIED.);
#701=B_SPLINE_CURVE_WITH_KNOTS('',3,(#35343,#35344,#35345,#35346,#35347,
#35348,#35349,#35350,#35351,#35352,#35353,#35354,#35355,#35356,#35357,#35358,
#35359,#35360,#35361,#35362,#35363,#35364),.UNSPECIFIED.,.F.,.F.,(4,3,3,
3,3,3,3,4),(220.35454642184,220.858147518096,221.857505651663,222.856863785229,
223.856221918795,224.855580052361,225.854938185927,226.637731729019),
 .UNSPECIFIED.);
#702=B_SPLINE_CURVE_WITH_KNOTS('',3,(#35369,#35370,#35371,#35372,#35373,
#35374,#35375,#35376,#35377,#35378,#35379,#35380,#35381,#35382,#35383,#35384,
#35385,#35386,#35387,#35388,#35389,#35390),.UNSPECIFIED.,.F.,.F.,(4,3,3,
3,3,3,3,4),(-236.176571857349,-235.848519521587,-234.849161388021,-233.849803254455,
-232.850445120889,-231.851086987323,-230.851728853757,-229.893386550169),
 .UNSPECIFIED.);
#703=B_SPLINE_CURVE_WITH_KNOTS('',3,(#35391,#35392,#35393,#35394,#35395,
#35396,#35397,#35398,#35399,#35400,#35401,#35402,#35403,#35404,#35405,#35406,
#35407,#35408,#35409,#35410,#35411,#35412,#35413,#35414,#35415),
 .UNSPECIFIED.,.F.,.F.,(4,3,3,3,3,3,3,3,4),(226.637731729019,226.854296319493,
227.853654453059,228.853012586625,229.852370720191,230.851728853757,231.851086987323,
232.850445120889,232.920917036199),.UNSPECIFIED.);
#704=B_SPLINE_CURVE_WITH_KNOTS('',3,(#35420,#35421,#35422,#35423,#35424,
#35425,#35426,#35427,#35428,#35429,#35430,#35431,#35432,#35433,#35434,#35435,
#35436,#35437,#35438,#35439,#35440,#35441),.UNSPECIFIED.,.F.,.F.,(4,3,3,
3,3,3,3,4),(-242.459757164528,-241.844668322983,-240.845310189417,-239.845952055851,
-238.846593922285,-237.847235788719,-236.847877655153,-236.176571857349),
 .UNSPECIFIED.);
#705=B_SPLINE_CURVE_WITH_KNOTS('',3,(#35442,#35443,#35444,#35445,#35446,
#35447,#35448,#35449,#35450,#35451,#35452,#35453,#35454,#35455,#35456,#35457,
#35458,#35459,#35460,#35461,#35462,#35463),.UNSPECIFIED.,.F.,.F.,(4,3,3,
3,3,3,3,4),(232.920917036199,233.849803254455,234.849161388021,235.848519521587,
236.847877655153,237.847235788719,238.846593922285,239.204102343378),
 .UNSPECIFIED.);
#706=B_SPLINE_CURVE_WITH_KNOTS('',3,(#35468,#35469,#35470,#35471,#35472,
#35473,#35474,#35475,#35476,#35477,#35478,#35479,#35480,#35481,#35482,#35483,
#35484,#35485,#35486,#35487,#35488,#35489),.UNSPECIFIED.,.F.,.F.,(4,3,3,
3,3,3,3,4),(-248.742942471708,-247.84081712438,-246.841458990814,-245.842100857247,
-244.842742723681,-243.843384590115,-242.844026456549,-242.459757164528),
 .UNSPECIFIED.);
#707=B_SPLINE_CURVE_WITH_KNOTS('',3,(#35490,#35491,#35492,#35493,#35494,
#35495,#35496,#35497,#35498,#35499,#35500,#35501,#35502,#35503,#35504,#35505,
#35506,#35507,#35508,#35509,#35510,#35511),.UNSPECIFIED.,.F.,.F.,(4,3,3,
3,3,3,3,4),(239.204102343378,239.845952055851,240.845310189417,241.844668322983,
242.84402645655,243.843384590116,244.842742723682,245.487287650558),
 .UNSPECIFIED.);
#708=B_SPLINE_CURVE_WITH_KNOTS('',3,(#35516,#35517,#35518,#35519,#35520,
#35521,#35522,#35523,#35524,#35525,#35526,#35527,#35528,#35529,#35530,#35531,
#35532,#35533,#35534,#35535,#35536,#35537,#35538,#35539,#35540),
 .UNSPECIFIED.,.F.,.F.,(4,3,3,3,3,3,3,3,4),(-255.026127778888,-254.836324059342,
-253.836965925776,-252.83760779221,-251.838249658644,-250.838891525078,
-249.839533391512,-248.840175257946,-248.742942471708),.UNSPECIFIED.);
#709=B_SPLINE_CURVE_WITH_KNOTS('',3,(#35541,#35542,#35543,#35544,#35545,
#35546,#35547,#35548,#35549,#35550,#35551,#35552,#35553,#35554,#35555,#35556,
#35557,#35558,#35559,#35560,#35561,#35562),.UNSPECIFIED.,.F.,.F.,(4,3,3,
3,3,3,3,4),(245.487287650558,245.842100857248,246.841458990814,247.84081712438,
248.840175257946,249.839533391512,250.838891525078,251.770472957738),
 .UNSPECIFIED.);
#710=B_SPLINE_CURVE_WITH_KNOTS('',3,(#35567,#35568,#35569,#35570,#35571,
#35572,#35573,#35574,#35575,#35576,#35577,#35578,#35579,#35580,#35581,#35582,
#35583,#35584,#35585,#35586,#35587,#35588),.UNSPECIFIED.,.F.,.F.,(4,3,3,
3,3,3,3,4),(-261.309313086067,-260.832472860738,-259.833114727172,-258.833756593606,
-257.83439846004,-256.835040326474,-255.835682192908,-255.026127778888),
 .UNSPECIFIED.);
#711=B_SPLINE_CURVE_WITH_KNOTS('',3,(#35589,#35590,#35591,#35592,#35593,
#35594,#35595,#35596,#35597,#35598,#35599,#35600,#35601,#35602,#35603,#35604,
#35605,#35606,#35607,#35608,#35609,#35610,#35611,#35612,#35613),
 .UNSPECIFIED.,.F.,.F.,(4,3,3,3,3,3,3,3,4),(251.770472957738,251.838249658644,
252.83760779221,253.836965925776,254.836324059342,255.835682192908,256.835040326474,
257.83439846004,258.053658264917),.UNSPECIFIED.);
#712=B_SPLINE_CURVE_WITH_KNOTS('',3,(#35618,#35619,#35620,#35621,#35622,
#35623,#35624,#35625,#35626,#35627,#35628,#35629,#35630,#35631,#35632,#35633,
#35634,#35635,#35636,#35637,#35638,#35639),.UNSPECIFIED.,.F.,.F.,(4,3,3,
3,3,3,3,4),(-267.592498393247,-266.828621662134,-265.829263528568,-264.829905395002,
-263.830547261436,-262.83118912787,-261.831830994304,-261.309313086067),
 .UNSPECIFIED.);
#713=B_SPLINE_CURVE_WITH_KNOTS('',3,(#35640,#35641,#35642,#35643,#35644,
#35645,#35646,#35647,#35648,#35649,#35650,#35651,#35652,#35653,#35654,#35655,
#35656,#35657,#35658,#35659,#35660,#35661),.UNSPECIFIED.,.F.,.F.,(4,3,3,
3,3,3,3,4),(258.053658264917,258.833756593606,259.833114727172,260.832472860738,
261.831830994304,262.83118912787,263.830547261436,264.336843572097),
 .UNSPECIFIED.);
#714=B_SPLINE_CURVE_WITH_KNOTS('',3,(#35666,#35667,#35668,#35669,#35670,
#35671,#35672,#35673,#35674,#35675,#35676,#35677,#35678,#35679,#35680,#35681,
#35682,#35683,#35684,#35685,#35686,#35687,#35688,#35689,#35690),
 .UNSPECIFIED.,.F.,.F.,(4,3,3,3,3,3,3,3,4),(-273.875683700426,-273.824128597097,
-272.824770463531,-271.825412329965,-270.826054196399,-269.826696062833,
-268.827337929266,-267.8279797957,-267.592498393247),.UNSPECIFIED.);
#715=B_SPLINE_CURVE_WITH_KNOTS('',3,(#35691,#35692,#35693,#35694,#35695,
#35696,#35697,#35698,#35699,#35700,#35701,#35702,#35703,#35704,#35705,#35706,
#35707,#35708,#35709,#35710,#35711,#35712),.UNSPECIFIED.,.F.,.F.,(4,3,3,
3,3,3,3,4),(264.336843572097,264.829905395003,265.829263528569,266.828621662135,
267.827979795701,268.827337929267,269.826696062833,270.620028879276),
 .UNSPECIFIED.);
#716=B_SPLINE_CURVE_WITH_KNOTS('',3,(#35717,#35718,#35719,#35720,#35721,
#35722,#35723,#35724,#35725,#35726,#35727,#35728,#35729,#35730,#35731,#35732,
#35733,#35734,#35735,#35736,#35737,#35738),.UNSPECIFIED.,.F.,.F.,(4,3,3,
3,3,3,3,4),(-280.158869007606,-279.820277398493,-278.820919264927,-277.821561131361,
-276.822202997795,-275.822844864229,-274.823486730663,-273.875683700426),
 .UNSPECIFIED.);
#717=B_SPLINE_CURVE_WITH_KNOTS('',3,(#35739,#35740,#35741,#35742,#35743,
#35744,#35745,#35746,#35747,#35748,#35749,#35750,#35751,#35752,#35753,#35754,
#35755,#35756,#35757,#35758,#35759,#35760,#35761,#35762,#35763),
 .UNSPECIFIED.,.F.,.F.,(4,3,3,3,3,3,3,3,4),(270.620028879276,270.826054196399,
271.825412329965,272.824770463531,273.824128597097,274.823486730663,275.822844864229,
276.822202997795,276.903214186456),.UNSPECIFIED.);
#718=B_SPLINE_CURVE_WITH_KNOTS('',3,(#35768,#35769,#35770,#35771,#35772,
#35773,#35774,#35775,#35776,#35777,#35778,#35779,#35780,#35781,#35782,#35783,
#35784,#35785,#35786,#35787,#35788,#35789),.UNSPECIFIED.,.F.,.F.,(4,3,3,
3,3,3,3,4),(-286.442054314785,-285.816426199889,-284.817068066323,-283.817709932757,
-282.818351799191,-281.818993665625,-280.819635532059,-280.158869007606),
 .UNSPECIFIED.);
#719=B_SPLINE_CURVE_WITH_KNOTS('',3,(#35790,#35791,#35792,#35793,#35794,
#35795,#35796,#35797,#35798,#35799,#35800,#35801,#35802,#35803,#35804,#35805,
#35806,#35807,#35808,#35809,#35810,#35811),.UNSPECIFIED.,.F.,.F.,(4,3,3,
3,3,3,3,4),(276.903214186456,277.821561131361,278.820919264927,279.820277398493,
280.819635532059,281.818993665625,282.818351799191,283.186399493635),
 .UNSPECIFIED.);
#720=B_SPLINE_CURVE_WITH_KNOTS('',3,(#35816,#35817,#35818,#35819,#35820,
#35821,#35822,#35823,#35824,#35825,#35826,#35827,#35828,#35829,#35830,#35831,
#35832,#35833,#35834,#35835,#35836,#35837),.UNSPECIFIED.,.F.,.F.,(4,3,3,
3,3,3,3,4),(-292.725239621965,-291.812575001286,-290.81321686772,-289.813858734153,
-288.814500600587,-287.815142467021,-286.815784333455,-286.442054314785),
 .UNSPECIFIED.);
#721=B_SPLINE_CURVE_WITH_KNOTS('',3,(#35838,#35839,#35840,#35841,#35842,
#35843,#35844,#35845,#35846,#35847,#35848,#35849,#35850,#35851,#35852,#35853,
#35854,#35855,#35856,#35857,#35858,#35859),.UNSPECIFIED.,.F.,.F.,(4,3,3,
3,3,3,3,4),(283.186399493635,283.817709932757,284.817068066323,285.81642619989,
286.815784333456,287.815142467022,288.814500600588,289.469584800815),
 .UNSPECIFIED.);
#722=B_SPLINE_CURVE_WITH_KNOTS('',3,(#35864,#35865,#35866,#35867,#35868,
#35869,#35870,#35871,#35872,#35873,#35874,#35875,#35876,#35877,#35878,#35879,
#35880,#35881,#35882,#35883,#35884,#35885,#35886,#35887,#35888),
 .UNSPECIFIED.,.F.,.F.,(4,3,3,3,3,3,3,3,4),(-299.008424929145,-298.808081936248,
-297.808723802682,-296.809365669116,-295.81000753555,-294.810649401984,
-293.811291268418,-292.811933134852,-292.725239621965),.UNSPECIFIED.);
#723=B_SPLINE_CURVE_WITH_KNOTS('',3,(#35889,#35890,#35891,#35892,#35893,
#35894,#35895,#35896,#35897,#35898,#35899,#35900,#35901,#35902,#35903,#35904,
#35905,#35906,#35907,#35908,#35909,#35910),.UNSPECIFIED.,.F.,.F.,(4,3,3,
3,3,3,3,4),(289.469584800815,289.813858734154,290.81321686772,291.812575001286,
292.811933134852,293.811291268418,294.810649401984,295.752770107995),
 .UNSPECIFIED.);
#724=B_SPLINE_CURVE_WITH_KNOTS('',3,(#35915,#35916,#35917,#35918,#35919,
#35920,#35921,#35922,#35923,#35924,#35925,#35926,#35927,#35928,#35929,#35930,
#35931,#35932,#35933,#35934,#35935,#35936),.UNSPECIFIED.,.F.,.F.,(4,3,3,
3,3,3,3,4),(-305.291610236324,-304.804230737644,-303.804872604078,-302.805514470512,
-301.806156336946,-300.80679820338,-299.807440069814,-299.008424929145),
 .UNSPECIFIED.);
#725=B_SPLINE_CURVE_WITH_KNOTS('',3,(#35937,#35938,#35939,#35940,#35941,
#35942,#35943,#35944,#35945,#35946,#35947,#35948,#35949,#35950,#35951,#35952,
#35953,#35954,#35955,#35956,#35957,#35958,#35959,#35960,#35961),
 .UNSPECIFIED.,.F.,.F.,(4,3,3,3,3,3,3,3,4),(295.752770107995,295.81000753555,
296.809365669116,297.808723802682,298.808081936248,299.807440069814,300.80679820338,
301.806156336946,302.035955415174),.UNSPECIFIED.);
#726=B_SPLINE_CURVE_WITH_KNOTS('',3,(#35966,#35967,#35968,#35969,#35970,
#35971,#35972,#35973,#35974,#35975,#35976,#35977,#35978,#35979,#35980,#35981,
#35982,#35983,#35984,#35985,#35986,#35987),.UNSPECIFIED.,.F.,.F.,(4,3,3,
3,3,3,3,4),(-311.574795543504,-310.80037953904,-309.801021405475,-308.801663271908,
-307.802305138342,-306.802947004776,-305.80358887121,-305.291610236324),
 .UNSPECIFIED.);
#727=B_SPLINE_CURVE_WITH_KNOTS('',3,(#35988,#35989,#35990,#35991,#35992,
#35993,#35994,#35995,#35996,#35997,#35998,#35999,#36000,#36001,#36002,#36003,
#36004,#36005,#36006,#36007,#36008,#36009),.UNSPECIFIED.,.F.,.F.,(4,3,3,
3,3,3,3,4),(302.035955415174,302.805514470512,303.804872604078,304.804230737644,
305.80358887121,306.802947004777,307.802305138343,308.319140722354),
 .UNSPECIFIED.);
#728=B_SPLINE_CURVE_WITH_KNOTS('',3,(#36014,#36015,#36016,#36017,#36018,
#36019,#36020,#36021,#36022,#36023,#36024,#36025,#36026,#36027,#36028,#36029,
#36030,#36031,#36032,#36033,#36034,#36035,#36036,#36037,#36038),
 .UNSPECIFIED.,.F.,.F.,(4,3,3,3,3,3,3,3,4),(-317.857980850683,-317.795886474003,
-316.796528340437,-315.797170206871,-314.797812073305,-313.798453939739,
-312.799095806173,-311.799737672607,-311.574795543504),.UNSPECIFIED.);
#729=B_SPLINE_CURVE_WITH_KNOTS('',3,(#36039,#36040,#36041,#36042,#36043,
#36044,#36045,#36046,#36047,#36048,#36049,#36050,#36051,#36052,#36053,#36054,
#36055,#36056,#36057,#36058,#36059,#36060),.UNSPECIFIED.,.F.,.F.,(4,3,3,
3,3,3,3,4),(308.319140722354,308.801663271909,309.801021405475,310.800379539041,
311.799737672607,312.799095806173,313.798453939739,314.602326029533),
 .UNSPECIFIED.);
#730=B_SPLINE_CURVE_WITH_KNOTS('',3,(#36065,#36066,#36067,#36068,#36069,
#36070,#36071,#36072,#36073,#36074,#36075,#36076,#36077,#36078,#36079,#36080,
#36081,#36082,#36083,#36084,#36085,#36086),.UNSPECIFIED.,.F.,.F.,(4,3,3,
3,3,3,3,4),(-324.141166157863,-323.792035275399,-322.792677141833,-321.793319008267,
-320.793960874701,-319.794602741135,-318.795244607569,-317.857980850683),
 .UNSPECIFIED.);
#731=B_SPLINE_CURVE_WITH_KNOTS('',3,(#36087,#36088,#36089,#36090,#36091,
#36092,#36093,#36094,#36095,#36096,#36097,#36098,#36099,#36100,#36101,#36102,
#36103,#36104,#36105,#36106,#36107,#36108,#36109,#36110,#36111),
 .UNSPECIFIED.,.F.,.F.,(4,3,3,3,3,3,3,3,4),(314.602326029533,314.797812073305,
315.797170206871,316.796528340437,317.795886474003,318.795244607569,319.794602741135,
320.793960874701,320.885511336713),.UNSPECIFIED.);
#732=B_SPLINE_CURVE_WITH_KNOTS('',3,(#36116,#36117,#36118,#36119,#36120,
#36121,#36122,#36123,#36124,#36125,#36126,#36127,#36128,#36129,#36130,#36131,
#36132,#36133,#36134,#36135,#36136,#36137),.UNSPECIFIED.,.F.,.F.,(4,3,3,
3,3,3,3,4),(-330.424351465042,-329.788184076795,-328.788825943229,-327.789467809663,
-326.790109676097,-325.790751542531,-324.791393408965,-324.141166157863),
 .UNSPECIFIED.);
#733=B_SPLINE_CURVE_WITH_KNOTS('',3,(#36138,#36139,#36140,#36141,#36142,
#36143,#36144,#36145,#36146,#36147,#36148,#36149,#36150,#36151,#36152,#36153,
#36154,#36155,#36156,#36157,#36158,#36159),.UNSPECIFIED.,.F.,.F.,(4,3,3,
3,3,3,3,4),(320.885511336713,321.793319008267,322.792677141833,323.792035275399,
324.791393408965,325.790751542531,326.790109676097,327.168696643892),
 .UNSPECIFIED.);
#734=B_SPLINE_CURVE_WITH_KNOTS('',3,(#36164,#36165,#36166,#36167,#36168,
#36169,#36170,#36171,#36172,#36173,#36174,#36175,#36176,#36177,#36178,#36179,
#36180,#36181,#36182,#36183,#36184,#36185),.UNSPECIFIED.,.F.,.F.,(4,3,3,
3,3,3,3,4),(-336.707536772222,-335.784332878192,-334.784974744626,-333.78561661106,
-332.786258477494,-331.786900343927,-330.787542210361,-330.424351465042),
 .UNSPECIFIED.);
#735=B_SPLINE_CURVE_WITH_KNOTS('',3,(#36186,#36187,#36188,#36189,#36190,
#36191,#36192,#36193,#36194,#36195,#36196,#36197,#36198,#36199,#36200,#36201,
#36202,#36203,#36204,#36205,#36206,#36207),.UNSPECIFIED.,.F.,.F.,(4,3,3,
3,3,3,3,4),(327.168696643892,327.789467809663,328.78882594323,329.788184076796,
330.787542210362,331.786900343928,332.786258477494,333.451881951072),
 .UNSPECIFIED.);
#736=B_SPLINE_CURVE_WITH_KNOTS('',3,(#36212,#36213,#36214,#36215,#36216,
#36217,#36218,#36219,#36220,#36221,#36222,#36223,#36224,#36225,#36226,#36227,
#36228,#36229,#36230,#36231,#36232,#36233,#36234,#36235,#36236),
 .UNSPECIFIED.,.F.,.F.,(4,3,3,3,3,3,3,3,4),(-342.990722079402,-342.779839813154,
-341.780481679588,-340.781123546022,-339.781765412456,-338.78240727889,
-337.783049145324,-336.783691011758,-336.707536772222),.UNSPECIFIED.);
#737=B_SPLINE_CURVE_WITH_KNOTS('',3,(#36237,#36238,#36239,#36240,#36241,
#36242,#36243,#36244,#36245,#36246,#36247,#36248,#36249,#36250,#36251,#36252,
#36253,#36254,#36255,#36256,#36257,#36258),.UNSPECIFIED.,.F.,.F.,(4,3,3,
3,3,3,3,4),(333.451881951072,333.78561661106,334.784974744626,335.784332878192,
336.783691011758,337.783049145324,338.78240727889,339.735067258252),
 .UNSPECIFIED.);
#738=B_SPLINE_CURVE_WITH_KNOTS('',3,(#36263,#36264,#36265,#36266,#36267,
#36268,#36269,#36270,#36271,#36272,#36273,#36274,#36275,#36276,#36277,#36278,
#36279,#36280,#36281,#36282,#36283,#36284,#36285,#36286,#36287,#36288,#36289,
#36290,#36291,#36292,#36293,#36294,#36295,#36296),.UNSPECIFIED.,.F.,.F.,
(4,3,3,3,3,3,3,3,3,3,3,4),(-349.273907386581,-348.77598861455,-348.276309547767,
-347.776630480984,-347.276951414201,-346.777272347418,-346.277593280635,
-345.777914213852,-345.278235147069,-344.778556080286,-343.77919794672,
-342.990722079402),.UNSPECIFIED.);
#739=B_SPLINE_CURVE_WITH_KNOTS('',3,(#36297,#36298,#36299,#36300,#36301,
#36302,#36303,#36304,#36305,#36306,#36307,#36308,#36309,#36310,#36311,#36312,
#36313,#36314,#36315,#36316,#36317,#36318,#36319,#36320,#36321,#36322,#36323,
#36324),.UNSPECIFIED.,.F.,.F.,(4,3,3,3,3,3,3,3,3,4),(339.735067258252,339.781765412456,
340.781123546022,341.780481679588,342.779839813154,343.77919794672,344.778556080286,
345.278235147069,345.777914213852,346.018252565431),.UNSPECIFIED.);
#740=B_SPLINE_CURVE_WITH_KNOTS('',3,(#36329,#36330,#36331,#36332,#36333,
#36334,#36335,#36336,#36337,#36338,#36339,#36340,#36341,#36342,#36343,#36344,
#36345,#36346,#36347,#36348,#36349,#36350,#36351,#36352,#36353,#36354,#36355,
#36356,#36357,#36358,#36359,#36360,#36361,#36362,#36363,#36364,#36365,#36366,
#36367,#36368,#36369,#36370,#36371),.UNSPECIFIED.,.F.,.F.,(4,3,3,3,3,3,
3,3,3,3,3,3,3,3,4),(-355.557092693761,-355.27181648273,-354.772137415947,
-354.272458349164,-353.77277928238,-353.273100215597,-352.773421148814,
-352.273742082031,-351.774063015248,-351.274383948465,-350.774704881682,
-350.275025814899,-349.775346748116,-349.275667681333,-349.273907386581),
 .UNSPECIFIED.);
#741=B_SPLINE_CURVE_WITH_KNOTS('',3,(#36372,#36373,#36374,#36375,#36376,
#36377,#36378,#36379,#36380,#36381,#36382,#36383,#36384,#36385,#36386,#36387,
#36388,#36389,#36390,#36391,#36392,#36393,#36394,#36395,#36396,#36397,#36398,
#36399,#36400,#36401,#36402,#36403,#36404,#36405,#36406,#36407,#36408,#36409,
#36410,#36411,#36412,#36413,#36414),.UNSPECIFIED.,.F.,.F.,(4,3,3,3,3,3,
3,3,3,3,3,3,3,3,4),(346.018252565431,346.277593280635,346.777272347418,
347.276951414201,347.776630480984,348.276309547767,348.77598861455,349.275667681334,
349.775346748116,350.2750258149,350.774704881683,351.274383948466,351.774063015249,
352.273742082032,352.301437872611),.UNSPECIFIED.);
#742=B_SPLINE_CURVE_WITH_KNOTS('',3,(#36419,#36420,#36421,#36422,#36423,
#36424,#36425,#36426,#36427,#36428,#36429,#36430,#36431,#36432,#36433,#36434,
#36435,#36436,#36437,#36438,#36439,#36440,#36441,#36442,#36443,#36444,#36445,
#36446,#36447,#36448,#36449,#36450,#36451,#36452,#36453,#36454,#36455,#36456,
#36457,#36458,#36459,#36460,#36461),.UNSPECIFIED.,.F.,.F.,(4,3,3,3,3,3,
3,3,3,3,3,3,3,3,4),(-361.84027800094,-361.767644350909,-361.267965284126,
-360.768286217343,-360.26860715056,-359.768928083777,-359.269249016994,
-358.769569950211,-358.269890883428,-357.770211816645,-357.270532749862,
-356.770853683079,-356.271174616296,-355.771495549513,-355.557092693761),
 .UNSPECIFIED.);
#743=B_SPLINE_CURVE_WITH_KNOTS('',3,(#36462,#36463,#36464,#36465,#36466,
#36467,#36468,#36469,#36470,#36471,#36472,#36473,#36474,#36475,#36476,#36477,
#36478,#36479,#36480,#36481,#36482,#36483,#36484,#36485,#36486,#36487,#36488,
#36489,#36490,#36491,#36492,#36493,#36494,#36495,#36496,#36497,#36498,#36499,
#36500,#36501),.UNSPECIFIED.,.F.,.F.,(4,3,3,3,3,3,3,3,3,3,3,3,3,4),(352.301437872611,
352.773421148815,353.273100215598,353.772779282381,354.272458349164,354.772137415947,
355.27181648273,355.771495549513,356.271174616296,356.770853683079,357.270532749862,
357.770211816645,358.269890883428,358.58462317979),.UNSPECIFIED.);
#744=B_SPLINE_CURVE_WITH_KNOTS('',3,(#36506,#36507,#36508,#36509,#36510,
#36511,#36512,#36513,#36514,#36515,#36516,#36517,#36518,#36519,#36520,#36521,
#36522,#36523,#36524,#36525,#36526,#36527,#36528,#36529,#36530,#36531,#36532,
#36533,#36534,#36535,#36536,#36537,#36538,#36539,#36540,#36541,#36542,#36543,
#36544,#36545),.UNSPECIFIED.,.F.,.F.,(4,3,3,3,3,3,3,3,3,3,3,3,3,4),(-368.12346330812,
-367.763793152305,-367.264114085522,-366.764435018739,-366.264755951956,
-365.765076885173,-365.26539781839,-364.765718751607,-364.266039684824,
-363.766360618041,-363.266681551258,-362.767002484475,-362.267323417692,
-361.84027800094),.UNSPECIFIED.);
#745=B_SPLINE_CURVE_WITH_KNOTS('',3,(#36546,#36547,#36548,#36549,#36550,
#36551,#36552,#36553,#36554,#36555,#36556,#36557,#36558,#36559,#36560,#36561,
#36562,#36563,#36564,#36565,#36566,#36567,#36568,#36569,#36570,#36571,#36572,
#36573,#36574,#36575,#36576,#36577,#36578,#36579,#36580,#36581,#36582,#36583,
#36584,#36585,#36586,#36587,#36588),.UNSPECIFIED.,.F.,.F.,(4,3,3,3,3,3,
3,3,3,3,3,3,3,3,4),(358.58462317979,358.769569950211,359.269249016994,359.768928083777,
360.26860715056,360.768286217343,361.267965284126,361.767644350909,362.267323417692,
362.767002484475,363.266681551258,363.766360618041,364.266039684824,364.765718751607,
364.86780848697),.UNSPECIFIED.);
#746=B_SPLINE_CURVE_WITH_KNOTS('',3,(#36593,#36594,#36595,#36596,#36597,
#36598,#36599,#36600,#36601,#36602,#36603,#36604,#36605,#36606,#36607,#36608,
#36609,#36610,#36611,#36612,#36613,#36614,#36615,#36616,#36617,#36618,#36619,
#36620,#36621,#36622,#36623,#36624,#36625,#36626,#36627,#36628,#36629,#36630,
#36631,#36632,#36633,#36634,#36635),.UNSPECIFIED.,.F.,.F.,(4,3,3,3,3,3,
3,3,3,3,3,3,3,3,4),(-374.406648615299,-374.259621020484,-373.759941953701,
-373.260262886918,-372.760583820135,-372.260904753352,-371.761225686569,
-371.261546619786,-370.761867553003,-370.26218848622,-369.762509419437,
-369.262830352654,-368.763151285871,-368.263472219088,-368.12346330812),
 .UNSPECIFIED.);
#747=B_SPLINE_CURVE_WITH_KNOTS('',3,(#36636,#36637,#36638,#36639,#36640,
#36641,#36642,#36643,#36644,#36645,#36646,#36647,#36648,#36649,#36650,#36651,
#36652,#36653,#36654,#36655,#36656,#36657,#36658,#36659,#36660,#36661,#36662,
#36663,#36664,#36665,#36666,#36667,#36668,#36669,#36670,#36671,#36672,#36673,
#36674,#36675),.UNSPECIFIED.,.F.,.F.,(4,3,3,3,3,3,3,3,3,3,3,3,3,4),(364.86780848697,
365.26539781839,365.765076885173,366.264755951956,366.764435018739,367.264114085522,
367.763793152305,368.263472219088,368.763151285871,369.262830352654,369.762509419437,
370.26218848622,370.761867553004,371.150993794149),.UNSPECIFIED.);
#748=B_SPLINE_CURVE_WITH_KNOTS('',3,(#36680,#36681,#36682,#36683,#36684,
#36685,#36686,#36687,#36688,#36689,#36690,#36691,#36692,#36693,#36694,#36695,
#36696,#36697,#36698,#36699,#36700,#36701,#36702,#36703,#36704,#36705,#36706,
#36707,#36708,#36709,#36710,#36711,#36712,#36713,#36714,#36715,#36716,#36717,
#36718,#36719),.UNSPECIFIED.,.F.,.F.,(4,3,3,3,3,3,3,3,3,3,3,3,3,4),(-380.689833922479,
-380.255769821881,-379.756090755098,-379.256411688315,-378.756732621532,
-378.257053554749,-377.757374487966,-377.257695421183,-376.7580163544,-376.258337287616,
-375.758658220834,-375.25897915405,-374.759300087267,-374.406648615299),
 .UNSPECIFIED.);
#749=B_SPLINE_CURVE_WITH_KNOTS('',3,(#36720,#36721,#36722,#36723,#36724,
#36725,#36726,#36727,#36728,#36729,#36730,#36731,#36732,#36733,#36734,#36735,
#36736,#36737,#36738,#36739,#36740,#36741,#36742,#36743,#36744,#36745,#36746,
#36747,#36748,#36749,#36750,#36751,#36752,#36753,#36754,#36755,#36756,#36757,
#36758,#36759,#36760,#36761,#36762),.UNSPECIFIED.,.F.,.F.,(4,3,3,3,3,3,
3,3,3,3,3,3,3,3,4),(371.150993794149,371.261546619787,371.76122568657,372.260904753353,
372.760583820136,373.260262886919,373.759941953702,374.259621020485,374.759300087268,
375.258979154051,375.758658220834,376.258337287617,376.7580163544,377.257695421183,
377.434179101329),.UNSPECIFIED.);
#750=B_SPLINE_CURVE_WITH_KNOTS('',3,(#36767,#36768,#36769,#36770,#36771,
#36772,#36773,#36774,#36775,#36776,#36777,#36778,#36779,#36780,#36781,#36782,
#36783,#36784,#36785,#36786,#36787,#36788,#36789,#36790,#36791,#36792,#36793,
#36794,#36795,#36796,#36797,#36798,#36799,#36800,#36801,#36802,#36803,#36804,
#36805,#36806,#36807,#36808,#36809),.UNSPECIFIED.,.F.,.F.,(4,3,3,3,3,3,
3,3,3,3,3,3,3,3,4),(-386.973019229658,-386.75159769006,-386.251918623277,
-385.752239556494,-385.252560489711,-384.752881422928,-384.253202356145,
-383.753523289362,-383.253844222579,-382.754165155796,-382.254486089013,
-381.75480702223,-381.255127955447,-380.755448888664,-380.689833922479),
 .UNSPECIFIED.);
#751=B_SPLINE_CURVE_WITH_KNOTS('',3,(#36810,#36811,#36812,#36813,#36814,
#36815,#36816,#36817,#36818,#36819,#36820,#36821,#36822,#36823,#36824,#36825,
#36826,#36827,#36828,#36829,#36830,#36831,#36832,#36833,#36834,#36835,#36836,
#36837,#36838,#36839,#36840,#36841,#36842,#36843,#36844,#36845,#36846,#36847,
#36848,#36849),.UNSPECIFIED.,.F.,.F.,(4,3,3,3,3,3,3,3,3,3,3,3,3,4),(377.434179101329,
377.757374487966,378.257053554749,378.756732621532,379.256411688315,379.756090755098,
380.255769821881,380.755448888664,381.255127955447,381.75480702223,382.254486089013,
382.754165155796,383.253844222579,383.717364408508),.UNSPECIFIED.);
#752=B_SPLINE_CURVE_WITH_KNOTS('',3,(#36854,#36855,#36856,#36857,#36858,
#36859,#36860,#36861,#36862,#36863,#36864,#36865,#36866,#36867,#36868,#36869,
#36870,#36871,#36872,#36873,#36874,#36875,#36876,#36877,#36878,#36879,#36880,
#36881,#36882,#36883,#36884,#36885,#36886,#36887,#36888,#36889,#36890,#36891,
#36892,#36893,#36894,#36895,#36896),.UNSPECIFIED.,.F.,.F.,(4,3,3,3,3,3,
3,3,3,3,3,3,3,3,4),(-393.256204536838,-393.247425558239,-392.747746491456,
-392.248067424673,-391.74838835789,-391.248709291107,-390.749030224324,
-390.249351157541,-389.749672090758,-389.249993023975,-388.750313957192,
-388.250634890409,-387.750955823626,-387.251276756843,-386.973019229658),
 .UNSPECIFIED.);
#753=B_SPLINE_CURVE_WITH_KNOTS('',3,(#36897,#36898,#36899,#36900,#36901,
#36902,#36903,#36904,#36905,#36906,#36907,#36908,#36909,#36910,#36911,#36912,
#36913,#36914,#36915,#36916,#36917,#36918,#36919,#36920,#36921,#36922,#36923,
#36924,#36925,#36926,#36927,#36928,#36929,#36930,#36931,#36932,#36933,#36934,
#36935,#36936,#36937,#36938,#36939),.UNSPECIFIED.,.F.,.F.,(4,3,3,3,3,3,
3,3,3,3,3,3,3,3,4),(383.717364408508,383.753523289362,384.253202356145,
384.752881422928,385.252560489711,385.752239556494,386.251918623277,386.75159769006,
387.251276756843,387.750955823626,388.250634890409,388.750313957192,389.249993023975,
389.749672090758,390.000549715688),.UNSPECIFIED.);
#754=B_SPLINE_CURVE_WITH_KNOTS('',3,(#36945,#36946,#36947,#36948),
 .UNSPECIFIED.,.F.,.F.,(4,4),(405.265452313083,405.755527026166),
 .UNSPECIFIED.);
#755=B_SPLINE_CURVE_WITH_KNOTS('',3,(#36954,#36955,#36956,#36957,#36958,
#36959,#36960,#36961,#36962,#36963,#36964,#36965,#36966,#36967,#36968,#36969,
#36970),.UNSPECIFIED.,.F.,.F.,(4,1,1,1,1,1,1,1,1,1,1,1,1,1,4),(398.982267005903,
399.260524533088,399.760203599871,400.259882666654,400.759561733437,401.25924080022,
401.758919867003,402.258598933787,402.75827800057,403.257957067353,403.757636134136,
404.257315200919,404.756994267702,405.256673334485,405.265452313083),
 .UNSPECIFIED.);
#756=B_SPLINE_CURVE_WITH_KNOTS('',3,(#36973,#36974,#36975,#36976,#36977,
#36978,#36979,#36980,#36981,#36982,#36983,#36984,#36985),.UNSPECIFIED.,
 .F.,.F.,(4,1,1,1,1,1,1,1,1,1,4),(398.982267005904,399.231068447758,399.730747514541,
400.230426581324,400.730105648107,401.22978471489,401.729463781673,402.229142848456,
402.728821915239,403.228500982022,403.728180048805),.UNSPECIFIED.);
#757=B_SPLINE_CURVE_WITH_KNOTS('',3,(#36990,#36991,#36992,#36993,#36994,
#36995,#36996,#36997,#36998,#36999,#37000,#37001,#37002,#37003,#37004,#37005,
#37006),.UNSPECIFIED.,.F.,.F.,(4,1,1,1,1,1,1,1,1,1,1,1,1,1,4),(392.699081698724,
392.764696664909,393.264375731692,393.764054798475,394.263733865258,394.763412932041,
395.263091998824,395.762771065607,396.26245013239,396.762129199173,397.261808265956,
397.761487332739,398.261166399522,398.760845466305,398.982267005903),
 .UNSPECIFIED.);
#758=B_SPLINE_CURVE_WITH_KNOTS('',3,(#37007,#37008,#37009,#37010,#37011,
#37012,#37013,#37014,#37015,#37016,#37017,#37018,#37019,#37020,#37021,#37022,
#37023),.UNSPECIFIED.,.F.,.F.,(4,1,1,1,1,1,1,1,1,1,1,1,1,1,4),(392.699081698724,
392.735240579579,393.234919646362,393.734598713145,394.234277779928,394.733956846711,
395.233635913494,395.733314980277,396.23299404706,396.732673113843,397.232352180626,
397.732031247409,398.231710314192,398.731389380975,398.982267005904),
 .UNSPECIFIED.);
#759=B_SPLINE_CURVE_WITH_KNOTS('',3,(#37028,#37029,#37030,#37031,#37032,
#37033,#37034,#37035,#37036,#37037,#37038,#37039,#37040,#37041,#37042,#37043),
 .UNSPECIFIED.,.F.,.F.,(4,1,1,1,1,1,1,1,1,1,1,1,1,4),(386.415896391544,
386.768547863513,387.268226930296,387.767905997079,388.267585063862,388.767264130645,
389.266943197428,389.766622264211,390.266301330994,390.765980397777,391.26565946456,
391.765338531343,392.265017598126,392.699081698724),.UNSPECIFIED.);
#760=B_SPLINE_CURVE_WITH_KNOTS('',3,(#37044,#37045,#37046,#37047,#37048,
#37049,#37050,#37051,#37052,#37053,#37054,#37055,#37056,#37057,#37058,#37059),
 .UNSPECIFIED.,.F.,.F.,(4,1,1,1,1,1,1,1,1,1,1,1,1,4),(386.415896391545,
386.739091778183,387.238770844966,387.738449911749,388.238128978532,388.737808045315,
389.237487112098,389.737166178881,390.236845245664,390.736524312447,391.23620337923,
391.735882446013,392.235561512796,392.699081698724),.UNSPECIFIED.);
#761=B_SPLINE_CURVE_WITH_KNOTS('',3,(#37064,#37065,#37066,#37067,#37068,
#37069,#37070,#37071,#37072,#37073,#37074,#37075,#37076,#37077,#37078,#37079,
#37080),.UNSPECIFIED.,.F.,.F.,(4,1,1,1,1,1,1,1,1,1,1,1,1,1,4),(380.132711084365,
380.272719995333,380.772399062117,381.2720781289,381.771757195683,382.271436262466,
382.771115329249,383.270794396032,383.770473462815,384.270152529598,384.769831596381,
385.269510663164,385.769189729947,386.26886879673,386.415896391544),
 .UNSPECIFIED.);
#762=B_SPLINE_CURVE_WITH_KNOTS('',3,(#37081,#37082,#37083,#37084,#37085,
#37086,#37087,#37088,#37089,#37090,#37091,#37092,#37093,#37094,#37095,#37096,
#37097),.UNSPECIFIED.,.F.,.F.,(4,1,1,1,1,1,1,1,1,1,1,1,1,1,4),(380.132711084365,
380.243263910003,380.742942976786,381.242622043569,381.742301110352,382.241980177135,
382.741659243918,383.241338310702,383.741017377485,384.240696444268,384.740375511051,
385.240054577834,385.739733644617,386.2394127114,386.415896391545),
 .UNSPECIFIED.);
#763=B_SPLINE_CURVE_WITH_KNOTS('',3,(#37102,#37103,#37104,#37105,#37106,
#37107,#37108,#37109,#37110,#37111,#37112,#37113,#37114,#37115,#37116,#37117),
 .UNSPECIFIED.,.F.,.F.,(4,1,1,1,1,1,1,1,1,1,1,1,1,4),(373.849525777185,
374.276571193937,374.77625026072,375.275929327503,375.775608394286,376.275287461069,
376.774966527852,377.274645594635,377.774324661418,378.274003728201,378.773682794984,
379.273361861767,379.77304092855,380.132711084365),.UNSPECIFIED.);
#764=B_SPLINE_CURVE_WITH_KNOTS('',3,(#37118,#37119,#37120,#37121,#37122,
#37123,#37124,#37125,#37126,#37127,#37128,#37129,#37130,#37131,#37132,#37133),
 .UNSPECIFIED.,.F.,.F.,(4,1,1,1,1,1,1,1,1,1,1,1,1,4),(373.849525777185,
374.247115108607,374.74679417539,375.246473242173,375.746152308956,376.245831375739,
376.745510442522,377.245189509305,377.744868576088,378.244547642871,378.744226709654,
379.243905776437,379.74358484322,380.132711084365),.UNSPECIFIED.);
#765=B_SPLINE_CURVE_WITH_KNOTS('',3,(#37138,#37139,#37140,#37141,#37142,
#37143,#37144,#37145,#37146,#37147,#37148,#37149,#37150,#37151,#37152,#37153,
#37154),.UNSPECIFIED.,.F.,.F.,(4,1,1,1,1,1,1,1,1,1,1,1,1,1,4),(367.566340470006,
367.780743325758,368.280422392541,368.780101459324,369.279780526107,369.77945959289,
370.279138659673,370.778817726456,371.278496793239,371.778175860022,372.277854926805,
372.777533993588,373.277213060371,373.776892127154,373.849525777185),
 .UNSPECIFIED.);
#766=B_SPLINE_CURVE_WITH_KNOTS('',3,(#37155,#37156,#37157,#37158,#37159,
#37160,#37161,#37162,#37163,#37164,#37165,#37166,#37167,#37168,#37169,#37170,
#37171),.UNSPECIFIED.,.F.,.F.,(4,1,1,1,1,1,1,1,1,1,1,1,1,1,4),(367.566340470006,
367.751287240428,368.250966307211,368.750645373994,369.250324440777,369.75000350756,
370.249682574343,370.749361641126,371.249040707909,371.748719774692,372.248398841475,
372.748077908258,373.247756975041,373.747436041824,373.849525777185),
 .UNSPECIFIED.);
#767=B_SPLINE_CURVE_WITH_KNOTS('',3,(#37176,#37177,#37178,#37179,#37180,
#37181,#37182,#37183,#37184,#37185,#37186,#37187,#37188,#37189,#37190,#37191,
#37192),.UNSPECIFIED.,.F.,.F.,(4,1,1,1,1,1,1,1,1,1,1,1,1,1,4),(361.283155162826,
361.284915457579,361.784594524362,362.284273591145,362.783952657928,363.283631724711,
363.783310791494,364.282989858277,364.78266892506,365.282347991843,365.782027058626,
366.281706125409,366.781385192192,367.281064258975,367.566340470006),
 .UNSPECIFIED.);
#768=B_SPLINE_CURVE_WITH_KNOTS('',3,(#37193,#37194,#37195,#37196,#37197,
#37198,#37199,#37200,#37201,#37202,#37203,#37204,#37205,#37206,#37207,#37208),
 .UNSPECIFIED.,.F.,.F.,(4,1,1,1,1,1,1,1,1,1,1,1,1,4),(361.283155162826,
361.755138439031,362.254817505815,362.754496572598,363.254175639381,363.753854706164,
364.253533772947,364.75321283973,365.252891906513,365.752570973296,366.252250040079,
366.751929106862,367.251608173645,367.566340470006),.UNSPECIFIED.);
#769=B_SPLINE_CURVE_WITH_KNOTS('',3,(#37213,#37214,#37215,#37216,#37217,
#37218,#37219,#37220,#37221,#37222,#37223,#37224,#37225,#37226),
 .UNSPECIFIED.,.F.,.F.,(4,1,1,1,1,1,1,1,1,1,1,4),(354.999969855646,355.788445722965,
356.787803856531,357.287482923314,357.787161990097,358.28684105688,358.786520123663,
359.286199190446,359.78587825723,360.285557324013,360.785236390796,361.283155162826),
 .UNSPECIFIED.);
#770=B_SPLINE_CURVE_WITH_KNOTS('',3,(#37227,#37228,#37229,#37230,#37231,
#37232,#37233,#37234,#37235,#37236,#37237,#37238,#37239,#37240,#37241,#37242,
#37243),.UNSPECIFIED.,.F.,.F.,(4,1,1,1,1,1,1,1,1,1,1,1,1,1,4),(354.999969855647,
355.259310570852,355.758989637635,356.258668704418,356.758347771201,357.258026837984,
357.757705904767,358.25738497155,358.757064038333,359.256743105116,359.756422171899,
360.256101238682,360.755780305465,361.255459372248,361.283155162826),
 .UNSPECIFIED.);
#771=B_SPLINE_CURVE_WITH_KNOTS('',3,(#37248,#37249,#37250,#37251,#37252,
#37253,#37254,#37255,#37256,#37257,#37258),.UNSPECIFIED.,.F.,.F.,(4,1,1,
1,1,1,1,1,4),(348.716784548467,348.792938788003,349.792296921569,350.791655055135,
351.791013188701,352.790371322267,353.789729455833,354.789087589399,354.999969855646),
 .UNSPECIFIED.);
#772=B_SPLINE_CURVE_WITH_KNOTS('',3,(#37259,#37260,#37261,#37262,#37263,
#37264,#37265,#37266,#37267,#37268,#37269,#37270),.UNSPECIFIED.,.F.,.F.,
(4,1,1,1,1,1,1,1,1,4),(348.716784548467,348.763482702673,349.762840836239,
350.762198969805,351.761557103371,352.760915236937,353.760273370503,354.259952437286,
354.759631504069,354.999969855647),.UNSPECIFIED.);
#773=B_SPLINE_CURVE_WITH_KNOTS('',3,(#37275,#37276,#37277,#37278,#37279,
#37280,#37281,#37282,#37283,#37284),.UNSPECIFIED.,.F.,.F.,(4,1,1,1,1,1,
1,4),(342.433599241287,342.796789986607,343.796148120173,344.795506253739,
345.794864387305,346.794222520871,347.793580654437,348.716784548467),
 .UNSPECIFIED.);
#774=B_SPLINE_CURVE_WITH_KNOTS('',3,(#37285,#37286,#37287,#37288,#37289,
#37290,#37291,#37292,#37293,#37294),.UNSPECIFIED.,.F.,.F.,(4,1,1,1,1,1,
1,4),(342.433599241288,342.767333901277,343.766692034843,344.766050168409,
345.765408301975,346.764766435541,347.764124569107,348.716784548467),
 .UNSPECIFIED.);
#775=B_SPLINE_CURVE_WITH_KNOTS('',3,(#37299,#37300,#37301,#37302,#37303,
#37304,#37305,#37306,#37307,#37308),.UNSPECIFIED.,.F.,.F.,(4,1,1,1,1,1,
1,4),(336.150413934108,336.80064118521,337.799999318776,338.799357452343,
339.798715585909,340.798073719475,341.797431853041,342.433599241287),
 .UNSPECIFIED.);
#776=B_SPLINE_CURVE_WITH_KNOTS('',3,(#37309,#37310,#37311,#37312,#37313,
#37314,#37315,#37316,#37317,#37318),.UNSPECIFIED.,.F.,.F.,(4,1,1,1,1,1,
1,4),(336.150413934108,336.77118509988,337.770543233446,338.769901367012,
339.769259500578,340.768617634145,341.767975767711,342.433599241288),
 .UNSPECIFIED.);
#777=B_SPLINE_CURVE_WITH_KNOTS('',3,(#37323,#37324,#37325,#37326,#37327,
#37328,#37329,#37330,#37331,#37332),.UNSPECIFIED.,.F.,.F.,(4,1,1,1,1,1,
1,4),(329.867228626928,330.804492383814,331.80385051738,332.803208650946,
333.802566784512,334.801924918078,335.801283051644,336.150413934108),
 .UNSPECIFIED.);
#778=B_SPLINE_CURVE_WITH_KNOTS('',3,(#37333,#37334,#37335,#37336,#37337,
#37338,#37339,#37340,#37341,#37342),.UNSPECIFIED.,.F.,.F.,(4,1,1,1,1,1,
1,4),(329.867228626928,330.775036298484,331.77439443205,332.773752565616,
333.773110699182,334.772468832748,335.771826966314,336.150413934108),
 .UNSPECIFIED.);
#779=B_SPLINE_CURVE_WITH_KNOTS('',3,(#37347,#37348,#37349,#37350,#37351,
#37352,#37353,#37354,#37355,#37356,#37357),.UNSPECIFIED.,.F.,.F.,(4,1,1,
1,1,1,1,1,4),(323.584043319749,323.808985448852,324.808343582418,325.807701715984,
326.80705984955,327.806417983116,328.805776116682,329.805134250248,329.867228626928),
 .UNSPECIFIED.);
#780=B_SPLINE_CURVE_WITH_KNOTS('',3,(#37358,#37359,#37360,#37361,#37362,
#37363,#37364,#37365,#37366,#37367,#37368),.UNSPECIFIED.,.F.,.F.,(4,1,1,
1,1,1,1,1,4),(323.584043319749,323.779529363522,324.778887497088,325.778245630654,
326.77760376422,327.776961897786,328.776320031352,329.775678164918,329.867228626928),
 .UNSPECIFIED.);
#781=B_SPLINE_CURVE_WITH_KNOTS('',3,(#37373,#37374,#37375,#37376,#37377,
#37378,#37379,#37380,#37381,#37382),.UNSPECIFIED.,.F.,.F.,(4,1,1,1,1,1,
1,4),(317.300858012569,317.812836647456,318.812194781022,319.811552914588,
320.810911048154,321.81026918172,322.809627315286,323.584043319749),
 .UNSPECIFIED.);
#782=B_SPLINE_CURVE_WITH_KNOTS('',3,(#37383,#37384,#37385,#37386,#37387,
#37388,#37389,#37390,#37391,#37392),.UNSPECIFIED.,.F.,.F.,(4,1,1,1,1,1,
1,4),(317.300858012569,317.783380562125,318.782738695691,319.782096829258,
320.781454962824,321.78081309639,322.780171229956,323.584043319749),
 .UNSPECIFIED.);
#783=B_SPLINE_CURVE_WITH_KNOTS('',3,(#37397,#37398,#37399,#37400,#37401,
#37402,#37403,#37404,#37405,#37406),.UNSPECIFIED.,.F.,.F.,(4,1,1,1,1,1,
1,4),(311.017672705389,311.816687846059,312.816045979625,313.815404113191,
314.814762246757,315.814120380323,316.81347851389,317.300858012569),
 .UNSPECIFIED.);
#784=B_SPLINE_CURVE_WITH_KNOTS('',3,(#37407,#37408,#37409,#37410,#37411,
#37412,#37413,#37414,#37415,#37416),.UNSPECIFIED.,.F.,.F.,(4,1,1,1,1,1,
1,4),(311.01767270539,311.787231760729,312.786589894295,313.785948027861,
314.785306161427,315.784664294993,316.784022428559,317.300858012569),
 .UNSPECIFIED.);
#785=B_SPLINE_CURVE_WITH_KNOTS('',3,(#37421,#37422,#37423,#37424,#37425,
#37426,#37427,#37428,#37429,#37430,#37431),.UNSPECIFIED.,.F.,.F.,(4,1,1,
1,1,1,1,1,4),(304.73448739821,304.821180911097,305.820539044663,306.819897178229,
307.819255311795,308.818613445361,309.817971578927,310.817329712493,311.017672705389),
 .UNSPECIFIED.);
#786=B_SPLINE_CURVE_WITH_KNOTS('',3,(#37432,#37433,#37434,#37435,#37436,
#37437,#37438,#37439,#37440,#37441,#37442),.UNSPECIFIED.,.F.,.F.,(4,1,1,
1,1,1,1,1,4),(304.73448739821,304.791724825767,305.791082959333,306.790441092899,
307.789799226465,308.789157360031,309.788515493597,310.787873627163,311.01767270539),
 .UNSPECIFIED.);
#787=B_SPLINE_CURVE_WITH_KNOTS('',3,(#37447,#37448,#37449,#37450,#37451,
#37452,#37453,#37454,#37455,#37456),.UNSPECIFIED.,.F.,.F.,(4,1,1,1,1,1,
1,4),(298.45130209103,298.825032109701,299.824390243267,300.823748376833,
301.823106510399,302.822464643965,303.821822777531,304.73448739821),
 .UNSPECIFIED.);
#788=B_SPLINE_CURVE_WITH_KNOTS('',3,(#37457,#37458,#37459,#37460,#37461,
#37462,#37463,#37464,#37465,#37466),.UNSPECIFIED.,.F.,.F.,(4,1,1,1,1,1,
1,4),(298.451302091031,298.795576024371,299.794934157937,300.794292291503,
301.793650425069,302.793008558635,303.792366692201,304.73448739821),
 .UNSPECIFIED.);
#789=B_SPLINE_CURVE_WITH_KNOTS('',3,(#37471,#37472,#37473,#37474,#37475,
#37476,#37477,#37478,#37479,#37480),.UNSPECIFIED.,.F.,.F.,(4,1,1,1,1,1,
1,4),(292.168116783851,292.828883308304,293.82824144187,294.827599575437,
295.826957709003,296.826315842569,297.825673976135,298.45130209103),
 .UNSPECIFIED.);
#790=B_SPLINE_CURVE_WITH_KNOTS('',3,(#37481,#37482,#37483,#37484,#37485,
#37486,#37487,#37488,#37489,#37490),.UNSPECIFIED.,.F.,.F.,(4,1,1,1,1,1,
1,4),(292.168116783851,292.799427222974,293.79878535654,294.798143490106,
295.797501623672,296.796859757238,297.796217890804,298.451302091031),
 .UNSPECIFIED.);
#791=B_SPLINE_CURVE_WITH_KNOTS('',3,(#37495,#37496,#37497,#37498,#37499,
#37500,#37501,#37502,#37503,#37504),.UNSPECIFIED.,.F.,.F.,(4,1,1,1,1,1,
1,4),(285.884931476671,286.832734506908,287.832092640474,288.83145077404,
289.830808907606,290.830167041172,291.829525174738,292.168116783851),
 .UNSPECIFIED.);
#792=B_SPLINE_CURVE_WITH_KNOTS('',3,(#37505,#37506,#37507,#37508,#37509,
#37510,#37511,#37512,#37513,#37514),.UNSPECIFIED.,.F.,.F.,(4,1,1,1,1,1,
1,4),(285.884931476672,286.803278421578,287.802636555144,288.80199468871,
289.801352822276,290.800710955842,291.800069089408,292.168116783851),
 .UNSPECIFIED.);
#793=B_SPLINE_CURVE_WITH_KNOTS('',3,(#37519,#37520,#37521,#37522,#37523,
#37524,#37525,#37526,#37527,#37528,#37529),.UNSPECIFIED.,.F.,.F.,(4,1,1,
1,1,1,1,1,4),(279.601746169492,279.837227571946,280.836585705512,281.835943839078,
282.835301972644,283.83466010621,284.834018239776,285.833376373342,285.884931476671),
 .UNSPECIFIED.);
#794=B_SPLINE_CURVE_WITH_KNOTS('',3,(#37530,#37531,#37532,#37533,#37534,
#37535,#37536,#37537,#37538,#37539,#37540),.UNSPECIFIED.,.F.,.F.,(4,1,1,
1,1,1,1,1,4),(279.601746169492,279.807771486616,280.807129620182,281.806487753748,
282.805845887314,283.80520402088,284.804562154446,285.803920288012,285.884931476672),
 .UNSPECIFIED.);
#795=B_SPLINE_CURVE_WITH_KNOTS('',3,(#37545,#37546,#37547,#37548,#37549,
#37550,#37551,#37552,#37553,#37554),.UNSPECIFIED.,.F.,.F.,(4,1,1,1,1,1,
1,4),(273.318560862312,273.84107877055,274.840436904116,275.839795037682,
276.839153171248,277.838511304814,278.83786943838,279.601746169492),
 .UNSPECIFIED.);
#796=B_SPLINE_CURVE_WITH_KNOTS('',3,(#37555,#37556,#37557,#37558,#37559,
#37560,#37561,#37562,#37563,#37564),.UNSPECIFIED.,.F.,.F.,(4,1,1,1,1,1,
1,4),(273.318560862312,273.811622685219,274.810980818785,275.810338952351,
276.809697085917,277.809055219484,278.80841335305,279.601746169492),
 .UNSPECIFIED.);
#797=B_SPLINE_CURVE_WITH_KNOTS('',3,(#37569,#37570,#37571,#37572,#37573,
#37574,#37575,#37576,#37577,#37578),.UNSPECIFIED.,.F.,.F.,(4,1,1,1,1,1,
1,4),(267.035375555133,267.844929969153,268.844288102719,269.843646236285,
270.843004369851,271.842362503417,272.841720636983,273.318560862312),
 .UNSPECIFIED.);
#798=B_SPLINE_CURVE_WITH_KNOTS('',3,(#37579,#37580,#37581,#37582,#37583,
#37584,#37585,#37586,#37587,#37588),.UNSPECIFIED.,.F.,.F.,(4,1,1,1,1,1,
1,4),(267.035375555133,267.815473883823,268.814832017389,269.814190150955,
270.813548284521,271.812906418087,272.812264551653,273.318560862312),
 .UNSPECIFIED.);
#799=B_SPLINE_CURVE_WITH_KNOTS('',3,(#37593,#37594,#37595,#37596,#37597,
#37598,#37599,#37600,#37601,#37602,#37603),.UNSPECIFIED.,.F.,.F.,(4,1,1,
1,1,1,1,1,4),(260.752190247953,260.849423034191,261.848781167757,262.848139301323,
263.847497434889,264.846855568455,265.846213702021,266.845571835587,267.035375555133),
 .UNSPECIFIED.);
#800=B_SPLINE_CURVE_WITH_KNOTS('',3,(#37604,#37605,#37606,#37607,#37608,
#37609,#37610,#37611,#37612,#37613,#37614),.UNSPECIFIED.,.F.,.F.,(4,1,1,
1,1,1,1,1,4),(260.752190247953,260.819966948861,261.819325082427,262.818683215993,
263.818041349559,264.817399483125,265.816757616691,266.816115750257,267.035375555133),
 .UNSPECIFIED.);
#801=B_SPLINE_CURVE_WITH_KNOTS('',3,(#37619,#37620,#37621,#37622,#37623,
#37624,#37625,#37626,#37627,#37628),.UNSPECIFIED.,.F.,.F.,(4,1,1,1,1,1,
1,4),(254.469004940773,254.853274232795,255.852632366361,256.851990499927,
257.851348633493,258.850706767059,259.850064900625,260.752190247953),
 .UNSPECIFIED.);
#802=B_SPLINE_CURVE_WITH_KNOTS('',3,(#37629,#37630,#37631,#37632,#37633,
#37634,#37635,#37636,#37637,#37638),.UNSPECIFIED.,.F.,.F.,(4,1,1,1,1,1,
1,4),(254.469004940774,254.823818147464,255.82317628103,256.822534414597,
257.821892548163,258.821250681729,259.820608815295,260.752190247953),
 .UNSPECIFIED.);
#803=B_SPLINE_CURVE_WITH_KNOTS('',3,(#37643,#37644,#37645,#37646,#37647,
#37648,#37649,#37650,#37651,#37652),.UNSPECIFIED.,.F.,.F.,(4,1,1,1,1,1,
1,4),(248.185819633594,248.857125431398,249.856483564964,250.85584169853,
251.855199832097,252.854557965663,253.853916099229,254.469004940773),
 .UNSPECIFIED.);
#804=B_SPLINE_CURVE_WITH_KNOTS('',3,(#37653,#37654,#37655,#37656,#37657,
#37658,#37659,#37660,#37661,#37662),.UNSPECIFIED.,.F.,.F.,(4,1,1,1,1,1,
1,4),(248.185819633594,248.827669346068,249.827027479634,250.8263856132,
251.825743746766,252.825101880332,253.824460013898,254.469004940774),
 .UNSPECIFIED.);
#805=B_SPLINE_CURVE_WITH_KNOTS('',3,(#37667,#37668,#37669,#37670,#37671,
#37672,#37673,#37674,#37675,#37676),.UNSPECIFIED.,.F.,.F.,(4,1,1,1,1,1,
1,4),(241.902634326414,242.860976630002,243.860334763568,244.859692897134,
245.8590510307,246.858409164266,247.857767297832,248.185819633594),
 .UNSPECIFIED.);
#806=B_SPLINE_CURVE_WITH_KNOTS('',3,(#37677,#37678,#37679,#37680,#37681,
#37682,#37683,#37684,#37685,#37686),.UNSPECIFIED.,.F.,.F.,(4,1,1,1,1,1,
1,4),(241.902634326415,242.831520544672,243.830878678238,244.830236811804,
245.82959494537,246.828953078936,247.828311212502,248.185819633594),
 .UNSPECIFIED.);
#807=B_SPLINE_CURVE_WITH_KNOTS('',3,(#37691,#37692,#37693,#37694,#37695,
#37696,#37697,#37698,#37699,#37700,#37701),.UNSPECIFIED.,.F.,.F.,(4,1,1,
1,1,1,1,1,4),(235.619449019235,235.86546969504,236.864827828606,237.864185962172,
238.863544095738,239.862902229304,240.86226036287,241.861618496436,241.902634326414),
 .UNSPECIFIED.);
#808=B_SPLINE_CURVE_WITH_KNOTS('',3,(#37702,#37703,#37704,#37705,#37706,
#37707,#37708,#37709,#37710,#37711,#37712),.UNSPECIFIED.,.F.,.F.,(4,1,1,
1,1,1,1,1,4),(235.619449019235,235.83601360971,236.835371743276,237.834729876842,
238.834088010408,239.833446143974,240.83280427754,241.832162411106,241.902634326415),
 .UNSPECIFIED.);
#809=B_SPLINE_CURVE_WITH_KNOTS('',3,(#37717,#37718,#37719,#37720,#37721,
#37722,#37723,#37724,#37725,#37726),.UNSPECIFIED.,.F.,.F.,(4,1,1,1,1,1,
1,4),(229.336263712055,229.869320893643,230.86867902721,231.868037160776,
232.867395294342,233.866753427908,234.866111561474,235.619449019235),
 .UNSPECIFIED.);
#810=B_SPLINE_CURVE_WITH_KNOTS('',3,(#37727,#37728,#37729,#37730,#37731,
#37732,#37733,#37734,#37735,#37736),.UNSPECIFIED.,.F.,.F.,(4,1,1,1,1,1,
1,4),(229.336263712055,229.839864808313,230.839222941879,231.838581075445,
232.837939209011,233.837297342577,234.836655476144,235.619449019235),
 .UNSPECIFIED.);
#811=B_SPLINE_CURVE_WITH_KNOTS('',3,(#37741,#37742,#37743,#37744,#37745,
#37746,#37747,#37748,#37749,#37750),.UNSPECIFIED.,.F.,.F.,(4,1,1,1,1,1,
1,4),(223.053078404876,223.873172092247,224.872530225813,225.871888359379,
226.871246492945,227.870604626511,228.869962760077,229.336263712055),
 .UNSPECIFIED.);
#812=B_SPLINE_CURVE_WITH_KNOTS('',3,(#37751,#37752,#37753,#37754,#37755,
#37756,#37757,#37758,#37759,#37760),.UNSPECIFIED.,.F.,.F.,(4,1,1,1,1,1,
1,4),(223.053078404876,223.843716006917,224.843074140483,225.842432274049,
226.841790407615,227.841148541181,228.840506674747,229.336263712055),
 .UNSPECIFIED.);
#813=B_SPLINE_CURVE_WITH_KNOTS('',3,(#37765,#37766,#37767,#37768,#37769,
#37770,#37771,#37772,#37773,#37774,#37775),.UNSPECIFIED.,.F.,.F.,(4,1,1,
1,1,1,1,1,4),(216.769893097696,216.877665157285,217.877023290851,218.876381424417,
219.875739557983,220.875097691549,221.874455825115,222.873813958681,223.053078404876),
 .UNSPECIFIED.);
#814=B_SPLINE_CURVE_WITH_KNOTS('',3,(#37776,#37777,#37778,#37779,#37780,
#37781,#37782,#37783,#37784,#37785,#37786),.UNSPECIFIED.,.F.,.F.,(4,1,1,
1,1,1,1,1,4),(216.769893097696,216.848209071955,217.847567205521,218.846925339087,
219.846283472653,220.845641606219,221.844999739785,222.844357873351,223.053078404876),
 .UNSPECIFIED.);
#815=B_SPLINE_CURVE_WITH_KNOTS('',3,(#37791,#37792,#37793,#37794,#37795,
#37796,#37797,#37798,#37799,#37800),.UNSPECIFIED.,.F.,.F.,(4,1,1,1,1,1,
1,4),(210.486707790516,210.881516355889,211.880874489455,212.880232623021,
213.879590756587,214.878948890153,215.878307023719,216.769893097696),
 .UNSPECIFIED.);
#816=B_SPLINE_CURVE_WITH_KNOTS('',3,(#37801,#37802,#37803,#37804,#37805,
#37806,#37807,#37808,#37809,#37810),.UNSPECIFIED.,.F.,.F.,(4,1,1,1,1,1,
1,4),(210.486707790517,210.852060270558,211.851418404124,212.85077653769,
213.850134671257,214.849492804823,215.848850938389,216.769893097696),
 .UNSPECIFIED.);
#817=B_SPLINE_CURVE_WITH_KNOTS('',3,(#37815,#37816,#37817,#37818,#37819,
#37820,#37821,#37822,#37823,#37824),.UNSPECIFIED.,.F.,.F.,(4,1,1,1,1,1,
1,4),(204.203522483337,204.885367554492,205.884725688058,206.884083821624,
207.88344195519,208.882800088756,209.882158222323,210.486707790516),
 .UNSPECIFIED.);
#818=B_SPLINE_CURVE_WITH_KNOTS('',3,(#37825,#37826,#37827,#37828,#37829,
#37830,#37831,#37832,#37833,#37834),.UNSPECIFIED.,.F.,.F.,(4,1,1,1,1,1,
1,4),(204.203522483337,204.855911469162,205.855269602728,206.854627736294,
207.85398586986,208.853344003426,209.852702136992,210.486707790517),
 .UNSPECIFIED.);
#819=B_SPLINE_CURVE_WITH_KNOTS('',3,(#37839,#37840,#37841,#37842,#37843,
#37844,#37845,#37846,#37847,#37848),.UNSPECIFIED.,.F.,.F.,(4,1,1,1,1,1,
1,4),(197.920337176157,198.889218753096,199.888576886662,200.887935020228,
201.887293153794,202.88665128736,203.886009420926,204.203522483337),
 .UNSPECIFIED.);
#820=B_SPLINE_CURVE_WITH_KNOTS('',3,(#37849,#37850,#37851,#37852,#37853,
#37854,#37855,#37856,#37857,#37858),.UNSPECIFIED.,.F.,.F.,(4,1,1,1,1,1,
1,4),(197.920337176158,198.859762667766,199.859120801332,200.858478934898,
201.857837068464,202.85719520203,203.856553335596,204.203522483337),
 .UNSPECIFIED.);
#821=B_SPLINE_CURVE_WITH_KNOTS('',3,(#37863,#37864,#37865,#37866,#37867,
#37868,#37869,#37870,#37871,#37872,#37873),.UNSPECIFIED.,.F.,.F.,(4,1,1,
1,1,1,1,1,4),(191.637151868978,191.893711818134,192.8930699517,193.892428085266,
194.891786218832,195.891144352398,196.890502485964,197.88986061953,197.920337176157),
 .UNSPECIFIED.);
#822=B_SPLINE_CURVE_WITH_KNOTS('',3,(#37874,#37875,#37876,#37877,#37878,
#37879,#37880,#37881,#37882,#37883,#37884),.UNSPECIFIED.,.F.,.F.,(4,1,1,
1,1,1,1,1,4),(191.637151868978,191.864255732803,192.86361386637,193.862971999936,
194.862330133502,195.861688267068,196.861046400634,197.8604045342,197.920337176158),
 .UNSPECIFIED.);
#823=B_SPLINE_CURVE_WITH_KNOTS('',3,(#37889,#37890,#37891,#37892,#37893,
#37894,#37895,#37896,#37897,#37898),.UNSPECIFIED.,.F.,.F.,(4,1,1,1,1,1,
1,4),(185.353966561798,185.897563016737,186.896921150303,187.89627928387,
188.895637417436,189.894995551002,190.894353684568,191.637151868978),
 .UNSPECIFIED.);
#824=B_SPLINE_CURVE_WITH_KNOTS('',3,(#37899,#37900,#37901,#37902,#37903,
#37904,#37905,#37906,#37907,#37908),.UNSPECIFIED.,.F.,.F.,(4,1,1,1,1,1,
1,4),(185.353966561799,185.868106931407,186.867465064973,187.866823198539,
188.866181332105,189.865539465671,190.864897599237,191.637151868978),
 .UNSPECIFIED.);
#825=B_SPLINE_CURVE_WITH_KNOTS('',3,(#37913,#37914,#37915,#37916,#37917,
#37918,#37919,#37920,#37921,#37922),.UNSPECIFIED.,.F.,.F.,(4,1,1,1,1,1,
1,4),(179.070781254619,179.901414215341,180.900772348907,181.900130482473,
182.899488616039,183.898846749605,184.898204883171,185.353966561798),
 .UNSPECIFIED.);
#826=B_SPLINE_CURVE_WITH_KNOTS('',3,(#37923,#37924,#37925,#37926,#37927,
#37928,#37929,#37930,#37931,#37932),.UNSPECIFIED.,.F.,.F.,(4,1,1,1,1,1,
1,4),(179.070781254619,179.871958130011,180.871316263577,181.870674397143,
182.870032530709,183.869390664275,184.868748797841,185.353966561799),
 .UNSPECIFIED.);
#827=B_SPLINE_CURVE_WITH_KNOTS('',3,(#37937,#37938,#37939,#37940,#37941,
#37942,#37943,#37944,#37945,#37946,#37947),.UNSPECIFIED.,.F.,.F.,(4,1,1,
1,1,1,1,1,4),(172.787595947439,172.905907280379,173.905265413945,174.904623547511,
175.903981681077,176.903339814643,177.902697948209,178.902056081775,179.070781254619),
 .UNSPECIFIED.);
#828=B_SPLINE_CURVE_WITH_KNOTS('',3,(#37948,#37949,#37950,#37951,#37952,
#37953,#37954,#37955,#37956,#37957,#37958),.UNSPECIFIED.,.F.,.F.,(4,1,1,
1,1,1,1,1,4),(172.787595947439,172.876451195049,173.875809328615,174.875167462181,
175.874525595747,176.873883729313,177.873241862879,178.872599996445,179.070781254619),
 .UNSPECIFIED.);
#829=B_SPLINE_CURVE_WITH_KNOTS('',3,(#37963,#37964,#37965,#37966,#37967,
#37968,#37969,#37970,#37971,#37972),.UNSPECIFIED.,.F.,.F.,(4,1,1,1,1,1,
1,4),(166.504410640259,166.909758478983,167.909116612549,168.908474746115,
169.907832879681,170.907191013247,171.906549146813,172.787595947439),
 .UNSPECIFIED.);
#830=B_SPLINE_CURVE_WITH_KNOTS('',3,(#37973,#37974,#37975,#37976,#37977,
#37978,#37979,#37980,#37981,#37982),.UNSPECIFIED.,.F.,.F.,(4,1,1,1,1,1,
1,4),(166.50441064026,166.880302393652,167.879660527218,168.879018660784,
169.87837679435,170.877734927916,171.877093061483,172.787595947439),
 .UNSPECIFIED.);
#831=B_SPLINE_CURVE_WITH_KNOTS('',3,(#37987,#37988,#37989,#37990,#37991,
#37992,#37993,#37994,#37995,#37996),.UNSPECIFIED.,.F.,.F.,(4,1,1,1,1,1,
1,4),(160.22122533308,160.913609677586,161.912967811152,162.912325944718,
163.911684078284,164.91104221185,165.910400345416,166.504410640259),
 .UNSPECIFIED.);
#832=B_SPLINE_CURVE_WITH_KNOTS('',3,(#37997,#37998,#37999,#38000,#38001,
#38002,#38003,#38004,#38005,#38006),.UNSPECIFIED.,.F.,.F.,(4,1,1,1,1,1,
1,4),(160.22122533308,160.884153592256,161.883511725822,162.882869859388,
163.882227992954,164.88158612652,165.880944260086,166.50441064026),
 .UNSPECIFIED.);
#833=B_SPLINE_CURVE_WITH_KNOTS('',3,(#38011,#38012,#38013,#38014,#38015,
#38016,#38017,#38018,#38019,#38020),.UNSPECIFIED.,.F.,.F.,(4,1,1,1,1,1,
1,4),(153.9380400259,154.91746087619,155.916819009756,156.916177143322,
157.915535276888,158.914893410454,159.91425154402,160.22122533308),
 .UNSPECIFIED.);
#834=B_SPLINE_CURVE_WITH_KNOTS('',3,(#38021,#38022,#38023,#38024,#38025,
#38026,#38027,#38028,#38029,#38030),.UNSPECIFIED.,.F.,.F.,(4,1,1,1,1,1,
1,4),(153.938040025901,154.88800479086,155.887362924426,156.886721057992,
157.886079191558,158.885437325124,159.88479545869,160.22122533308),
 .UNSPECIFIED.);
#835=B_SPLINE_CURVE_WITH_KNOTS('',3,(#38035,#38036,#38037,#38038,#38039,
#38040,#38041,#38042,#38043,#38044,#38045),.UNSPECIFIED.,.F.,.F.,(4,1,1,
1,1,1,1,1,4),(147.654854718721,147.921953941228,148.921312074794,149.92067020836,
150.920028341926,151.919386475492,152.918744609058,153.918102742624,153.9380400259),
 .UNSPECIFIED.);
#836=B_SPLINE_CURVE_WITH_KNOTS('',3,(#38046,#38047,#38048,#38049,#38050,
#38051,#38052,#38053,#38054,#38055,#38056),.UNSPECIFIED.,.F.,.F.,(4,1,1,
1,1,1,1,1,4),(147.654854718721,147.892497855897,148.891855989463,149.891214123029,
150.890572256596,151.889930390162,152.889288523728,153.888646657294,153.938040025901),
 .UNSPECIFIED.);
#837=B_SPLINE_CURVE_WITH_KNOTS('',3,(#38061,#38062,#38063,#38064,#38065,
#38066,#38067,#38068,#38069,#38070),.UNSPECIFIED.,.F.,.F.,(4,1,1,1,1,1,
1,4),(141.371669411541,141.925805139831,142.925163273397,143.924521406963,
144.92387954053,145.923237674096,146.922595807662,147.654854718721),
 .UNSPECIFIED.);
#838=B_SPLINE_CURVE_WITH_KNOTS('',3,(#38071,#38072,#38073,#38074,#38075,
#38076,#38077,#38078,#38079,#38080),.UNSPECIFIED.,.F.,.F.,(4,1,1,1,1,1,
1,4),(141.371669411542,141.896349054501,142.895707188067,143.895065321633,
144.894423455199,145.893781588765,146.893139722331,147.654854718721),
 .UNSPECIFIED.);
#839=B_SPLINE_CURVE_WITH_KNOTS('',3,(#38085,#38086,#38087,#38088,#38089,
#38090,#38091,#38092,#38093,#38094),.UNSPECIFIED.,.F.,.F.,(4,1,1,1,1,1,
1,4),(135.088484104362,135.929656338435,136.929014472001,137.928372605567,
138.927730739133,139.927088872699,140.926447006265,141.371669411541),
 .UNSPECIFIED.);
#840=B_SPLINE_CURVE_WITH_KNOTS('',3,(#38095,#38096,#38097,#38098,#38099,
#38100,#38101,#38102,#38103,#38104),.UNSPECIFIED.,.F.,.F.,(4,1,1,1,1,1,
1,4),(135.088484104362,135.900200253105,136.899558386671,137.898916520237,
138.898274653803,139.897632787369,140.896990920935,141.371669411542),
 .UNSPECIFIED.);
#841=B_SPLINE_CURVE_WITH_KNOTS('',3,(#38109,#38110,#38111,#38112,#38113,
#38114,#38115,#38116,#38117,#38118,#38119),.UNSPECIFIED.,.F.,.F.,(4,1,1,
1,1,1,1,1,4),(128.805298797182,128.934149403473,129.933507537039,130.932865670605,
131.932223804171,132.931581937737,133.930940071303,134.930298204869,135.088484104362),
 .UNSPECIFIED.);
#842=B_SPLINE_CURVE_WITH_KNOTS('',3,(#38120,#38121,#38122,#38123,#38124,
#38125,#38126,#38127,#38128,#38129,#38130),.UNSPECIFIED.,.F.,.F.,(4,1,1,
1,1,1,1,1,4),(128.805298797182,128.904693318142,129.904051451709,130.903409585275,
131.902767718841,132.902125852407,133.901483985973,134.900842119539,135.088484104362),
 .UNSPECIFIED.);
#843=B_SPLINE_CURVE_WITH_KNOTS('',3,(#38135,#38136,#38137,#38138,#38139,
#38140,#38141,#38142,#38143,#38144),.UNSPECIFIED.,.F.,.F.,(4,1,1,1,1,1,
1,4),(122.522113490002,122.938000602077,123.937358735643,124.936716869209,
125.936075002775,126.935433136341,127.934791269907,128.805298797182),
 .UNSPECIFIED.);
#844=B_SPLINE_CURVE_WITH_KNOTS('',3,(#38145,#38146,#38147,#38148,#38149,
#38150,#38151,#38152,#38153,#38154),.UNSPECIFIED.,.F.,.F.,(4,1,1,1,1,1,
1,4),(122.522113490003,122.908544516746,123.907902650312,124.907260783878,
125.906618917444,126.90597705101,127.905335184576,128.805298797182),
 .UNSPECIFIED.);
#845=B_SPLINE_CURVE_WITH_KNOTS('',3,(#38159,#38160,#38161,#38162,#38163,
#38164,#38165,#38166,#38167,#38168),.UNSPECIFIED.,.F.,.F.,(4,1,1,1,1,1,
1,4),(116.238928182823,116.94185180068,117.941209934246,118.940568067812,
119.939926201378,120.939284334944,121.93864246851,122.522113490002),
 .UNSPECIFIED.);
#846=B_SPLINE_CURVE_WITH_KNOTS('',3,(#38169,#38170,#38171,#38172,#38173,
#38174,#38175,#38176,#38177,#38178),.UNSPECIFIED.,.F.,.F.,(4,1,1,1,1,1,
1,4),(116.238928182823,116.91239571535,117.911753848916,118.911111982482,
119.910470116048,120.909828249614,121.90918638318,122.522113490003),
 .UNSPECIFIED.);
#847=B_SPLINE_CURVE_WITH_KNOTS('',3,(#38183,#38184,#38185,#38186,#38187,
#38188,#38189,#38190,#38191,#38192),.UNSPECIFIED.,.F.,.F.,(4,1,1,1,1,1,
1,4),(109.955742875643,110.945702999284,111.94506113285,112.944419266416,
113.943777399982,114.943135533548,115.942493667114,116.238928182823),
 .UNSPECIFIED.);
#848=B_SPLINE_CURVE_WITH_KNOTS('',3,(#38193,#38194,#38195,#38196,#38197,
#38198,#38199,#38200,#38201,#38202),.UNSPECIFIED.,.F.,.F.,(4,1,1,1,1,1,
1,4),(109.955742875644,110.916246913954,111.91560504752,112.914963181086,
113.914321314652,114.913679448218,115.913037581784,116.238928182823),
 .UNSPECIFIED.);
#849=B_SPLINE_CURVE_WITH_KNOTS('',3,(#38207,#38208,#38209,#38210,#38211,
#38212,#38213,#38214,#38215,#38216,#38217),.UNSPECIFIED.,.F.,.F.,(4,1,1,
1,1,1,1,1,4),(103.672557568464,103.950196064322,104.949554197888,105.948912331454,
106.94827046502,107.947628598586,108.946986732152,109.946344865718,109.955742875643),
 .UNSPECIFIED.);
#850=B_SPLINE_CURVE_WITH_KNOTS('',3,(#38218,#38219,#38220,#38221,#38222,
#38223,#38224,#38225,#38226,#38227,#38228),.UNSPECIFIED.,.F.,.F.,(4,1,1,
1,1,1,1,1,4),(103.672557568464,103.920739978991,104.920098112557,105.919456246123,
106.918814379689,107.918172513255,108.917530646822,109.916888780388,109.955742875644),
 .UNSPECIFIED.);
#851=B_SPLINE_CURVE_WITH_KNOTS('',3,(#38233,#38234,#38235,#38236,#38237,
#38238,#38239,#38240,#38241,#38242),.UNSPECIFIED.,.F.,.F.,(4,1,1,1,1,1,
1,4),(97.3893722612841,97.9540472629253,98.9534053964914,99.9527635300574,
100.952121663623,101.95147979719,102.950837930756,103.672557568464),
 .UNSPECIFIED.);
#852=B_SPLINE_CURVE_WITH_KNOTS('',3,(#38243,#38244,#38245,#38246,#38247,
#38248,#38249,#38250,#38251,#38252),.UNSPECIFIED.,.F.,.F.,(4,1,1,1,1,1,
1,4),(97.3893722612845,97.924591177595,98.9239493111611,99.9233074447271,
100.922665578293,101.922023711859,102.921381845425,103.672557568464),
 .UNSPECIFIED.);
#853=B_SPLINE_CURVE_WITH_KNOTS('',3,(#38257,#38258,#38259,#38260,#38261,
#38262,#38263,#38264,#38265,#38266),.UNSPECIFIED.,.F.,.F.,(4,1,1,1,1,1,
1,4),(91.1061869541045,91.9578984615291,92.9572565950951,93.9566147286612,
94.9559728622272,95.9553309957932,96.9546891293593,97.3893722612841),
 .UNSPECIFIED.);
#854=B_SPLINE_CURVE_WITH_KNOTS('',3,(#38267,#38268,#38269,#38270,#38271,
#38272,#38273,#38274,#38275,#38276),.UNSPECIFIED.,.F.,.F.,(4,1,1,1,1,1,
1,4),(91.1061869541048,91.9284423761987,92.9278005097648,93.9271586433308,
94.9265167768969,95.9258749104629,96.925233044029,97.3893722612845),
 .UNSPECIFIED.);
#855=B_SPLINE_CURVE_WITH_KNOTS('',3,(#38281,#38282,#38283,#38284,#38285,
#38286,#38287,#38288,#38289,#38290,#38291),.UNSPECIFIED.,.F.,.F.,(4,1,1,
1,1,1,1,1,4),(84.8230016469249,84.9623915265667,85.9617496601328,86.9611077936988,
87.9604659272649,88.9598240608309,89.959182194397,90.958540327963,91.1061869541045),
 .UNSPECIFIED.);
#856=B_SPLINE_CURVE_WITH_KNOTS('',3,(#38292,#38293,#38294,#38295,#38296,
#38297,#38298,#38299,#38300,#38301,#38302),.UNSPECIFIED.,.F.,.F.,(4,1,1,
1,1,1,1,1,4),(84.8230016469253,84.9329354412364,85.9322935748025,86.9316517083685,
87.9310098419346,88.9303679755006,89.9297261090666,90.9290842426327,91.1061869541048),
 .UNSPECIFIED.);
#857=B_SPLINE_CURVE_WITH_KNOTS('',3,(#38307,#38308,#38309,#38310,#38311,
#38312,#38313,#38314,#38315,#38316),.UNSPECIFIED.,.F.,.F.,(4,1,1,1,1,1,
1,4),(78.5398163397454,78.9662427251705,79.9656008587365,80.9649589923026,
81.9643171258686,82.9636752594347,83.9630333930007,84.8230016469249),
 .UNSPECIFIED.);
#858=B_SPLINE_CURVE_WITH_KNOTS('',3,(#38317,#38318,#38319,#38320,#38321,
#38322,#38323,#38324,#38325,#38326),.UNSPECIFIED.,.F.,.F.,(4,1,1,1,1,1,
1,4),(78.5398163397457,78.9367866398401,79.9361447734062,80.9355029069722,
81.9348610405383,82.9342191741043,83.9335773076704,84.8230016469253),
 .UNSPECIFIED.);
#859=B_SPLINE_CURVE_WITH_KNOTS('',3,(#38331,#38332,#38333,#38334,#38335,
#38336,#38337,#38338,#38339,#38340),.UNSPECIFIED.,.F.,.F.,(4,1,1,1,1,1,
1,4),(72.2566310325658,72.9700939237742,73.9694520573402,74.9688101909063,
75.9681683244723,76.9675264580384,77.9668845916044,78.5398163397454),
 .UNSPECIFIED.);
#860=B_SPLINE_CURVE_WITH_KNOTS('',3,(#38341,#38342,#38343,#38344,#38345,
#38346,#38347,#38348,#38349,#38350),.UNSPECIFIED.,.F.,.F.,(4,1,1,1,1,1,
1,4),(72.2566310325661,72.9406378384438,73.9399959720099,74.9393541055759,
75.938712239142,76.938070372708,77.9374285062741,78.5398163397457),
 .UNSPECIFIED.);
#861=B_SPLINE_CURVE_WITH_KNOTS('',3,(#38355,#38356,#38357,#38358,#38359,
#38360,#38361,#38362,#38363,#38364,#38365),.UNSPECIFIED.,.F.,.F.,(4,1,1,
1,1,1,1,1,4),(65.9734457253862,65.9745869888119,66.9739451223779,67.9733032559439,
68.97266138951,69.972019523076,70.9713776566421,71.9707357902081,72.2566310325658),
 .UNSPECIFIED.);
#862=B_SPLINE_CURVE_WITH_KNOTS('',3,(#38366,#38367,#38368,#38369,#38370,
#38371,#38372,#38373,#38374,#38375),.UNSPECIFIED.,.F.,.F.,(4,1,1,1,1,1,
1,4),(65.9734457253865,66.9444890370476,67.9438471706136,68.9432053041797,
69.9425634377457,70.9419215713118,71.9412797048778,72.2566310325661),
 .UNSPECIFIED.);
#863=B_SPLINE_CURVE_WITH_KNOTS('',3,(#38380,#38381,#38382,#38383,#38384,
#38385,#38386,#38387,#38388,#38389,#38390,#38391),.UNSPECIFIED.,.F.,.F.,
(4,1,1,1,1,1,1,1,1,4),(59.6902604182066,59.9784381874156,60.4781172541986,
60.9777963209816,61.4774753877646,61.9771544545477,62.9765125881137,63.9758707216798,
64.9752288552458,65.9734457253862),.UNSPECIFIED.);
#864=B_SPLINE_CURVE_WITH_KNOTS('',3,(#38392,#38393,#38394,#38395,#38396,
#38397,#38398,#38399,#38400,#38401,#38402),.UNSPECIFIED.,.F.,.F.,(4,1,1,
1,1,1,1,1,4),(59.6902604182069,59.9489821020852,60.9483402356513,61.9476983692173,
62.9470565027834,63.9464146363494,64.9457727699155,65.9451309034815,65.9734457253865),
 .UNSPECIFIED.);
#865=B_SPLINE_CURVE_WITH_KNOTS('',3,(#38407,#38408,#38409,#38410,#38411,
#38412,#38413,#38414,#38415,#38416,#38417,#38418,#38419,#38420,#38421,#38422,
#38423),.UNSPECIFIED.,.F.,.F.,(4,1,1,1,1,1,1,1,1,1,1,1,1,1,4),(53.407075111027,
53.4826103192363,53.9822893860193,54.4819684528023,54.9816475195853,55.4813265863684,
55.9810056531514,56.4806847199344,56.9803637867174,57.4800428535005,57.9797219202835,
58.4794009870665,58.9790800538495,59.4787591206325,59.6902604182066),
 .UNSPECIFIED.);
#866=B_SPLINE_CURVE_WITH_KNOTS('',3,(#38424,#38425,#38426,#38427,#38428,
#38429,#38430,#38431,#38432,#38433,#38434,#38435,#38436,#38437,#38438,#38439),
 .UNSPECIFIED.,.F.,.F.,(4,1,1,1,1,1,1,1,1,1,1,1,1,4),(53.4070751110273,
53.4531542339059,53.9528333006889,54.452512367472,54.952191434255,55.451870501038,
55.951549567821,56.4512286346041,56.9509077013871,57.4505867681701,57.9502658349531,
58.4499449017362,58.9496239685192,59.6902604182069),.UNSPECIFIED.);
#867=B_SPLINE_CURVE_WITH_KNOTS('',3,(#38444,#38445,#38446,#38447,#38448,
#38449,#38450,#38451,#38452,#38453,#38454,#38455,#38456,#38457,#38458,#38459),
 .UNSPECIFIED.,.F.,.F.,(4,1,1,1,1,1,1,1,1,1,1,1,1,4),(47.1238898038474,
47.48646151784,47.986140584623,48.485819651406,48.9854987181891,49.4851777849721,
49.9848568517551,50.4845359185381,50.9842149853212,51.4838940521042,51.9835731188872,
52.4832521856702,52.9829312524532,53.407075111027),.UNSPECIFIED.);
#868=B_SPLINE_CURVE_WITH_KNOTS('',3,(#38460,#38461,#38462,#38463,#38464,
#38465,#38466,#38467,#38468,#38469,#38470,#38471,#38472,#38473,#38474,#38475),
 .UNSPECIFIED.,.F.,.F.,(4,1,1,1,1,1,1,1,1,1,1,1,1,4),(47.1238898038477,
47.4570054325096,47.9566844992927,48.4563635660757,48.9560426328587,49.4557216996417,
49.9554007664248,50.4550798332078,50.9547588999908,51.4544379667738,51.9541170335568,
52.4537961003399,52.9534751671229,53.4070751110273),.UNSPECIFIED.);
#869=B_SPLINE_CURVE_WITH_KNOTS('',3,(#38480,#38481,#38482,#38483,#38484,
#38485,#38486,#38487,#38488,#38489,#38490,#38491,#38492,#38493,#38494,#38495,
#38496),.UNSPECIFIED.,.F.,.F.,(4,1,1,1,1,1,1,1,1,1,1,1,1,1,4),(40.8407044966678,
40.9906336496607,41.4903127164437,41.9899917832267,42.4896708500098,42.9893499167928,
43.4890289835758,43.9887080503588,44.4883871171419,44.9880661839249,45.4877452507079,
45.9874243174909,46.4871033842739,46.986782451057,47.1238898038474),
 .UNSPECIFIED.);
#870=B_SPLINE_CURVE_WITH_KNOTS('',3,(#38497,#38498,#38499,#38500,#38501,
#38502,#38503,#38504,#38505,#38506,#38507,#38508,#38509,#38510,#38511,#38512,
#38513),.UNSPECIFIED.,.F.,.F.,(4,1,1,1,1,1,1,1,1,1,1,1,1,1,4),(40.8407044966681,
40.9611775643303,41.4608566311134,41.9605356978964,42.4602147646794,42.9598938314624,
43.4595728982454,43.9592519650285,44.4589310318115,44.9586100985945,45.4582891653775,
45.9579682321606,46.4576472989436,46.9573263657266,47.1238898038477),
 .UNSPECIFIED.);
#871=B_SPLINE_CURVE_WITH_KNOTS('',3,(#38518,#38519,#38520,#38521,#38522,
#38523,#38524,#38525,#38526,#38527,#38528,#38529,#38530,#38531,#38532,#38533),
 .UNSPECIFIED.,.F.,.F.,(4,1,1,1,1,1,1,1,1,1,1,1,1,4),(34.5575191894882,
34.9944848482644,35.4941639150474,35.9938429818305,36.4935220486135,36.9932011153965,
37.4928801821795,37.9925592489626,38.4922383157456,38.9919173825286,39.4915964493116,
39.9912755160946,40.4909545828777,40.8407044966678),.UNSPECIFIED.);
#872=B_SPLINE_CURVE_WITH_KNOTS('',3,(#38534,#38535,#38536,#38537,#38538,
#38539,#38540,#38541,#38542,#38543,#38544,#38545,#38546,#38547,#38548,#38549),
 .UNSPECIFIED.,.F.,.F.,(4,1,1,1,1,1,1,1,1,1,1,1,1,4),(34.5575191894886,
34.965028762934,35.4647078297171,35.9643868965001,36.4640659632831,36.9637450300661,
37.4634240968492,37.9631031636322,38.4627822304152,38.9624612971982,39.4621403639813,
39.9618194307643,40.4614984975473,40.8407044966681),.UNSPECIFIED.);
#873=B_SPLINE_CURVE_WITH_KNOTS('',3,(#38554,#38555,#38556,#38557,#38558,
#38559,#38560,#38561,#38562,#38563,#38564,#38565,#38566,#38567,#38568,#38569,
#38570),.UNSPECIFIED.,.F.,.F.,(4,1,1,1,1,1,1,1,1,1,1,1,1,1,4),(28.2743338823086,
28.4986569800851,28.9983360468681,29.4980151136512,29.9976941804342,30.4973732472172,
30.9970523140002,31.4967313807832,31.9964104475663,32.4960895143493,32.9957685811323,
33.4954476479153,33.9951267146984,34.4948057814814,34.5575191894882),
 .UNSPECIFIED.);
#874=B_SPLINE_CURVE_WITH_KNOTS('',3,(#38571,#38572,#38573,#38574,#38575,
#38576,#38577,#38578,#38579,#38580,#38581,#38582,#38583,#38584,#38585,#38586,
#38587),.UNSPECIFIED.,.F.,.F.,(4,1,1,1,1,1,1,1,1,1,1,1,1,1,4),(28.2743338823089,
28.4692008947547,28.9688799615378,29.4685590283208,29.9682380951038,30.4679171618868,
30.9675962286699,31.4672752954529,31.9669543622359,32.4666334290189,32.966312495802,
33.465991562585,33.965670629368,34.465349696151,34.5575191894886),
 .UNSPECIFIED.);
#875=B_SPLINE_CURVE_WITH_KNOTS('',3,(#38592,#38593,#38594,#38595,#38596,
#38597,#38598,#38599,#38600,#38601,#38602,#38603,#38604,#38605,#38606,#38607,
#38608),.UNSPECIFIED.,.F.,.F.,(4,1,1,1,1,1,1,1,1,1,1,1,1,1,4),(21.991148575129,
22.0028291119058,22.5025081786888,23.0021872454719,23.5018663122549,24.0015453790379,
24.5012244458209,25.0009035126039,25.500582579387,26.00026164617,26.499940712953,
26.999619779736,27.4992988465191,27.9989779133021,28.2743338823086),
 .UNSPECIFIED.);
#876=B_SPLINE_CURVE_WITH_KNOTS('',3,(#38609,#38610,#38611,#38612,#38613,
#38614,#38615,#38616,#38617,#38618,#38619,#38620,#38621,#38622,#38623,#38624),
 .UNSPECIFIED.,.F.,.F.,(4,1,1,1,1,1,1,1,1,1,1,1,1,4),(21.9911485751294,
22.4730520933585,22.9727311601415,23.4724102269245,23.9720892937075,24.4717683604905,
24.9714474272736,25.4711264940566,25.9708055608396,26.4704846276226,26.9701636944057,
27.4698427611887,27.9695218279717,28.2743338823089),.UNSPECIFIED.);
#877=B_SPLINE_CURVE_WITH_KNOTS('',3,(#38629,#38630,#38631,#38632,#38633,
#38634,#38635,#38636,#38637,#38638,#38639,#38640,#38641,#38642,#38643,#38644),
 .UNSPECIFIED.,.F.,.F.,(4,1,1,1,1,1,1,1,1,1,1,1,1,4),(15.7079632679495,
16.0066803105095,16.5063593772925,17.0060384440756,17.5057175108586,18.0053965776416,
18.5050756444246,19.0047547112077,19.5044337779907,20.0041128447737,20.5037919115567,
21.0034709783398,21.5031500451228,21.991148575129),.UNSPECIFIED.);
#878=B_SPLINE_CURVE_WITH_KNOTS('',3,(#38645,#38646,#38647,#38648,#38649,
#38650,#38651,#38652,#38653,#38654,#38655,#38656,#38657,#38658,#38659,#38660,
#38661),.UNSPECIFIED.,.F.,.F.,(4,1,1,1,1,1,1,1,1,1,1,1,1,1,4),(15.7079632679498,
15.9772242251791,16.4769032919622,16.9765823587452,17.4762614255282,17.9759404923112,
18.4756195590943,18.9752986258773,19.4749776926603,19.9746567594433,20.4743358262264,
20.9740148930094,21.4736939597924,21.9733730265754,21.9911485751294),
 .UNSPECIFIED.);
#879=B_SPLINE_CURVE_WITH_KNOTS('',3,(#38666,#38667,#38668,#38669,#38670,
#38671,#38672,#38673,#38674,#38675,#38676,#38677,#38678,#38679,#38680,#38681,
#38682,#38683,#38684,#38685,#38686,#38687,#38688,#38689,#38690,#38691,#38692,
#38693,#38694,#38695,#38696,#38697,#38698,#38699,#38700,#38701,#38702),
 .UNSPECIFIED.,.F.,.F.,(4,3,3,3,3,3,3,3,3,3,3,3,4),(0.,0.000373494560508806,
0.0620760815771024,0.112839239637108,0.153038169722591,0.175804963675793,
0.247183842626883,0.319084136954533,0.344742425233931,0.363606980156396,
0.439518700737557,0.51795432283266,0.534785019937482),.UNSPECIFIED.);
#880=B_SPLINE_CURVE_WITH_KNOTS('',3,(#38704,#38705,#38706,#38707,#38708,
#38709,#38710,#38711,#38712,#38713,#38714,#38715,#38716,#38717,#38718,#38719,
#38720,#38721,#38722,#38723,#38724,#38725,#38726,#38727,#38728,#38729,#38730,
#38731,#38732,#38733,#38734,#38735,#38736,#38737,#38738,#38739,#38740),
 .UNSPECIFIED.,.F.,.F.,(4,3,3,3,3,3,3,3,3,3,3,3,4),(0.,0.000511892384038064,
0.078754853834616,0.155070466132989,0.20164291816609,0.227017770490094,
0.290460834304131,0.352619921814331,0.383703668213755,0.403796492255862,
0.466621120797767,0.52704524650008,0.539097184344933),.UNSPECIFIED.);
#881=B_SPLINE_CURVE_WITH_KNOTS('',3,(#40740,#40741,#40742,#40743,#40744,
#40745,#40746,#40747,#40748,#40749,#40750,#40751,#40752,#40753,#40754,#40755,
#40756,#40757,#40758,#40759,#40760,#40761,#40762,#40763,#40764,#40765,#40766,
#40767,#40768,#40769,#40770,#40771,#40772,#40773,#40774,#40775,#40776,#40777,
#40778,#40779),.UNSPECIFIED.,.F.,.F.,(4,3,3,3,3,3,3,3,3,3,3,3,3,4),(-0.53478501993692,
-0.534277081309421,-0.456439695901019,-0.38064245929011,-0.348102919117109,
-0.328886681298388,-0.258595553176405,-0.246742105655551,-0.185056579241663,
-0.163339235199672,-0.143463957830519,-0.0808484674142256,-0.0206857924044652,
0.),.UNSPECIFIED.);
#882=B_SPLINE_CURVE_WITH_KNOTS('',3,(#40780,#40781,#40782,#40783,#40784,
#40785,#40786,#40787,#40788,#40789,#40790,#40791,#40792,#40793,#40794,#40795,
#40796,#40797,#40798,#40799,#40800,#40801,#40802,#40803,#40804),
 .UNSPECIFIED.,.F.,.F.,(4,3,3,3,3,3,3,3,4),(390.000549715688,390.249351157541,
390.749030224325,391.248709291108,391.748388357891,392.248067424674,392.747746491457,
393.24742555824,393.746279249921),.UNSPECIFIED.);
#883=B_SPLINE_CURVE_WITH_KNOTS('',3,(#40805,#40806,#40807,#40808,#40809,
#40810,#40811,#40812,#40813,#40814,#40815,#40816,#40817,#40818,#40819),
 .UNSPECIFIED.,.F.,.F.,(4,1,1,1,1,1,1,1,1,1,1,1,4),(9.98190079888485,10.4807544905659,
10.9804335573489,11.4801126241319,11.979791690915,12.479470757698,12.979149824481,
13.478828891264,13.9785079580471,14.4781870248301,14.9778660916131,15.4775451583961,
15.7079632679498),.UNSPECIFIED.);
#884=B_SPLINE_CURVE_WITH_KNOTS('',3,(#40821,#40822,#40823,#40824,#40825,
#40826,#40827,#40828,#40829,#40830,#40831),.UNSPECIFIED.,.F.,.F.,(4,1,1,
1,1,1,1,1,4),(12.0092477762453,12.5089268430284,13.0086059098114,13.5082849765944,
14.0079640433774,14.5076431101605,15.0073221769435,15.5070012437265,15.7079632679495),
 .UNSPECIFIED.);
#885=B_SPLINE_CURVE_WITH_KNOTS('',3,(#42825,#42826,#42827,#42828,#42829,
#42830,#42831,#42832,#42833,#42834,#42835,#42836,#42837,#42838,#42839,#42840,
#42841,#42842,#42843,#42844,#42845,#42846,#42847,#42848,#42849,#42850,#42851,
#42852,#42853,#42854,#42855,#42856,#42857,#42858,#42859,#42860,#42861,#42862,
#42863,#42864),.UNSPECIFIED.,.F.,.F.,(4,3,3,3,3,3,3,3,3,3,3,3,3,4),(-0.539097184344981,
-0.538720824057998,-0.476544551511477,-0.429912347101587,-0.401091234701428,
-0.381803774975435,-0.313681369269712,-0.290015733871917,-0.24230273417063,
-0.214804629165427,-0.192593514291413,-0.116696500404398,-0.0381316372362206,
0.),.UNSPECIFIED.);
#886=B_SPLINE_CURVE_WITH_KNOTS('',3,(#42865,#42866,#42867,#42868,#42869,
#42870,#42871,#42872,#42873,#42874),.UNSPECIFIED.,.F.,.F.,(4,3,3,4),(-394.746462758588,
-394.246783691805,-393.747104625022,-393.256204536838),.UNSPECIFIED.);
#887=B_SPLINE_CURVE_WITH_KNOTS('',3,(#42941,#42942,#42943,#42944,#42945,
#42946,#42947,#42948),.UNSPECIFIED.,.F.,.F.,(4,2,2,4),(0.756005737987019,
0.793568827564653,0.872922520054208,0.952276212543762),.UNSPECIFIED.);
#888=B_SPLINE_CURVE_WITH_KNOTS('',3,(#42951,#42952,#42953,#42954,#42955,
#42956,#42957,#42958,#42959,#42960,#42961,#42962,#42963,#42964),
 .UNSPECIFIED.,.F.,.F.,(4,2,2,2,2,2,4),(0.121154929624509,0.158718019202145,
0.238071711691699,0.317425404181254,0.396779096670809,0.476132789160363,
0.513695878738001),.UNSPECIFIED.);
#889=B_SPLINE_CURVE_WITH_KNOTS('',3,(#42965,#42966,#42967,#42968,#42969,
#42970,#42971,#42972),.UNSPECIFIED.,.F.,.F.,(4,2,2,4),(0.952276212543762,
1.03162990503332,1.11098359752287,1.14854668710052),.UNSPECIFIED.);
#890=B_SPLINE_CURVE_WITH_KNOTS('',3,(#42976,#42977,#42978,#42979,#42980,
#42981,#42982,#42983,#42984,#42985),.UNSPECIFIED.,.F.,.F.,(4,2,2,2,4),(0.,
0.0792165807733642,0.158433161546728,0.237648697074572,0.316864232602417),
 .UNSPECIFIED.);
#891=B_SPLINE_CURVE_WITH_KNOTS('',3,(#42986,#42987,#42988,#42989,#42990,
#42991,#42992,#42993,#42994,#42995,#42996,#42997,#42998,#42999,#43000,#43001,
#43002,#43003,#43004,#43005,#43006,#43007,#43008,#43009,#43010,#43011),
 .UNSPECIFIED.,.F.,.F.,(4,2,2,2,2,2,2,2,2,2,2,2,4),(0.316864232602417,0.396079768130261,
0.475295303658105,0.554511884431469,0.633728465204833,0.712945045978197,
0.792161626751562,0.871377162279406,0.95059269780725,1.02980823333509,1.10902376886294,
1.1882403496363,1.26745693040967),.UNSPECIFIED.);
#892=B_SPLINE_CURVE_WITH_KNOTS('',3,(#43043,#43044,#43045,#43046,#43047,
#43048),.UNSPECIFIED.,.F.,.F.,(4,2,4),(0.803821788694078,0.872950991853625,
0.952307212900975),.UNSPECIFIED.);
#893=B_SPLINE_CURVE_WITH_KNOTS('',3,(#43051,#43052,#43053,#43054,#43055,
#43056,#43057,#43058,#43059,#43060),.UNSPECIFIED.,.F.,.F.,(4,2,2,2,4),(0.168950313426762,
0.238079516586309,0.317435737633658,0.396791958681008,0.465921161840561),
 .UNSPECIFIED.);
#894=B_SPLINE_CURVE_WITH_KNOTS('',3,(#43061,#43062,#43063,#43064,#43065,
#43066),.UNSPECIFIED.,.F.,.F.,(4,2,4),(0.952307212900975,1.03166343394832,
1.10079263710787),.UNSPECIFIED.);
#895=B_SPLINE_CURVE_WITH_KNOTS('',3,(#43070,#43071,#43072,#43073,#43074,
#43075,#43076,#43077,#43078,#43079),.UNSPECIFIED.,.F.,.F.,(4,2,2,2,4),(0.,
0.0792165807733642,0.158433161546728,0.237648697074572,0.316864232602417),
 .UNSPECIFIED.);
#896=B_SPLINE_CURVE_WITH_KNOTS('',3,(#43080,#43081,#43082,#43083,#43084,
#43085,#43086,#43087,#43088,#43089,#43090,#43091,#43092,#43093,#43094,#43095,
#43096,#43097,#43098,#43099,#43100,#43101,#43102,#43103,#43104,#43105),
 .UNSPECIFIED.,.F.,.F.,(4,2,2,2,2,2,2,2,2,2,2,2,4),(0.316864232602417,0.396079768130261,
0.475295303658105,0.554511884431469,0.633728465204833,0.712945045978197,
0.792161626751562,0.871377162279406,0.95059269780725,1.02980823333509,1.10902376886294,
1.1882403496363,1.26745693040967),.UNSPECIFIED.);
#897=SPHERICAL_SURFACE('',#20034,0.29765);
#898=SPHERICAL_SURFACE('',#20036,0.29765);
#899=SPHERICAL_SURFACE('',#20038,0.29765);
#900=SPHERICAL_SURFACE('',#20040,0.29765);
#901=SPHERICAL_SURFACE('',#20042,0.29765);
#902=SPHERICAL_SURFACE('',#20044,0.29765);
#903=SPHERICAL_SURFACE('',#20046,0.29765);
#904=SPHERICAL_SURFACE('',#20049,0.309556);
#905=SPHERICAL_SURFACE('',#20065,0.309556);
#906=SPHERICAL_SURFACE('',#20070,0.309556);
#907=SPHERICAL_SURFACE('',#20076,0.309556);
#908=SPHERICAL_SURFACE('',#20081,0.309556);
#909=SPHERICAL_SURFACE('',#20086,0.309556);
#910=SPHERICAL_SURFACE('',#20094,0.309556);
#911=SPHERICAL_SURFACE('',#20162,0.3969);
#912=SPHERICAL_SURFACE('',#20164,0.3969);
#913=SPHERICAL_SURFACE('',#20166,0.3969);
#914=SPHERICAL_SURFACE('',#20168,0.3969);
#915=SPHERICAL_SURFACE('',#20170,0.3969);
#916=SPHERICAL_SURFACE('',#20172,0.3969);
#917=SPHERICAL_SURFACE('',#20174,0.3969);
#918=SPHERICAL_SURFACE('',#20176,0.3969);
#919=SPHERICAL_SURFACE('',#20179,0.412776);
#920=SPHERICAL_SURFACE('',#20195,0.412776);
#921=SPHERICAL_SURFACE('',#20200,0.412776);
#922=SPHERICAL_SURFACE('',#20205,0.412776);
#923=SPHERICAL_SURFACE('',#20210,0.412776);
#924=SPHERICAL_SURFACE('',#20215,0.412776);
#925=SPHERICAL_SURFACE('',#20220,0.412776);
#926=SPHERICAL_SURFACE('',#20228,0.412776);
#927=TOROIDAL_SURFACE('',#19994,1.1,0.309556);
#928=TOROIDAL_SURFACE('',#20014,1.1,0.309556);
#929=TOROIDAL_SURFACE('',#20122,1.675,0.412776);
#930=TOROIDAL_SURFACE('',#20142,1.675,0.412776);
#931=ORIENTED_CLOSED_SHELL('',*,#18563,.F.);
#932=ORIENTED_CLOSED_SHELL('',*,#18591,.F.);
#933=ORIENTED_CLOSED_SHELL('',*,#18592,.F.);
#934=ORIENTED_CLOSED_SHELL('',*,#18596,.F.);
#935=ORIENTED_CLOSED_SHELL('',*,#18608,.F.);
#936=ORIENTED_CLOSED_SHELL('',*,#18611,.F.);
#937=ORIENTED_CLOSED_SHELL('',*,#18622,.F.);
#938=BREP_WITH_VOIDS('Body1',#18564,(#931));
#939=BREP_WITH_VOIDS('Body1',#18590,(#932));
#940=BREP_WITH_VOIDS('Body1',#18593,(#933));
#941=BREP_WITH_VOIDS('Body1',#18595,(#934));
#942=BREP_WITH_VOIDS('Body1',#18609,(#935));
#943=BREP_WITH_VOIDS('Body1',#18610,(#936));
#944=BREP_WITH_VOIDS('Body1',#18621,(#937));
#945=CONICAL_SURFACE('',#19921,0.55,0.785398163397448);
#946=CONICAL_SURFACE('',#19927,0.55,0.785398163397441);
#947=CONICAL_SURFACE('',#19981,0.4,0.785398163397448);
#948=CONICAL_SURFACE('',#19985,0.41,0.785398163397448);
#949=CONICAL_SURFACE('',#19989,0.26,0.463647609000806);
#950=CONICAL_SURFACE('',#20005,0.63,0.785398163397448);
#951=CONICAL_SURFACE('',#20012,0.63,0.785398163397448);
#952=CONICAL_SURFACE('',#20025,1.57,0.785398163397449);
#953=CONICAL_SURFACE('',#20029,1.57,0.785398163397449);
#954=CONICAL_SURFACE('',#20133,1.05,0.785398163397449);
#955=CONICAL_SURFACE('',#20140,1.05,0.785398163397449);
#956=CONICAL_SURFACE('',#20153,2.3,0.785398163397449);
#957=CONICAL_SURFACE('',#20157,2.3,0.785398163397449);
#958=CONICAL_SURFACE('',#20263,0.4,0.785398163397448);
#959=CONICAL_SURFACE('',#20267,0.41,0.785398163397448);
#960=CONICAL_SURFACE('',#20271,0.26,0.463647609000806);
#961=CONICAL_SURFACE('',#20295,0.325,0.785398163397448);
#962=CONICAL_SURFACE('',#20299,0.335,0.785398163397448);
#963=CONICAL_SURFACE('',#20303,0.21,0.463647609000806);
#964=CONICAL_SURFACE('',#20359,0.4,0.785398163397448);
#965=CONICAL_SURFACE('',#20363,0.41,0.785398163397448);
#966=CONICAL_SURFACE('',#20367,0.26,0.463647609000806);
#967=CONICAL_SURFACE('',#20371,0.225,0.785398163397448);
#968=CONICAL_SURFACE('',#20408,0.4,0.785398163397448);
#969=CONICAL_SURFACE('',#20412,0.41,0.785398163397448);
#970=CONICAL_SURFACE('',#20416,0.26,0.463647609000806);
#971=CONICAL_SURFACE('',#20753,0.325,0.785398163397448);
#972=CONICAL_SURFACE('',#20757,0.335,0.785398163397448);
#973=CONICAL_SURFACE('',#20761,0.21,0.463647609000806);
#974=CONICAL_SURFACE('',#20767,0.325,0.785398163397448);
#975=CONICAL_SURFACE('',#20771,0.335,0.785398163397448);
#976=CONICAL_SURFACE('',#20775,0.21,0.463647609000806);
#977=CONICAL_SURFACE('',#20779,0.18,0.785398163397448);
#978=CONICAL_SURFACE('',#21140,0.235,0.785398163397448);
#979=CONICAL_SURFACE('',#21144,0.2125,0.785398163397448);
#980=CONICAL_SURFACE('',#21159,0.475,0.785398163397449);
#981=CONICAL_SURFACE('',#21163,0.485,0.785398163397448);
#982=CONICAL_SURFACE('',#21167,0.31,0.463647609000806);
#983=CONICAL_SURFACE('',#21171,0.27,0.785398163397448);
#984=SHAPE_REPRESENTATION_RELATIONSHIP('SRR','None',#43796,#1044);
#985=SHAPE_REPRESENTATION_RELATIONSHIP('SRR','None',#43797,#1045);
#986=SHAPE_REPRESENTATION_RELATIONSHIP('SRR','None',#43798,#1046);
#987=SHAPE_REPRESENTATION_RELATIONSHIP('SRR','None',#43799,#1047);
#988=SHAPE_REPRESENTATION_RELATIONSHIP('SRR','None',#43800,#1048);
#989=SHAPE_REPRESENTATION_RELATIONSHIP('SRR','None',#43801,#1049);
#990=SHAPE_REPRESENTATION_RELATIONSHIP('SRR','None',#43802,#1050);
#991=SHAPE_REPRESENTATION_RELATIONSHIP('SRR','None',#43803,#1051);
#992=SHAPE_REPRESENTATION_RELATIONSHIP('SRR','None',#43804,#1052);
#993=SHAPE_REPRESENTATION_RELATIONSHIP('SRR','None',#43805,#1053);
#994=SHAPE_REPRESENTATION_RELATIONSHIP('SRR','None',#43806,#1054);
#995=SHAPE_REPRESENTATION_RELATIONSHIP('SRR','None',#43807,#1055);
#996=SHAPE_REPRESENTATION_RELATIONSHIP('SRR','None',#43808,#1056);
#997=SHAPE_REPRESENTATION_RELATIONSHIP('SRR','None',#43809,#1057);
#998=SHAPE_REPRESENTATION_RELATIONSHIP('SRR','None',#43810,#1058);
#999=SHAPE_REPRESENTATION_RELATIONSHIP('SRR','None',#43811,#1059);
#1000=SHAPE_REPRESENTATION_RELATIONSHIP('SRR','None',#43812,#1060);
#1001=SHAPE_REPRESENTATION_RELATIONSHIP('SRR','None',#43813,#1061);
#1002=SHAPE_REPRESENTATION_RELATIONSHIP('SRR','None',#43814,#1062);
#1003=SHAPE_REPRESENTATION_RELATIONSHIP('SRR','None',#43815,#1063);
#1004=SHAPE_REPRESENTATION_RELATIONSHIP('SRR','None',#43816,#1064);
#1005=SHAPE_REPRESENTATION_RELATIONSHIP('SRR','None',#43817,#1065);
#1006=SHAPE_REPRESENTATION_RELATIONSHIP('SRR','None',#43818,#1066);
#1007=SHAPE_REPRESENTATION_RELATIONSHIP('SRR','None',#43820,#1067);
#1008=SHAPE_REPRESENTATION_RELATIONSHIP('SRR','None',#43821,#1068);
#1009=SHAPE_REPRESENTATION_RELATIONSHIP('SRR','None',#43822,#1069);
#1010=SHAPE_REPRESENTATION_RELATIONSHIP('SRR','None',#43823,#1070);
#1011=SHAPE_REPRESENTATION_RELATIONSHIP('SRR','None',#43824,#1071);
#1012=SHAPE_REPRESENTATION_RELATIONSHIP('SRR','None',#43826,#1072);
#1013=SHAPE_REPRESENTATION_RELATIONSHIP('SRR','None',#43827,#1073);
#1014=SHAPE_REPRESENTATION_RELATIONSHIP('SRR','None',#43828,#1074);
#1015=SHAPE_REPRESENTATION_RELATIONSHIP('SRR','None',#43829,#1075);
#1016=SHAPE_REPRESENTATION_RELATIONSHIP('SRR','None',#43830,#1076);
#1017=SHAPE_REPRESENTATION_RELATIONSHIP('SRR','None',#43831,#1077);
#1018=SHAPE_REPRESENTATION_RELATIONSHIP('SRR','None',#43832,#1078);
#1019=SHAPE_REPRESENTATION_RELATIONSHIP('SRR','None',#43833,#1079);
#1020=SHAPE_REPRESENTATION_RELATIONSHIP('SRR','None',#43834,#1080);
#1021=SHAPE_REPRESENTATION_RELATIONSHIP('SRR','None',#43835,#1081);
#1022=SHAPE_REPRESENTATION_RELATIONSHIP('SRR','None',#43836,#1082);
#1023=SHAPE_REPRESENTATION_RELATIONSHIP('SRR','None',#43838,#1083);
#1024=SHAPE_REPRESENTATION_RELATIONSHIP('SRR','None',#43839,#1084);
#1025=SHAPE_REPRESENTATION_RELATIONSHIP('SRR','None',#43840,#1085);
#1026=SHAPE_REPRESENTATION_RELATIONSHIP('SRR','None',#43841,#1086);
#1027=SHAPE_REPRESENTATION_RELATIONSHIP('SRR','None',#43842,#1087);
#1028=SHAPE_REPRESENTATION_RELATIONSHIP('SRR','None',#43843,#1088);
#1029=SHAPE_REPRESENTATION_RELATIONSHIP('SRR','None',#43845,#1089);
#1030=SHAPE_REPRESENTATION_RELATIONSHIP('SRR','None',#43846,#1090);
#1031=SHAPE_REPRESENTATION_RELATIONSHIP('SRR','None',#43847,#1091);
#1032=SHAPE_REPRESENTATION_RELATIONSHIP('SRR','None',#43848,#1092);
#1033=SHAPE_REPRESENTATION_RELATIONSHIP('SRR','None',#43849,#1093);
#1034=SHAPE_REPRESENTATION_RELATIONSHIP('SRR','None',#43851,#1094);
#1035=SHAPE_REPRESENTATION_RELATIONSHIP('SRR','None',#43852,#1095);
#1036=SHAPE_REPRESENTATION_RELATIONSHIP('SRR','None',#43853,#1096);
#1037=SHAPE_REPRESENTATION_RELATIONSHIP('SRR','None',#43854,#1097);
#1038=SHAPE_REPRESENTATION_RELATIONSHIP('SRR','None',#43855,#1098);
#1039=SHAPE_REPRESENTATION_RELATIONSHIP('SRR','None',#43856,#1099);
#1040=SHAPE_REPRESENTATION_RELATIONSHIP('SRR','None',#43857,#1100);
#1041=SHAPE_REPRESENTATION_RELATIONSHIP('SRR','None',#43858,#1101);
#1042=SHAPE_REPRESENTATION_RELATIONSHIP('SRR','None',#43859,#1102);
#1043=SHAPE_REPRESENTATION_RELATIONSHIP('SRR','None',#43860,#1103);
#1044=ADVANCED_BREP_SHAPE_REPRESENTATION('',(#1179),#43456);
#1045=ADVANCED_BREP_SHAPE_REPRESENTATION('',(#1180),#43457);
#1046=ADVANCED_BREP_SHAPE_REPRESENTATION('',(#1181),#43458);
#1047=ADVANCED_BREP_SHAPE_REPRESENTATION('',(#1182),#43459);
#1048=ADVANCED_BREP_SHAPE_REPRESENTATION('',(#1183),#43460);
#1049=ADVANCED_BREP_SHAPE_REPRESENTATION('',(#1184),#43461);
#1050=ADVANCED_BREP_SHAPE_REPRESENTATION('',(#1185),#43462);
#1051=ADVANCED_BREP_SHAPE_REPRESENTATION('',(#1186),#43463);
#1052=ADVANCED_BREP_SHAPE_REPRESENTATION('',(#1187),#43464);
#1053=ADVANCED_BREP_SHAPE_REPRESENTATION('',(#1188),#43465);
#1054=ADVANCED_BREP_SHAPE_REPRESENTATION('',(#1189),#43466);
#1055=ADVANCED_BREP_SHAPE_REPRESENTATION('',(#1190),#43467);
#1056=ADVANCED_BREP_SHAPE_REPRESENTATION('',(#1191),#43468);
#1057=ADVANCED_BREP_SHAPE_REPRESENTATION('',(#1192),#43469);
#1058=ADVANCED_BREP_SHAPE_REPRESENTATION('',(#1193),#43470);
#1059=ADVANCED_BREP_SHAPE_REPRESENTATION('',(#1194),#43471);
#1060=ADVANCED_BREP_SHAPE_REPRESENTATION('',(#1195),#43472);
#1061=ADVANCED_BREP_SHAPE_REPRESENTATION('',(#1196),#43473);
#1062=ADVANCED_BREP_SHAPE_REPRESENTATION('',(#1197),#43474);
#1063=ADVANCED_BREP_SHAPE_REPRESENTATION('',(#1198),#43475);
#1064=ADVANCED_BREP_SHAPE_REPRESENTATION('',(#1199),#43476);
#1065=ADVANCED_BREP_SHAPE_REPRESENTATION('',(#1200),#43477);
#1066=ADVANCED_BREP_SHAPE_REPRESENTATION('',(#938),#43478);
#1067=ADVANCED_BREP_SHAPE_REPRESENTATION('',(#1201),#43480);
#1068=ADVANCED_BREP_SHAPE_REPRESENTATION('',(#1202),#43481);
#1069=ADVANCED_BREP_SHAPE_REPRESENTATION('',(#1203,#1204,#1205,#1206,#1207,
#1208,#1209),#43482);
#1070=ADVANCED_BREP_SHAPE_REPRESENTATION('',(#1210),#43483);
#1071=ADVANCED_BREP_SHAPE_REPRESENTATION('',(#1211,#1212),#43484);
#1072=ADVANCED_BREP_SHAPE_REPRESENTATION('',(#1213),#43486);
#1073=ADVANCED_BREP_SHAPE_REPRESENTATION('',(#1214),#43487);
#1074=ADVANCED_BREP_SHAPE_REPRESENTATION('',(#1215,#1216,#1217,#1218,#1219,
#1220,#1221,#1222),#43488);
#1075=ADVANCED_BREP_SHAPE_REPRESENTATION('',(#1223),#43489);
#1076=ADVANCED_BREP_SHAPE_REPRESENTATION('',(#1224,#1225),#43490);
#1077=ADVANCED_BREP_SHAPE_REPRESENTATION('',(#939),#43491);
#1078=ADVANCED_BREP_SHAPE_REPRESENTATION('',(#940),#43492);
#1079=ADVANCED_BREP_SHAPE_REPRESENTATION('',(#1226),#43493);
#1080=ADVANCED_BREP_SHAPE_REPRESENTATION('',(#941),#43494);
#1081=ADVANCED_BREP_SHAPE_REPRESENTATION('',(#1227),#43495);
#1082=ADVANCED_BREP_SHAPE_REPRESENTATION('',(#1228),#43496);
#1083=ADVANCED_BREP_SHAPE_REPRESENTATION('',(#1229),#43498);
#1084=ADVANCED_BREP_SHAPE_REPRESENTATION('',(#1230),#43499);
#1085=ADVANCED_BREP_SHAPE_REPRESENTATION('',(#1231),#43500);
#1086=ADVANCED_BREP_SHAPE_REPRESENTATION('',(#1232),#43501);
#1087=ADVANCED_BREP_SHAPE_REPRESENTATION('',(#1233),#43502);
#1088=ADVANCED_BREP_SHAPE_REPRESENTATION('',(#1234),#43503);
#1089=ADVANCED_BREP_SHAPE_REPRESENTATION('',(#1235),#43505);
#1090=ADVANCED_BREP_SHAPE_REPRESENTATION('',(#1236),#43506);
#1091=ADVANCED_BREP_SHAPE_REPRESENTATION('',(#1237),#43507);
#1092=ADVANCED_BREP_SHAPE_REPRESENTATION('',(#942),#43508);
#1093=ADVANCED_BREP_SHAPE_REPRESENTATION('',(#943),#43509);
#1094=ADVANCED_BREP_SHAPE_REPRESENTATION('',(#1238),#43511);
#1095=ADVANCED_BREP_SHAPE_REPRESENTATION('',(#1239),#43512);
#1096=ADVANCED_BREP_SHAPE_REPRESENTATION('',(#1240),#43513);
#1097=ADVANCED_BREP_SHAPE_REPRESENTATION('',(#1241),#43514);
#1098=ADVANCED_BREP_SHAPE_REPRESENTATION('',(#1242),#43515);
#1099=ADVANCED_BREP_SHAPE_REPRESENTATION('',(#1243),#43516);
#1100=ADVANCED_BREP_SHAPE_REPRESENTATION('',(#1244),#43517);
#1101=ADVANCED_BREP_SHAPE_REPRESENTATION('',(#1245),#43518);
#1102=ADVANCED_BREP_SHAPE_REPRESENTATION('',(#1246),#43519);
#1103=ADVANCED_BREP_SHAPE_REPRESENTATION('',(#944),#43520);
#1104=STYLED_ITEM('',(#44181),#1179);
#1105=STYLED_ITEM('',(#44188),#1180);
#1106=STYLED_ITEM('',(#44188),#1181);
#1107=STYLED_ITEM('',(#44195),#1182);
#1108=STYLED_ITEM('',(#44181),#1183);
#1109=STYLED_ITEM('',(#44181),#1184);
#1110=STYLED_ITEM('',(#44181),#1185);
#1111=STYLED_ITEM('',(#44181),#1186);
#1112=STYLED_ITEM('',(#44181),#1187);
#1113=STYLED_ITEM('',(#44181),#1188);
#1114=STYLED_ITEM('',(#44202),#1189);
#1115=STYLED_ITEM('',(#44202),#1190);
#1116=STYLED_ITEM('',(#44202),#1191);
#1117=STYLED_ITEM('',(#44202),#1192);
#1118=STYLED_ITEM('',(#44188),#1193);
#1119=STYLED_ITEM('',(#44216),#1194);
#1120=STYLED_ITEM('',(#44188),#1195);
#1121=STYLED_ITEM('',(#44216),#1196);
#1122=STYLED_ITEM('',(#44195),#1197);
#1123=STYLED_ITEM('',(#44216),#1198);
#1124=STYLED_ITEM('',(#44202),#1199);
#1125=STYLED_ITEM('',(#44202),#1200);
#1126=STYLED_ITEM('',(#44209),#938);
#1127=STYLED_ITEM('',(#44202),#1201);
#1128=STYLED_ITEM('',(#44202),#1202);
#1129=STYLED_ITEM('',(#44202),#1203);
#1130=STYLED_ITEM('',(#44202),#1204);
#1131=STYLED_ITEM('',(#44202),#1205);
#1132=STYLED_ITEM('',(#44202),#1206);
#1133=STYLED_ITEM('',(#44202),#1207);
#1134=STYLED_ITEM('',(#44202),#1208);
#1135=STYLED_ITEM('',(#44202),#1209);
#1136=STYLED_ITEM('',(#44202),#1210);
#1137=STYLED_ITEM('',(#44202),#1211);
#1138=STYLED_ITEM('',(#44202),#1212);
#1139=STYLED_ITEM('',(#44202),#1213);
#1140=STYLED_ITEM('',(#44202),#1214);
#1141=STYLED_ITEM('',(#44202),#1215);
#1142=STYLED_ITEM('',(#44202),#1216);
#1143=STYLED_ITEM('',(#44202),#1217);
#1144=STYLED_ITEM('',(#44202),#1218);
#1145=STYLED_ITEM('',(#44202),#1219);
#1146=STYLED_ITEM('',(#44202),#1220);
#1147=STYLED_ITEM('',(#44202),#1221);
#1148=STYLED_ITEM('',(#44202),#1222);
#1149=STYLED_ITEM('',(#44202),#1223);
#1150=STYLED_ITEM('',(#44202),#1224);
#1151=STYLED_ITEM('',(#44202),#1225);
#1152=STYLED_ITEM('',(#44209),#939);
#1153=STYLED_ITEM('',(#44209),#940);
#1154=STYLED_ITEM('',(#44188),#1226);
#1155=STYLED_ITEM('',(#44209),#941);
#1156=STYLED_ITEM('',(#44209),#1227);
#1157=STYLED_ITEM('',(#44209),#1228);
#1158=STYLED_ITEM('',(#44188),#1229);
#1159=STYLED_ITEM('',(#44181),#1230);
#1160=STYLED_ITEM('',(#44181),#1231);
#1161=STYLED_ITEM('',(#44209),#1232);
#1162=STYLED_ITEM('',(#44216),#1233);
#1163=STYLED_ITEM('',(#44195),#1234);
#1164=STYLED_ITEM('',(#44216),#1235);
#1165=STYLED_ITEM('',(#44195),#1236);
#1166=STYLED_ITEM('',(#44209),#1237);
#1167=STYLED_ITEM('',(#44209),#942);
#1168=STYLED_ITEM('',(#44209),#943);
#1169=STYLED_ITEM('',(#44209),#1238);
#1170=STYLED_ITEM('',(#44202),#1239);
#1171=STYLED_ITEM('',(#44202),#1240);
#1172=STYLED_ITEM('',(#44195),#1241);
#1173=STYLED_ITEM('',(#44195),#1242);
#1174=STYLED_ITEM('',(#44195),#1243);
#1175=STYLED_ITEM('',(#44202),#1244);
#1176=STYLED_ITEM('',(#44209),#1245);
#1177=STYLED_ITEM('',(#44209),#1246);
#1178=STYLED_ITEM('',(#44209),#944);
#1179=MANIFOLD_SOLID_BREP('Body1',#18541);
#1180=MANIFOLD_SOLID_BREP('Body1',#18542);
#1181=MANIFOLD_SOLID_BREP('Body1',#18543);
#1182=MANIFOLD_SOLID_BREP('Body1',#18544);
#1183=MANIFOLD_SOLID_BREP('Body1',#18545);
#1184=MANIFOLD_SOLID_BREP('Body1',#18546);
#1185=MANIFOLD_SOLID_BREP('Body1',#18547);
#1186=MANIFOLD_SOLID_BREP('Body1',#18548);
#1187=MANIFOLD_SOLID_BREP('Body1',#18549);
#1188=MANIFOLD_SOLID_BREP('Body1',#18550);
#1189=MANIFOLD_SOLID_BREP('Body1',#18551);
#1190=MANIFOLD_SOLID_BREP('Body1',#18552);
#1191=MANIFOLD_SOLID_BREP('Body1',#18553);
#1192=MANIFOLD_SOLID_BREP('Body1',#18554);
#1193=MANIFOLD_SOLID_BREP('Body1',#18555);
#1194=MANIFOLD_SOLID_BREP('Body1',#18556);
#1195=MANIFOLD_SOLID_BREP('Body1',#18557);
#1196=MANIFOLD_SOLID_BREP('Body1',#18558);
#1197=MANIFOLD_SOLID_BREP('Body1',#18559);
#1198=MANIFOLD_SOLID_BREP('Body1',#18560);
#1199=MANIFOLD_SOLID_BREP('Body1',#18561);
#1200=MANIFOLD_SOLID_BREP('Body1',#18562);
#1201=MANIFOLD_SOLID_BREP('Body1',#18565);
#1202=MANIFOLD_SOLID_BREP('Body1',#18566);
#1203=MANIFOLD_SOLID_BREP('Body1',#18567);
#1204=MANIFOLD_SOLID_BREP('Body2',#18568);
#1205=MANIFOLD_SOLID_BREP('Body3',#18569);
#1206=MANIFOLD_SOLID_BREP('Body4',#18570);
#1207=MANIFOLD_SOLID_BREP('Body5',#18571);
#1208=MANIFOLD_SOLID_BREP('Body6',#18572);
#1209=MANIFOLD_SOLID_BREP('Body7',#18573);
#1210=MANIFOLD_SOLID_BREP('Continuous crown cage',#18574);
#1211=MANIFOLD_SOLID_BREP('Body1',#18575);
#1212=MANIFOLD_SOLID_BREP('Body2',#18576);
#1213=MANIFOLD_SOLID_BREP('Body1',#18577);
#1214=MANIFOLD_SOLID_BREP('Body1',#18578);
#1215=MANIFOLD_SOLID_BREP('Body1',#18579);
#1216=MANIFOLD_SOLID_BREP('Body2',#18580);
#1217=MANIFOLD_SOLID_BREP('Body3',#18581);
#1218=MANIFOLD_SOLID_BREP('Body4',#18582);
#1219=MANIFOLD_SOLID_BREP('Body5',#18583);
#1220=MANIFOLD_SOLID_BREP('Body6',#18584);
#1221=MANIFOLD_SOLID_BREP('Body7',#18585);
#1222=MANIFOLD_SOLID_BREP('Body8',#18586);
#1223=MANIFOLD_SOLID_BREP('Continuous crown cage',#18587);
#1224=MANIFOLD_SOLID_BREP('Body1',#18588);
#1225=MANIFOLD_SOLID_BREP('Body2',#18589);
#1226=MANIFOLD_SOLID_BREP('Body1',#18594);
#1227=MANIFOLD_SOLID_BREP('Body1',#18597);
#1228=MANIFOLD_SOLID_BREP('Body1',#18598);
#1229=MANIFOLD_SOLID_BREP('Body1',#18599);
#1230=MANIFOLD_SOLID_BREP('Body1',#18600);
#1231=MANIFOLD_SOLID_BREP('Body1',#18601);
#1232=MANIFOLD_SOLID_BREP('Body1',#18602);
#1233=MANIFOLD_SOLID_BREP('Body1',#18603);
#1234=MANIFOLD_SOLID_BREP('Body1',#18604);
#1235=MANIFOLD_SOLID_BREP('Body1',#18605);
#1236=MANIFOLD_SOLID_BREP('Body1',#18606);
#1237=MANIFOLD_SOLID_BREP('Body1',#18607);
#1238=MANIFOLD_SOLID_BREP('Body1',#18612);
#1239=MANIFOLD_SOLID_BREP('Body1',#18613);
#1240=MANIFOLD_SOLID_BREP('Body1',#18614);
#1241=MANIFOLD_SOLID_BREP('Body1',#18615);
#1242=MANIFOLD_SOLID_BREP('Body1',#18616);
#1243=MANIFOLD_SOLID_BREP('Body1',#18617);
#1244=MANIFOLD_SOLID_BREP('Body1',#18618);
#1245=MANIFOLD_SOLID_BREP('Body1',#18619);
#1246=MANIFOLD_SOLID_BREP('Body1',#18620);
#1247=FACE_BOUND('',#3250,.T.);
#1248=FACE_BOUND('',#3251,.T.);
#1249=FACE_BOUND('',#3252,.T.);
#1250=FACE_BOUND('',#3253,.T.);
#1251=FACE_BOUND('',#3254,.T.);
#1252=FACE_BOUND('',#3255,.T.);
#1253=FACE_BOUND('',#3256,.T.);
#1254=FACE_BOUND('',#3257,.T.);
#1255=FACE_BOUND('',#3258,.T.);
#1256=FACE_BOUND('',#3259,.T.);
#1257=FACE_BOUND('',#3260,.T.);
#1258=FACE_BOUND('',#3261,.T.);
#1259=FACE_BOUND('',#3262,.T.);
#1260=FACE_BOUND('',#3263,.T.);
#1261=FACE_BOUND('',#3264,.T.);
#1262=FACE_BOUND('',#3265,.T.);
#1263=FACE_BOUND('',#3266,.T.);
#1264=FACE_BOUND('',#3267,.T.);
#1265=FACE_BOUND('',#3268,.T.);
#1266=FACE_BOUND('',#3269,.T.);
#1267=FACE_BOUND('',#3271,.T.);
#1268=FACE_BOUND('',#3272,.T.);
#1269=FACE_BOUND('',#3273,.T.);
#1270=FACE_BOUND('',#3274,.T.);
#1271=FACE_BOUND('',#3275,.T.);
#1272=FACE_BOUND('',#3276,.T.);
#1273=FACE_BOUND('',#3277,.T.);
#1274=FACE_BOUND('',#3278,.T.);
#1275=FACE_BOUND('',#3279,.T.);
#1276=FACE_BOUND('',#3280,.T.);
#1277=FACE_BOUND('',#3281,.T.);
#1278=FACE_BOUND('',#3282,.T.);
#1279=FACE_BOUND('',#3283,.T.);
#1280=FACE_BOUND('',#3284,.T.);
#1281=FACE_BOUND('',#3285,.T.);
#1282=FACE_BOUND('',#3286,.T.);
#1283=FACE_BOUND('',#3318,.T.);
#1284=FACE_BOUND('',#3319,.T.);
#1285=FACE_BOUND('',#3320,.T.);
#1286=FACE_BOUND('',#3321,.T.);
#1287=FACE_BOUND('',#3322,.T.);
#1288=FACE_BOUND('',#3323,.T.);
#1289=FACE_BOUND('',#3324,.T.);
#1290=FACE_BOUND('',#3325,.T.);
#1291=FACE_BOUND('',#3326,.T.);
#1292=FACE_BOUND('',#3327,.T.);
#1293=FACE_BOUND('',#3328,.T.);
#1294=FACE_BOUND('',#3330,.T.);
#1295=FACE_BOUND('',#3331,.T.);
#1296=FACE_BOUND('',#3332,.T.);
#1297=FACE_BOUND('',#3333,.T.);
#1298=FACE_BOUND('',#3334,.T.);
#1299=FACE_BOUND('',#3335,.T.);
#1300=FACE_BOUND('',#3336,.T.);
#1301=FACE_BOUND('',#3337,.T.);
#1302=FACE_BOUND('',#3338,.T.);
#1303=FACE_BOUND('',#3339,.T.);
#1304=FACE_BOUND('',#3340,.T.);
#1305=FACE_BOUND('',#3353,.T.);
#1306=FACE_BOUND('',#3354,.T.);
#1307=FACE_BOUND('',#3357,.T.);
#1308=FACE_BOUND('',#3358,.T.);
#1309=FACE_BOUND('',#3360,.T.);
#1310=FACE_BOUND('',#3361,.T.);
#1311=FACE_BOUND('',#3363,.T.);
#1312=FACE_BOUND('',#3364,.T.);
#1313=FACE_BOUND('',#3377,.T.);
#1314=FACE_BOUND('',#3378,.T.);
#1315=FACE_BOUND('',#3381,.T.);
#1316=FACE_BOUND('',#3382,.T.);
#1317=FACE_BOUND('',#3384,.T.);
#1318=FACE_BOUND('',#3385,.T.);
#1319=FACE_BOUND('',#3387,.T.);
#1320=FACE_BOUND('',#3388,.T.);
#1321=FACE_BOUND('',#3396,.T.);
#1322=FACE_BOUND('',#3397,.T.);
#1323=FACE_BOUND('',#3400,.T.);
#1324=FACE_BOUND('',#3401,.T.);
#1325=FACE_BOUND('',#3405,.T.);
#1326=FACE_BOUND('',#3406,.T.);
#1327=FACE_BOUND('',#3415,.T.);
#1328=FACE_BOUND('',#3416,.T.);
#1329=FACE_BOUND('',#3420,.T.);
#1330=FACE_BOUND('',#3421,.T.);
#1331=FACE_BOUND('',#3424,.T.);
#1332=FACE_BOUND('',#3425,.T.);
#1333=FACE_BOUND('',#3434,.T.);
#1334=FACE_BOUND('',#3435,.T.);
#1335=FACE_BOUND('',#3438,.T.);
#1336=FACE_BOUND('',#3439,.T.);
#1337=FACE_BOUND('',#3443,.T.);
#1338=FACE_BOUND('',#3444,.T.);
#1339=FACE_BOUND('',#3453,.T.);
#1340=FACE_BOUND('',#3454,.T.);
#1341=FACE_BOUND('',#3458,.T.);
#1342=FACE_BOUND('',#3459,.T.);
#1343=FACE_BOUND('',#3462,.T.);
#1344=FACE_BOUND('',#3463,.T.);
#1345=FACE_BOUND('',#3478,.T.);
#1346=FACE_BOUND('',#3482,.T.);
#1347=FACE_BOUND('',#3483,.T.);
#1348=FACE_BOUND('',#3484,.T.);
#1349=FACE_BOUND('',#3485,.T.);
#1350=FACE_BOUND('',#3491,.T.);
#1351=FACE_BOUND('',#3492,.T.);
#1352=FACE_BOUND('',#3493,.T.);
#1353=FACE_BOUND('',#3494,.T.);
#1354=FACE_BOUND('',#3496,.T.);
#1355=FACE_BOUND('',#3497,.T.);
#1356=FACE_BOUND('',#3498,.T.);
#1357=FACE_BOUND('',#3499,.T.);
#1358=FACE_BOUND('',#3500,.T.);
#1359=FACE_BOUND('',#3516,.T.);
#1360=FACE_BOUND('',#3521,.T.);
#1361=FACE_BOUND('',#3522,.T.);
#1362=FACE_BOUND('',#3524,.T.);
#1363=FACE_BOUND('',#3525,.T.);
#1364=FACE_BOUND('',#3526,.T.);
#1365=FACE_BOUND('',#3527,.T.);
#1366=FACE_BOUND('',#3528,.T.);
#1367=FACE_BOUND('',#3529,.T.);
#1368=FACE_BOUND('',#3533,.T.);
#1369=FACE_BOUND('',#3534,.T.);
#1370=FACE_BOUND('',#3536,.T.);
#1371=FACE_BOUND('',#3537,.T.);
#1372=FACE_BOUND('',#3538,.T.);
#1373=FACE_BOUND('',#3539,.T.);
#1374=FACE_BOUND('',#3540,.T.);
#1375=FACE_BOUND('',#3541,.T.);
#1376=FACE_BOUND('',#3547,.T.);
#1377=FACE_BOUND('',#3551,.T.);
#1378=FACE_BOUND('',#3552,.T.);
#1379=FACE_BOUND('',#3553,.T.);
#1380=FACE_BOUND('',#3554,.T.);
#1381=FACE_BOUND('',#3556,.T.);
#1382=FACE_BOUND('',#3557,.T.);
#1383=FACE_BOUND('',#3558,.T.);
#1384=FACE_BOUND('',#3559,.T.);
#1385=FACE_BOUND('',#3565,.T.);
#1386=FACE_BOUND('',#3569,.T.);
#1387=FACE_BOUND('',#3570,.T.);
#1388=FACE_BOUND('',#3571,.T.);
#1389=FACE_BOUND('',#3572,.T.);
#1390=FACE_BOUND('',#3574,.T.);
#1391=FACE_BOUND('',#3575,.T.);
#1392=FACE_BOUND('',#3576,.T.);
#1393=FACE_BOUND('',#3577,.T.);
#1394=FACE_BOUND('',#3583,.T.);
#1395=FACE_BOUND('',#3588,.T.);
#1396=FACE_BOUND('',#3595,.T.);
#1397=FACE_BOUND('',#3600,.T.);
#1398=FACE_BOUND('',#3604,.T.);
#1399=FACE_BOUND('',#3607,.T.);
#1400=FACE_BOUND('',#3610,.T.);
#1401=FACE_BOUND('',#3613,.T.);
#1402=FACE_BOUND('',#3620,.T.);
#1403=FACE_BOUND('',#3621,.T.);
#1404=FACE_BOUND('',#3622,.T.);
#1405=FACE_BOUND('',#3623,.T.);
#1406=FACE_BOUND('',#3625,.T.);
#1407=FACE_BOUND('',#3626,.T.);
#1408=FACE_BOUND('',#3627,.T.);
#1409=FACE_BOUND('',#3628,.T.);
#1410=FACE_BOUND('',#3758,.T.);
#1411=FACE_BOUND('',#3759,.T.);
#1412=FACE_BOUND('',#3762,.T.);
#1413=FACE_BOUND('',#3763,.T.);
#1414=FACE_BOUND('',#3764,.T.);
#1415=FACE_BOUND('',#3765,.T.);
#1416=FACE_BOUND('',#3766,.T.);
#1417=FACE_BOUND('',#3767,.T.);
#1418=FACE_BOUND('',#3768,.T.);
#1419=FACE_BOUND('',#3769,.T.);
#1420=FACE_BOUND('',#3770,.T.);
#1421=FACE_BOUND('',#3771,.T.);
#1422=FACE_BOUND('',#3772,.T.);
#1423=FACE_BOUND('',#3773,.T.);
#1424=FACE_BOUND('',#3774,.T.);
#1425=FACE_BOUND('',#3775,.T.);
#1426=FACE_BOUND('',#3776,.T.);
#1427=FACE_BOUND('',#3777,.T.);
#1428=FACE_BOUND('',#3778,.T.);
#1429=FACE_BOUND('',#3779,.T.);
#1430=FACE_BOUND('',#3780,.T.);
#1431=FACE_BOUND('',#3781,.T.);
#1432=FACE_BOUND('',#3782,.T.);
#1433=FACE_BOUND('',#3783,.T.);
#1434=FACE_BOUND('',#3784,.T.);
#1435=FACE_BOUND('',#3785,.T.);
#1436=FACE_BOUND('',#3786,.T.);
#1437=FACE_BOUND('',#3787,.T.);
#1438=FACE_BOUND('',#3788,.T.);
#1439=FACE_BOUND('',#3801,.T.);
#1440=FACE_BOUND('',#3803,.T.);
#1441=FACE_BOUND('',#3805,.T.);
#1442=FACE_BOUND('',#3812,.T.);
#1443=FACE_BOUND('',#3815,.T.);
#1444=FACE_BOUND('',#3816,.T.);
#1445=FACE_BOUND('',#3819,.T.);
#1446=FACE_BOUND('',#3822,.T.);
#1447=FACE_BOUND('',#3825,.T.);
#1448=FACE_BOUND('',#3828,.T.);
#1449=FACE_BOUND('',#3843,.T.);
#1450=FACE_BOUND('',#3851,.T.);
#1451=FACE_BOUND('',#3854,.T.);
#1452=FACE_BOUND('',#3859,.T.);
#1453=FACE_BOUND('',#3864,.T.);
#1454=FACE_BOUND('',#3889,.T.);
#1455=FACE_BOUND('',#3892,.T.);
#1456=FACE_BOUND('',#3895,.T.);
#1457=FACE_BOUND('',#3898,.T.);
#1458=FACE_BOUND('',#3901,.T.);
#1459=FACE_BOUND('',#3908,.T.);
#1460=FACE_BOUND('',#3911,.T.);
#1461=FACE_BOUND('',#3916,.T.);
#1462=FACE_BOUND('',#3921,.T.);
#1463=FACE_BOUND('',#3949,.T.);
#1464=FACE_BOUND('',#3952,.T.);
#1465=FACE_BOUND('',#3955,.T.);
#1466=FACE_BOUND('',#3958,.T.);
#1467=FACE_BOUND('',#3961,.T.);
#1468=FACE_BOUND('',#3965,.T.);
#1469=FACE_BOUND('',#3972,.T.);
#1470=FACE_BOUND('',#3997,.T.);
#1471=FACE_BOUND('',#4046,.T.);
#1472=FACE_BOUND('',#4048,.T.);
#1473=FACE_BOUND('',#4054,.T.);
#1474=FACE_BOUND('',#4070,.T.);
#1475=FACE_BOUND('',#4083,.T.);
#1476=FACE_BOUND('',#4089,.T.);
#1477=FACE_BOUND('',#4122,.T.);
#1478=FACE_BOUND('',#4123,.T.);
#1479=FACE_BOUND('',#4124,.T.);
#1480=FACE_BOUND('',#4125,.T.);
#1481=FACE_BOUND('',#4126,.T.);
#1482=FACE_BOUND('',#4127,.T.);
#1483=FACE_BOUND('',#4128,.T.);
#1484=FACE_BOUND('',#4129,.T.);
#1485=FACE_BOUND('',#4130,.T.);
#1486=FACE_BOUND('',#4131,.T.);
#1487=FACE_BOUND('',#4132,.T.);
#1488=FACE_BOUND('',#4133,.T.);
#1489=FACE_BOUND('',#4134,.T.);
#1490=FACE_BOUND('',#4135,.T.);
#1491=FACE_BOUND('',#4136,.T.);
#1492=FACE_BOUND('',#4137,.T.);
#1493=FACE_BOUND('',#4138,.T.);
#1494=FACE_BOUND('',#4139,.T.);
#1495=FACE_BOUND('',#4141,.T.);
#1496=FACE_BOUND('',#4142,.T.);
#1497=FACE_BOUND('',#4143,.T.);
#1498=FACE_BOUND('',#4144,.T.);
#1499=FACE_BOUND('',#4145,.T.);
#1500=FACE_BOUND('',#4146,.T.);
#1501=FACE_BOUND('',#4147,.T.);
#1502=FACE_BOUND('',#4148,.T.);
#1503=FACE_BOUND('',#4149,.T.);
#1504=FACE_BOUND('',#4150,.T.);
#1505=FACE_BOUND('',#4151,.T.);
#1506=FACE_BOUND('',#4152,.T.);
#1507=FACE_BOUND('',#4153,.T.);
#1508=FACE_BOUND('',#4154,.T.);
#1509=FACE_BOUND('',#4155,.T.);
#1510=FACE_BOUND('',#4156,.T.);
#1511=FACE_BOUND('',#4157,.T.);
#1512=FACE_BOUND('',#4158,.T.);
#1513=FACE_BOUND('',#4170,.T.);
#1514=FACE_BOUND('',#4172,.T.);
#1515=FACE_BOUND('',#4176,.T.);
#1516=FACE_BOUND('',#4177,.T.);
#1517=FACE_BOUND('',#4178,.T.);
#1518=FACE_BOUND('',#4179,.T.);
#1519=FACE_BOUND('',#4180,.T.);
#1520=FACE_BOUND('',#4182,.T.);
#1521=FACE_BOUND('',#4194,.T.);
#1522=FACE_BOUND('',#4196,.T.);
#1523=FACE_BOUND('',#4200,.T.);
#1524=FACE_BOUND('',#4201,.T.);
#1525=FACE_BOUND('',#4202,.T.);
#1526=FACE_BOUND('',#4203,.T.);
#1527=FACE_BOUND('',#4204,.T.);
#1528=FACE_BOUND('',#4206,.T.);
#1529=FACE_BOUND('',#4216,.T.);
#1530=FACE_BOUND('',#4217,.T.);
#1531=FACE_BOUND('',#4218,.T.);
#1532=FACE_BOUND('',#4219,.T.);
#1533=FACE_BOUND('',#4221,.T.);
#1534=FACE_BOUND('',#4226,.T.);
#1535=FACE_BOUND('',#4227,.T.);
#1536=FACE_BOUND('',#4229,.T.);
#1537=FACE_BOUND('',#4230,.T.);
#1538=FACE_BOUND('',#4238,.T.);
#1539=FACE_BOUND('',#4239,.T.);
#1540=FACE_BOUND('',#4247,.T.);
#1541=FACE_BOUND('',#4248,.T.);
#1542=FACE_BOUND('',#4256,.T.);
#1543=FACE_BOUND('',#4259,.T.);
#1544=FACE_BOUND('',#4262,.T.);
#1545=FACE_BOUND('',#4265,.T.);
#1546=FACE_BOUND('',#4268,.T.);
#1547=FACE_BOUND('',#4271,.T.);
#1548=FACE_BOUND('',#4273,.T.);
#1549=FACE_BOUND('',#4279,.T.);
#1550=FACE_BOUND('',#4281,.T.);
#1551=FACE_BOUND('',#4283,.T.);
#1552=FACE_BOUND('',#4285,.T.);
#1553=FACE_BOUND('',#4308,.T.);
#1554=FACE_BOUND('',#4309,.T.);
#1555=FACE_BOUND('',#4310,.T.);
#1556=FACE_BOUND('',#4311,.T.);
#1557=FACE_BOUND('',#4317,.T.);
#1558=FACE_BOUND('',#4318,.T.);
#1559=FACE_BOUND('',#4319,.T.);
#1560=FACE_BOUND('',#4320,.T.);
#1561=FACE_BOUND('',#4325,.T.);
#1562=FACE_BOUND('',#4335,.T.);
#1563=FACE_BOUND('',#4343,.T.);
#1564=FACE_BOUND('',#4351,.T.);
#1565=FACE_BOUND('',#4491,.T.);
#1566=FACE_BOUND('',#4503,.T.);
#1567=FACE_BOUND('',#4506,.T.);
#1568=FACE_BOUND('',#4509,.T.);
#1569=FACE_BOUND('',#4514,.T.);
#1570=FACE_BOUND('',#4516,.T.);
#1571=FACE_BOUND('',#4521,.T.);
#1572=FACE_BOUND('',#4523,.T.);
#1573=FACE_BOUND('',#4525,.T.);
#1574=FACE_BOUND('',#4527,.T.);
#1575=FACE_BOUND('',#4536,.T.);
#1576=FACE_BOUND('',#4537,.T.);
#1577=FACE_BOUND('',#4539,.T.);
#1578=FACE_BOUND('',#4540,.T.);
#1579=FACE_BOUND('',#4543,.T.);
#1580=FACE_BOUND('',#4545,.T.);
#1581=FACE_BOUND('',#4550,.T.);
#1582=FACE_BOUND('',#4552,.T.);
#1583=FACE_BOUND('',#4556,.T.);
#1584=FACE_BOUND('',#4558,.T.);
#1585=FACE_BOUND('',#4577,.T.);
#1586=FACE_BOUND('',#4585,.T.);
#1587=FACE_BOUND('',#4587,.T.);
#1588=FACE_BOUND('',#4593,.T.);
#1589=PLANE('',#19290);
#1590=PLANE('',#19291);
#1591=PLANE('',#19292);
#1592=PLANE('',#19293);
#1593=PLANE('',#19294);
#1594=PLANE('',#19298);
#1595=PLANE('',#19302);
#1596=PLANE('',#19306);
#1597=PLANE('',#19310);
#1598=PLANE('',#19356);
#1599=PLANE('',#19357);
#1600=PLANE('',#19358);
#1601=PLANE('',#19359);
#1602=PLANE('',#19360);
#1603=PLANE('',#19362);
#1604=PLANE('',#19363);
#1605=PLANE('',#19364);
#1606=PLANE('',#19365);
#1607=PLANE('',#19366);
#1608=PLANE('',#19367);
#1609=PLANE('',#19369);
#1610=PLANE('',#19370);
#1611=PLANE('',#19371);
#1612=PLANE('',#19372);
#1613=PLANE('',#19373);
#1614=PLANE('',#19374);
#1615=PLANE('',#19400);
#1616=PLANE('',#19401);
#1617=PLANE('',#19402);
#1618=PLANE('',#19403);
#1619=PLANE('',#19410);
#1620=PLANE('',#19411);
#1621=PLANE('',#19412);
#1622=PLANE('',#19413);
#1623=PLANE('',#19414);
#1624=PLANE('',#19415);
#1625=PLANE('',#19426);
#1626=PLANE('',#19430);
#1627=PLANE('',#19434);
#1628=PLANE('',#19438);
#1629=PLANE('',#19439);
#1630=PLANE('',#19440);
#1631=PLANE('',#19441);
#1632=PLANE('',#19442);
#1633=PLANE('',#19443);
#1634=PLANE('',#19444);
#1635=PLANE('',#19455);
#1636=PLANE('',#19459);
#1637=PLANE('',#19463);
#1638=PLANE('',#19467);
#1639=PLANE('',#19468);
#1640=PLANE('',#19469);
#1641=PLANE('',#19470);
#1642=PLANE('',#19471);
#1643=PLANE('',#19472);
#1644=PLANE('',#19473);
#1645=PLANE('',#19478);
#1646=PLANE('',#19482);
#1647=PLANE('',#19489);
#1648=PLANE('',#19490);
#1649=PLANE('',#19491);
#1650=PLANE('',#19492);
#1651=PLANE('',#19493);
#1652=PLANE('',#19494);
#1653=PLANE('',#19507);
#1654=PLANE('',#19513);
#1655=PLANE('',#19514);
#1656=PLANE('',#19515);
#1657=PLANE('',#19516);
#1658=PLANE('',#19517);
#1659=PLANE('',#19518);
#1660=PLANE('',#19519);
#1661=PLANE('',#19520);
#1662=PLANE('',#19521);
#1663=PLANE('',#19526);
#1664=PLANE('',#19530);
#1665=PLANE('',#19537);
#1666=PLANE('',#19538);
#1667=PLANE('',#19539);
#1668=PLANE('',#19540);
#1669=PLANE('',#19541);
#1670=PLANE('',#19542);
#1671=PLANE('',#19555);
#1672=PLANE('',#19561);
#1673=PLANE('',#19562);
#1674=PLANE('',#19563);
#1675=PLANE('',#19564);
#1676=PLANE('',#19565);
#1677=PLANE('',#19566);
#1678=PLANE('',#19567);
#1679=PLANE('',#19568);
#1680=PLANE('',#19569);
#1681=PLANE('',#19583);
#1682=PLANE('',#19587);
#1683=PLANE('',#19591);
#1684=PLANE('',#19595);
#1685=PLANE('',#19599);
#1686=PLANE('',#19606);
#1687=PLANE('',#19607);
#1688=PLANE('',#19608);
#1689=PLANE('',#19609);
#1690=PLANE('',#19610);
#1691=PLANE('',#19611);
#1692=PLANE('',#19612);
#1693=PLANE('',#19632);
#1694=PLANE('',#19636);
#1695=PLANE('',#19640);
#1696=PLANE('',#19644);
#1697=PLANE('',#19648);
#1698=PLANE('',#19658);
#1699=PLANE('',#19659);
#1700=PLANE('',#19660);
#1701=PLANE('',#19661);
#1702=PLANE('',#19662);
#1703=PLANE('',#19663);
#1704=PLANE('',#19677);
#1705=PLANE('',#19684);
#1706=PLANE('',#19685);
#1707=PLANE('',#19699);
#1708=PLANE('',#19706);
#1709=PLANE('',#19707);
#1710=PLANE('',#19712);
#1711=PLANE('',#19716);
#1712=PLANE('',#19717);
#1713=PLANE('',#19722);
#1714=PLANE('',#19726);
#1715=PLANE('',#19727);
#1716=PLANE('',#19732);
#1717=PLANE('',#19736);
#1718=PLANE('',#19737);
#1719=PLANE('',#19742);
#1720=PLANE('',#19746);
#1721=PLANE('',#19747);
#1722=PLANE('',#19752);
#1723=PLANE('',#19757);
#1724=PLANE('',#19762);
#1725=PLANE('',#19767);
#1726=PLANE('',#19780);
#1727=PLANE('',#19781);
#1728=PLANE('',#19783);
#1729=PLANE('',#19784);
#1730=PLANE('',#19785);
#1731=PLANE('',#19786);
#1732=PLANE('',#19787);
#1733=PLANE('',#19788);
#1734=PLANE('',#19789);
#1735=PLANE('',#19790);
#1736=PLANE('',#19791);
#1737=PLANE('',#19792);
#1738=PLANE('',#19793);
#1739=PLANE('',#19794);
#1740=PLANE('',#19795);
#1741=PLANE('',#19796);
#1742=PLANE('',#19797);
#1743=PLANE('',#19798);
#1744=PLANE('',#19799);
#1745=PLANE('',#19800);
#1746=PLANE('',#19801);
#1747=PLANE('',#19802);
#1748=PLANE('',#19803);
#1749=PLANE('',#19804);
#1750=PLANE('',#19805);
#1751=PLANE('',#19806);
#1752=PLANE('',#19807);
#1753=PLANE('',#19808);
#1754=PLANE('',#19809);
#1755=PLANE('',#19810);
#1756=PLANE('',#19811);
#1757=PLANE('',#19812);
#1758=PLANE('',#19813);
#1759=PLANE('',#19814);
#1760=PLANE('',#19815);
#1761=PLANE('',#19816);
#1762=PLANE('',#19817);
#1763=PLANE('',#19818);
#1764=PLANE('',#19819);
#1765=PLANE('',#19820);
#1766=PLANE('',#19821);
#1767=PLANE('',#19822);
#1768=PLANE('',#19823);
#1769=PLANE('',#19824);
#1770=PLANE('',#19825);
#1771=PLANE('',#19826);
#1772=PLANE('',#19827);
#1773=PLANE('',#19828);
#1774=PLANE('',#19829);
#1775=PLANE('',#19830);
#1776=PLANE('',#19831);
#1777=PLANE('',#19832);
#1778=PLANE('',#19833);
#1779=PLANE('',#19834);
#1780=PLANE('',#19835);
#1781=PLANE('',#19836);
#1782=PLANE('',#19837);
#1783=PLANE('',#19838);
#1784=PLANE('',#19839);
#1785=PLANE('',#19840);
#1786=PLANE('',#19841);
#1787=PLANE('',#19842);
#1788=PLANE('',#19843);
#1789=PLANE('',#19844);
#1790=PLANE('',#19845);
#1791=PLANE('',#19846);
#1792=PLANE('',#19847);
#1793=PLANE('',#19848);
#1794=PLANE('',#19849);
#1795=PLANE('',#19850);
#1796=PLANE('',#19851);
#1797=PLANE('',#19852);
#1798=PLANE('',#19853);
#1799=PLANE('',#19854);
#1800=PLANE('',#19855);
#1801=PLANE('',#19856);
#1802=PLANE('',#19857);
#1803=PLANE('',#19858);
#1804=PLANE('',#19859);
#1805=PLANE('',#19860);
#1806=PLANE('',#19861);
#1807=PLANE('',#19862);
#1808=PLANE('',#19863);
#1809=PLANE('',#19864);
#1810=PLANE('',#19865);
#1811=PLANE('',#19866);
#1812=PLANE('',#19867);
#1813=PLANE('',#19868);
#1814=PLANE('',#19869);
#1815=PLANE('',#19870);
#1816=PLANE('',#19871);
#1817=PLANE('',#19872);
#1818=PLANE('',#19873);
#1819=PLANE('',#19874);
#1820=PLANE('',#19875);
#1821=PLANE('',#19876);
#1822=PLANE('',#19877);
#1823=PLANE('',#19878);
#1824=PLANE('',#19879);
#1825=PLANE('',#19880);
#1826=PLANE('',#19881);
#1827=PLANE('',#19882);
#1828=PLANE('',#19883);
#1829=PLANE('',#19884);
#1830=PLANE('',#19885);
#1831=PLANE('',#19886);
#1832=PLANE('',#19887);
#1833=PLANE('',#19888);
#1834=PLANE('',#19889);
#1835=PLANE('',#19890);
#1836=PLANE('',#19891);
#1837=PLANE('',#19892);
#1838=PLANE('',#19893);
#1839=PLANE('',#19894);
#1840=PLANE('',#19895);
#1841=PLANE('',#19896);
#1842=PLANE('',#19897);
#1843=PLANE('',#19898);
#1844=PLANE('',#19899);
#1845=PLANE('',#19900);
#1846=PLANE('',#19901);
#1847=PLANE('',#19902);
#1848=PLANE('',#19903);
#1849=PLANE('',#19904);
#1850=PLANE('',#19905);
#1851=PLANE('',#19906);
#1852=PLANE('',#19907);
#1853=PLANE('',#19914);
#1854=PLANE('',#19915);
#1855=PLANE('',#19916);
#1856=PLANE('',#19917);
#1857=PLANE('',#19918);
#1858=PLANE('',#19919);
#1859=PLANE('',#19926);
#1860=PLANE('',#19929);
#1861=PLANE('',#19931);
#1862=PLANE('',#19938);
#1863=PLANE('',#19939);
#1864=PLANE('',#19941);
#1865=PLANE('',#19943);
#1866=PLANE('',#19957);
#1867=PLANE('',#19958);
#1868=PLANE('',#19959);
#1869=PLANE('',#19960);
#1870=PLANE('',#19961);
#1871=PLANE('',#19962);
#1872=PLANE('',#19963);
#1873=PLANE('',#19964);
#1874=PLANE('',#19965);
#1875=PLANE('',#19966);
#1876=PLANE('',#19967);
#1877=PLANE('',#19969);
#1878=PLANE('',#19970);
#1879=PLANE('',#19971);
#1880=PLANE('',#19972);
#1881=PLANE('',#19973);
#1882=PLANE('',#19974);
#1883=PLANE('',#19975);
#1884=PLANE('',#19976);
#1885=PLANE('',#19977);
#1886=PLANE('',#19979);
#1887=PLANE('',#19987);
#1888=PLANE('',#20007);
#1889=PLANE('',#20010);
#1890=PLANE('',#20022);
#1891=PLANE('',#20031);
#1892=PLANE('',#20062);
#1893=PLANE('',#20067);
#1894=PLANE('',#20072);
#1895=PLANE('',#20078);
#1896=PLANE('',#20083);
#1897=PLANE('',#20092);
#1898=PLANE('',#20096);
#1899=PLANE('',#20097);
#1900=PLANE('',#20099);
#1901=PLANE('',#20104);
#1902=PLANE('',#20107);
#1903=PLANE('',#20112);
#1904=PLANE('',#20135);
#1905=PLANE('',#20138);
#1906=PLANE('',#20150);
#1907=PLANE('',#20159);
#1908=PLANE('',#20192);
#1909=PLANE('',#20197);
#1910=PLANE('',#20202);
#1911=PLANE('',#20207);
#1912=PLANE('',#20212);
#1913=PLANE('',#20217);
#1914=PLANE('',#20226);
#1915=PLANE('',#20230);
#1916=PLANE('',#20231);
#1917=PLANE('',#20233);
#1918=PLANE('',#20238);
#1919=PLANE('',#20241);
#1920=PLANE('',#20246);
#1921=PLANE('',#20255);
#1922=PLANE('',#20257);
#1923=PLANE('',#20261);
#1924=PLANE('',#20269);
#1925=PLANE('',#20274);
#1926=PLANE('',#20275);
#1927=PLANE('',#20276);
#1928=PLANE('',#20277);
#1929=PLANE('',#20278);
#1930=PLANE('',#20279);
#1931=PLANE('',#20280);
#1932=PLANE('',#20281);
#1933=PLANE('',#20283);
#1934=PLANE('',#20284);
#1935=PLANE('',#20285);
#1936=PLANE('',#20286);
#1937=PLANE('',#20287);
#1938=PLANE('',#20288);
#1939=PLANE('',#20289);
#1940=PLANE('',#20290);
#1941=PLANE('',#20291);
#1942=PLANE('',#20293);
#1943=PLANE('',#20301);
#1944=PLANE('',#20307);
#1945=PLANE('',#20308);
#1946=PLANE('',#20309);
#1947=PLANE('',#20310);
#1948=PLANE('',#20311);
#1949=PLANE('',#20312);
#1950=PLANE('',#20313);
#1951=PLANE('',#20314);
#1952=PLANE('',#20315);
#1953=PLANE('',#20316);
#1954=PLANE('',#20317);
#1955=PLANE('',#20318);
#1956=PLANE('',#20319);
#1957=PLANE('',#20320);
#1958=PLANE('',#20321);
#1959=PLANE('',#20322);
#1960=PLANE('',#20323);
#1961=PLANE('',#20324);
#1962=PLANE('',#20325);
#1963=PLANE('',#20326);
#1964=PLANE('',#20327);
#1965=PLANE('',#20328);
#1966=PLANE('',#20329);
#1967=PLANE('',#20330);
#1968=PLANE('',#20331);
#1969=PLANE('',#20332);
#1970=PLANE('',#20333);
#1971=PLANE('',#20334);
#1972=PLANE('',#20335);
#1973=PLANE('',#20336);
#1974=PLANE('',#20337);
#1975=PLANE('',#20338);
#1976=PLANE('',#20339);
#1977=PLANE('',#20340);
#1978=PLANE('',#20341);
#1979=PLANE('',#20342);
#1980=PLANE('',#20346);
#1981=PLANE('',#20347);
#1982=PLANE('',#20348);
#1983=PLANE('',#20349);
#1984=PLANE('',#20350);
#1985=PLANE('',#20351);
#1986=PLANE('',#20352);
#1987=PLANE('',#20353);
#1988=PLANE('',#20354);
#1989=PLANE('',#20355);
#1990=PLANE('',#20357);
#1991=PLANE('',#20365);
#1992=PLANE('',#20373);
#1993=PLANE('',#20374);
#1994=PLANE('',#20375);
#1995=PLANE('',#20376);
#1996=PLANE('',#20377);
#1997=PLANE('',#20378);
#1998=PLANE('',#20379);
#1999=PLANE('',#20380);
#2000=PLANE('',#20381);
#2001=PLANE('',#20383);
#2002=PLANE('',#20384);
#2003=PLANE('',#20385);
#2004=PLANE('',#20387);
#2005=PLANE('',#20388);
#2006=PLANE('',#20389);
#2007=PLANE('',#20390);
#2008=PLANE('',#20391);
#2009=PLANE('',#20392);
#2010=PLANE('',#20399);
#2011=PLANE('',#20400);
#2012=PLANE('',#20401);
#2013=PLANE('',#20402);
#2014=PLANE('',#20404);
#2015=PLANE('',#20406);
#2016=PLANE('',#20414);
#2017=PLANE('',#20419);
#2018=PLANE('',#20420);
#2019=PLANE('',#20421);
#2020=PLANE('',#20422);
#2021=PLANE('',#20423);
#2022=PLANE('',#20424);
#2023=PLANE('',#20425);
#2024=PLANE('',#20482);
#2025=PLANE('',#20483);
#2026=PLANE('',#20484);
#2027=PLANE('',#20485);
#2028=PLANE('',#20486);
#2029=PLANE('',#20487);
#2030=PLANE('',#20489);
#2031=PLANE('',#20496);
#2032=PLANE('',#20503);
#2033=PLANE('',#20510);
#2034=PLANE('',#20527);
#2035=PLANE('',#20529);
#2036=PLANE('',#20535);
#2037=PLANE('',#20536);
#2038=PLANE('',#20538);
#2039=PLANE('',#20545);
#2040=PLANE('',#20552);
#2041=PLANE('',#20559);
#2042=PLANE('',#20576);
#2043=PLANE('',#20578);
#2044=PLANE('',#20584);
#2045=PLANE('',#20585);
#2046=PLANE('',#20590);
#2047=PLANE('',#20594);
#2048=PLANE('',#20598);
#2049=PLANE('',#20605);
#2050=PLANE('',#20606);
#2051=PLANE('',#20617);
#2052=PLANE('',#20618);
#2053=PLANE('',#20626);
#2054=PLANE('',#20627);
#2055=PLANE('',#20628);
#2056=PLANE('',#20629);
#2057=PLANE('',#20630);
#2058=PLANE('',#20631);
#2059=PLANE('',#20632);
#2060=PLANE('',#20633);
#2061=PLANE('',#20634);
#2062=PLANE('',#20635);
#2063=PLANE('',#20636);
#2064=PLANE('',#20637);
#2065=PLANE('',#20638);
#2066=PLANE('',#20641);
#2067=PLANE('',#20643);
#2068=PLANE('',#20644);
#2069=PLANE('',#20646);
#2070=PLANE('',#20647);
#2071=PLANE('',#20648);
#2072=PLANE('',#20653);
#2073=PLANE('',#20657);
#2074=PLANE('',#20661);
#2075=PLANE('',#20665);
#2076=PLANE('',#20669);
#2077=PLANE('',#20673);
#2078=PLANE('',#20676);
#2079=PLANE('',#20677);
#2080=PLANE('',#20680);
#2081=PLANE('',#20681);
#2082=PLANE('',#20686);
#2083=PLANE('',#20715);
#2084=PLANE('',#20727);
#2085=PLANE('',#20728);
#2086=PLANE('',#20735);
#2087=PLANE('',#20737);
#2088=PLANE('',#20738);
#2089=PLANE('',#20739);
#2090=PLANE('',#20740);
#2091=PLANE('',#20741);
#2092=PLANE('',#20742);
#2093=PLANE('',#20743);
#2094=PLANE('',#20744);
#2095=PLANE('',#20745);
#2096=PLANE('',#20750);
#2097=PLANE('',#20751);
#2098=PLANE('',#20759);
#2099=PLANE('',#20765);
#2100=PLANE('',#20773);
#2101=PLANE('',#20781);
#2102=PLANE('',#20782);
#2103=PLANE('',#20783);
#2104=PLANE('',#20784);
#2105=PLANE('',#20785);
#2106=PLANE('',#20786);
#2107=PLANE('',#20787);
#2108=PLANE('',#20788);
#2109=PLANE('',#20789);
#2110=PLANE('',#21029);
#2111=PLANE('',#21034);
#2112=PLANE('',#21036);
#2113=PLANE('',#21037);
#2114=PLANE('',#21039);
#2115=PLANE('',#21040);
#2116=PLANE('',#21041);
#2117=PLANE('',#21046);
#2118=PLANE('',#21047);
#2119=PLANE('',#21052);
#2120=PLANE('',#21061);
#2121=PLANE('',#21062);
#2122=PLANE('',#21064);
#2123=PLANE('',#21068);
#2124=PLANE('',#21075);
#2125=PLANE('',#21076);
#2126=PLANE('',#21081);
#2127=PLANE('',#21085);
#2128=PLANE('',#21086);
#2129=PLANE('',#21087);
#2130=PLANE('',#21088);
#2131=PLANE('',#21089);
#2132=PLANE('',#21092);
#2133=PLANE('',#21100);
#2134=PLANE('',#21108);
#2135=PLANE('',#21109);
#2136=PLANE('',#21117);
#2137=PLANE('',#21118);
#2138=PLANE('',#21120);
#2139=PLANE('',#21121);
#2140=PLANE('',#21122);
#2141=PLANE('',#21123);
#2142=PLANE('',#21124);
#2143=PLANE('',#21125);
#2144=PLANE('',#21126);
#2145=PLANE('',#21127);
#2146=PLANE('',#21128);
#2147=PLANE('',#21129);
#2148=PLANE('',#21131);
#2149=PLANE('',#21132);
#2150=PLANE('',#21133);
#2151=PLANE('',#21134);
#2152=PLANE('',#21135);
#2153=PLANE('',#21136);
#2154=PLANE('',#21137);
#2155=PLANE('',#21138);
#2156=PLANE('',#21146);
#2157=PLANE('',#21154);
#2158=PLANE('',#21155);
#2159=PLANE('',#21157);
#2160=PLANE('',#21165);
#2161=PLANE('',#21173);
#2162=PLANE('',#21174);
#2163=PLANE('',#21175);
#2164=PLANE('',#21176);
#2165=PLANE('',#21177);
#2166=PLANE('',#21178);
#2167=PLANE('',#21179);
#2168=PLANE('',#21180);
#2169=PLANE('',#21181);
#2170=FACE_OUTER_BOUND('',#3217,.T.);
#2171=FACE_OUTER_BOUND('',#3218,.T.);
#2172=FACE_OUTER_BOUND('',#3219,.T.);
#2173=FACE_OUTER_BOUND('',#3220,.T.);
#2174=FACE_OUTER_BOUND('',#3221,.T.);
#2175=FACE_OUTER_BOUND('',#3222,.T.);
#2176=FACE_OUTER_BOUND('',#3223,.T.);
#2177=FACE_OUTER_BOUND('',#3224,.T.);
#2178=FACE_OUTER_BOUND('',#3225,.T.);
#2179=FACE_OUTER_BOUND('',#3226,.T.);
#2180=FACE_OUTER_BOUND('',#3227,.T.);
#2181=FACE_OUTER_BOUND('',#3228,.T.);
#2182=FACE_OUTER_BOUND('',#3229,.T.);
#2183=FACE_OUTER_BOUND('',#3230,.T.);
#2184=FACE_OUTER_BOUND('',#3231,.T.);
#2185=FACE_OUTER_BOUND('',#3232,.T.);
#2186=FACE_OUTER_BOUND('',#3233,.T.);
#2187=FACE_OUTER_BOUND('',#3234,.T.);
#2188=FACE_OUTER_BOUND('',#3235,.T.);
#2189=FACE_OUTER_BOUND('',#3236,.T.);
#2190=FACE_OUTER_BOUND('',#3237,.T.);
#2191=FACE_OUTER_BOUND('',#3238,.T.);
#2192=FACE_OUTER_BOUND('',#3239,.T.);
#2193=FACE_OUTER_BOUND('',#3240,.T.);
#2194=FACE_OUTER_BOUND('',#3241,.T.);
#2195=FACE_OUTER_BOUND('',#3242,.T.);
#2196=FACE_OUTER_BOUND('',#3243,.T.);
#2197=FACE_OUTER_BOUND('',#3244,.T.);
#2198=FACE_OUTER_BOUND('',#3245,.T.);
#2199=FACE_OUTER_BOUND('',#3246,.T.);
#2200=FACE_OUTER_BOUND('',#3247,.T.);
#2201=FACE_OUTER_BOUND('',#3248,.T.);
#2202=FACE_OUTER_BOUND('',#3249,.T.);
#2203=FACE_OUTER_BOUND('',#3270,.T.);
#2204=FACE_OUTER_BOUND('',#3287,.T.);
#2205=FACE_OUTER_BOUND('',#3288,.T.);
#2206=FACE_OUTER_BOUND('',#3289,.T.);
#2207=FACE_OUTER_BOUND('',#3290,.T.);
#2208=FACE_OUTER_BOUND('',#3291,.T.);
#2209=FACE_OUTER_BOUND('',#3292,.T.);
#2210=FACE_OUTER_BOUND('',#3293,.T.);
#2211=FACE_OUTER_BOUND('',#3294,.T.);
#2212=FACE_OUTER_BOUND('',#3295,.T.);
#2213=FACE_OUTER_BOUND('',#3296,.T.);
#2214=FACE_OUTER_BOUND('',#3297,.T.);
#2215=FACE_OUTER_BOUND('',#3298,.T.);
#2216=FACE_OUTER_BOUND('',#3299,.T.);
#2217=FACE_OUTER_BOUND('',#3300,.T.);
#2218=FACE_OUTER_BOUND('',#3301,.T.);
#2219=FACE_OUTER_BOUND('',#3302,.T.);
#2220=FACE_OUTER_BOUND('',#3303,.T.);
#2221=FACE_OUTER_BOUND('',#3304,.T.);
#2222=FACE_OUTER_BOUND('',#3305,.T.);
#2223=FACE_OUTER_BOUND('',#3306,.T.);
#2224=FACE_OUTER_BOUND('',#3307,.T.);
#2225=FACE_OUTER_BOUND('',#3308,.T.);
#2226=FACE_OUTER_BOUND('',#3309,.T.);
#2227=FACE_OUTER_BOUND('',#3310,.T.);
#2228=FACE_OUTER_BOUND('',#3311,.T.);
#2229=FACE_OUTER_BOUND('',#3312,.T.);
#2230=FACE_OUTER_BOUND('',#3313,.T.);
#2231=FACE_OUTER_BOUND('',#3314,.T.);
#2232=FACE_OUTER_BOUND('',#3315,.T.);
#2233=FACE_OUTER_BOUND('',#3316,.T.);
#2234=FACE_OUTER_BOUND('',#3317,.T.);
#2235=FACE_OUTER_BOUND('',#3329,.T.);
#2236=FACE_OUTER_BOUND('',#3341,.T.);
#2237=FACE_OUTER_BOUND('',#3342,.T.);
#2238=FACE_OUTER_BOUND('',#3343,.T.);
#2239=FACE_OUTER_BOUND('',#3344,.T.);
#2240=FACE_OUTER_BOUND('',#3345,.T.);
#2241=FACE_OUTER_BOUND('',#3346,.T.);
#2242=FACE_OUTER_BOUND('',#3347,.T.);
#2243=FACE_OUTER_BOUND('',#3348,.T.);
#2244=FACE_OUTER_BOUND('',#3349,.T.);
#2245=FACE_OUTER_BOUND('',#3350,.T.);
#2246=FACE_OUTER_BOUND('',#3351,.T.);
#2247=FACE_OUTER_BOUND('',#3352,.T.);
#2248=FACE_OUTER_BOUND('',#3355,.T.);
#2249=FACE_OUTER_BOUND('',#3356,.T.);
#2250=FACE_OUTER_BOUND('',#3359,.T.);
#2251=FACE_OUTER_BOUND('',#3362,.T.);
#2252=FACE_OUTER_BOUND('',#3365,.T.);
#2253=FACE_OUTER_BOUND('',#3366,.T.);
#2254=FACE_OUTER_BOUND('',#3367,.T.);
#2255=FACE_OUTER_BOUND('',#3368,.T.);
#2256=FACE_OUTER_BOUND('',#3369,.T.);
#2257=FACE_OUTER_BOUND('',#3370,.T.);
#2258=FACE_OUTER_BOUND('',#3371,.T.);
#2259=FACE_OUTER_BOUND('',#3372,.T.);
#2260=FACE_OUTER_BOUND('',#3373,.T.);
#2261=FACE_OUTER_BOUND('',#3374,.T.);
#2262=FACE_OUTER_BOUND('',#3375,.T.);
#2263=FACE_OUTER_BOUND('',#3376,.T.);
#2264=FACE_OUTER_BOUND('',#3379,.T.);
#2265=FACE_OUTER_BOUND('',#3380,.T.);
#2266=FACE_OUTER_BOUND('',#3383,.T.);
#2267=FACE_OUTER_BOUND('',#3386,.T.);
#2268=FACE_OUTER_BOUND('',#3389,.T.);
#2269=FACE_OUTER_BOUND('',#3390,.T.);
#2270=FACE_OUTER_BOUND('',#3391,.T.);
#2271=FACE_OUTER_BOUND('',#3392,.T.);
#2272=FACE_OUTER_BOUND('',#3393,.T.);
#2273=FACE_OUTER_BOUND('',#3394,.T.);
#2274=FACE_OUTER_BOUND('',#3395,.T.);
#2275=FACE_OUTER_BOUND('',#3398,.T.);
#2276=FACE_OUTER_BOUND('',#3399,.T.);
#2277=FACE_OUTER_BOUND('',#3402,.T.);
#2278=FACE_OUTER_BOUND('',#3403,.T.);
#2279=FACE_OUTER_BOUND('',#3404,.T.);
#2280=FACE_OUTER_BOUND('',#3407,.T.);
#2281=FACE_OUTER_BOUND('',#3408,.T.);
#2282=FACE_OUTER_BOUND('',#3409,.T.);
#2283=FACE_OUTER_BOUND('',#3410,.T.);
#2284=FACE_OUTER_BOUND('',#3411,.T.);
#2285=FACE_OUTER_BOUND('',#3412,.T.);
#2286=FACE_OUTER_BOUND('',#3413,.T.);
#2287=FACE_OUTER_BOUND('',#3414,.T.);
#2288=FACE_OUTER_BOUND('',#3417,.T.);
#2289=FACE_OUTER_BOUND('',#3418,.T.);
#2290=FACE_OUTER_BOUND('',#3419,.T.);
#2291=FACE_OUTER_BOUND('',#3422,.T.);
#2292=FACE_OUTER_BOUND('',#3423,.T.);
#2293=FACE_OUTER_BOUND('',#3426,.T.);
#2294=FACE_OUTER_BOUND('',#3427,.T.);
#2295=FACE_OUTER_BOUND('',#3428,.T.);
#2296=FACE_OUTER_BOUND('',#3429,.T.);
#2297=FACE_OUTER_BOUND('',#3430,.T.);
#2298=FACE_OUTER_BOUND('',#3431,.T.);
#2299=FACE_OUTER_BOUND('',#3432,.T.);
#2300=FACE_OUTER_BOUND('',#3433,.T.);
#2301=FACE_OUTER_BOUND('',#3436,.T.);
#2302=FACE_OUTER_BOUND('',#3437,.T.);
#2303=FACE_OUTER_BOUND('',#3440,.T.);
#2304=FACE_OUTER_BOUND('',#3441,.T.);
#2305=FACE_OUTER_BOUND('',#3442,.T.);
#2306=FACE_OUTER_BOUND('',#3445,.T.);
#2307=FACE_OUTER_BOUND('',#3446,.T.);
#2308=FACE_OUTER_BOUND('',#3447,.T.);
#2309=FACE_OUTER_BOUND('',#3448,.T.);
#2310=FACE_OUTER_BOUND('',#3449,.T.);
#2311=FACE_OUTER_BOUND('',#3450,.T.);
#2312=FACE_OUTER_BOUND('',#3451,.T.);
#2313=FACE_OUTER_BOUND('',#3452,.T.);
#2314=FACE_OUTER_BOUND('',#3455,.T.);
#2315=FACE_OUTER_BOUND('',#3456,.T.);
#2316=FACE_OUTER_BOUND('',#3457,.T.);
#2317=FACE_OUTER_BOUND('',#3460,.T.);
#2318=FACE_OUTER_BOUND('',#3461,.T.);
#2319=FACE_OUTER_BOUND('',#3464,.T.);
#2320=FACE_OUTER_BOUND('',#3465,.T.);
#2321=FACE_OUTER_BOUND('',#3466,.T.);
#2322=FACE_OUTER_BOUND('',#3467,.T.);
#2323=FACE_OUTER_BOUND('',#3468,.T.);
#2324=FACE_OUTER_BOUND('',#3469,.T.);
#2325=FACE_OUTER_BOUND('',#3470,.T.);
#2326=FACE_OUTER_BOUND('',#3471,.T.);
#2327=FACE_OUTER_BOUND('',#3472,.T.);
#2328=FACE_OUTER_BOUND('',#3473,.T.);
#2329=FACE_OUTER_BOUND('',#3474,.T.);
#2330=FACE_OUTER_BOUND('',#3475,.T.);
#2331=FACE_OUTER_BOUND('',#3476,.T.);
#2332=FACE_OUTER_BOUND('',#3477,.T.);
#2333=FACE_OUTER_BOUND('',#3479,.T.);
#2334=FACE_OUTER_BOUND('',#3480,.T.);
#2335=FACE_OUTER_BOUND('',#3481,.T.);
#2336=FACE_OUTER_BOUND('',#3486,.T.);
#2337=FACE_OUTER_BOUND('',#3487,.T.);
#2338=FACE_OUTER_BOUND('',#3488,.T.);
#2339=FACE_OUTER_BOUND('',#3489,.T.);
#2340=FACE_OUTER_BOUND('',#3490,.T.);
#2341=FACE_OUTER_BOUND('',#3495,.T.);
#2342=FACE_OUTER_BOUND('',#3501,.T.);
#2343=FACE_OUTER_BOUND('',#3502,.T.);
#2344=FACE_OUTER_BOUND('',#3503,.T.);
#2345=FACE_OUTER_BOUND('',#3504,.T.);
#2346=FACE_OUTER_BOUND('',#3505,.T.);
#2347=FACE_OUTER_BOUND('',#3506,.T.);
#2348=FACE_OUTER_BOUND('',#3507,.T.);
#2349=FACE_OUTER_BOUND('',#3508,.T.);
#2350=FACE_OUTER_BOUND('',#3509,.T.);
#2351=FACE_OUTER_BOUND('',#3510,.T.);
#2352=FACE_OUTER_BOUND('',#3511,.T.);
#2353=FACE_OUTER_BOUND('',#3512,.T.);
#2354=FACE_OUTER_BOUND('',#3513,.T.);
#2355=FACE_OUTER_BOUND('',#3514,.T.);
#2356=FACE_OUTER_BOUND('',#3515,.T.);
#2357=FACE_OUTER_BOUND('',#3517,.T.);
#2358=FACE_OUTER_BOUND('',#3518,.T.);
#2359=FACE_OUTER_BOUND('',#3519,.T.);
#2360=FACE_OUTER_BOUND('',#3520,.T.);
#2361=FACE_OUTER_BOUND('',#3523,.T.);
#2362=FACE_OUTER_BOUND('',#3530,.T.);
#2363=FACE_OUTER_BOUND('',#3531,.T.);
#2364=FACE_OUTER_BOUND('',#3532,.T.);
#2365=FACE_OUTER_BOUND('',#3535,.T.);
#2366=FACE_OUTER_BOUND('',#3542,.T.);
#2367=FACE_OUTER_BOUND('',#3543,.T.);
#2368=FACE_OUTER_BOUND('',#3544,.T.);
#2369=FACE_OUTER_BOUND('',#3545,.T.);
#2370=FACE_OUTER_BOUND('',#3546,.T.);
#2371=FACE_OUTER_BOUND('',#3548,.T.);
#2372=FACE_OUTER_BOUND('',#3549,.T.);
#2373=FACE_OUTER_BOUND('',#3550,.T.);
#2374=FACE_OUTER_BOUND('',#3555,.T.);
#2375=FACE_OUTER_BOUND('',#3560,.T.);
#2376=FACE_OUTER_BOUND('',#3561,.T.);
#2377=FACE_OUTER_BOUND('',#3562,.T.);
#2378=FACE_OUTER_BOUND('',#3563,.T.);
#2379=FACE_OUTER_BOUND('',#3564,.T.);
#2380=FACE_OUTER_BOUND('',#3566,.T.);
#2381=FACE_OUTER_BOUND('',#3567,.T.);
#2382=FACE_OUTER_BOUND('',#3568,.T.);
#2383=FACE_OUTER_BOUND('',#3573,.T.);
#2384=FACE_OUTER_BOUND('',#3578,.T.);
#2385=FACE_OUTER_BOUND('',#3579,.T.);
#2386=FACE_OUTER_BOUND('',#3580,.T.);
#2387=FACE_OUTER_BOUND('',#3581,.T.);
#2388=FACE_OUTER_BOUND('',#3582,.T.);
#2389=FACE_OUTER_BOUND('',#3584,.T.);
#2390=FACE_OUTER_BOUND('',#3585,.T.);
#2391=FACE_OUTER_BOUND('',#3586,.T.);
#2392=FACE_OUTER_BOUND('',#3587,.T.);
#2393=FACE_OUTER_BOUND('',#3589,.T.);
#2394=FACE_OUTER_BOUND('',#3590,.T.);
#2395=FACE_OUTER_BOUND('',#3591,.T.);
#2396=FACE_OUTER_BOUND('',#3592,.T.);
#2397=FACE_OUTER_BOUND('',#3593,.T.);
#2398=FACE_OUTER_BOUND('',#3594,.T.);
#2399=FACE_OUTER_BOUND('',#3596,.T.);
#2400=FACE_OUTER_BOUND('',#3597,.T.);
#2401=FACE_OUTER_BOUND('',#3598,.T.);
#2402=FACE_OUTER_BOUND('',#3599,.T.);
#2403=FACE_OUTER_BOUND('',#3601,.T.);
#2404=FACE_OUTER_BOUND('',#3602,.T.);
#2405=FACE_OUTER_BOUND('',#3603,.T.);
#2406=FACE_OUTER_BOUND('',#3605,.T.);
#2407=FACE_OUTER_BOUND('',#3606,.T.);
#2408=FACE_OUTER_BOUND('',#3608,.T.);
#2409=FACE_OUTER_BOUND('',#3609,.T.);
#2410=FACE_OUTER_BOUND('',#3611,.T.);
#2411=FACE_OUTER_BOUND('',#3612,.T.);
#2412=FACE_OUTER_BOUND('',#3614,.T.);
#2413=FACE_OUTER_BOUND('',#3615,.T.);
#2414=FACE_OUTER_BOUND('',#3616,.T.);
#2415=FACE_OUTER_BOUND('',#3617,.T.);
#2416=FACE_OUTER_BOUND('',#3618,.T.);
#2417=FACE_OUTER_BOUND('',#3619,.T.);
#2418=FACE_OUTER_BOUND('',#3624,.T.);
#2419=FACE_OUTER_BOUND('',#3629,.T.);
#2420=FACE_OUTER_BOUND('',#3630,.T.);
#2421=FACE_OUTER_BOUND('',#3631,.T.);
#2422=FACE_OUTER_BOUND('',#3632,.T.);
#2423=FACE_OUTER_BOUND('',#3633,.T.);
#2424=FACE_OUTER_BOUND('',#3634,.T.);
#2425=FACE_OUTER_BOUND('',#3635,.T.);
#2426=FACE_OUTER_BOUND('',#3636,.T.);
#2427=FACE_OUTER_BOUND('',#3637,.T.);
#2428=FACE_OUTER_BOUND('',#3638,.T.);
#2429=FACE_OUTER_BOUND('',#3639,.T.);
#2430=FACE_OUTER_BOUND('',#3640,.T.);
#2431=FACE_OUTER_BOUND('',#3641,.T.);
#2432=FACE_OUTER_BOUND('',#3642,.T.);
#2433=FACE_OUTER_BOUND('',#3643,.T.);
#2434=FACE_OUTER_BOUND('',#3644,.T.);
#2435=FACE_OUTER_BOUND('',#3645,.T.);
#2436=FACE_OUTER_BOUND('',#3646,.T.);
#2437=FACE_OUTER_BOUND('',#3647,.T.);
#2438=FACE_OUTER_BOUND('',#3648,.T.);
#2439=FACE_OUTER_BOUND('',#3649,.T.);
#2440=FACE_OUTER_BOUND('',#3650,.T.);
#2441=FACE_OUTER_BOUND('',#3651,.T.);
#2442=FACE_OUTER_BOUND('',#3652,.T.);
#2443=FACE_OUTER_BOUND('',#3653,.T.);
#2444=FACE_OUTER_BOUND('',#3654,.T.);
#2445=FACE_OUTER_BOUND('',#3655,.T.);
#2446=FACE_OUTER_BOUND('',#3656,.T.);
#2447=FACE_OUTER_BOUND('',#3657,.T.);
#2448=FACE_OUTER_BOUND('',#3658,.T.);
#2449=FACE_OUTER_BOUND('',#3659,.T.);
#2450=FACE_OUTER_BOUND('',#3660,.T.);
#2451=FACE_OUTER_BOUND('',#3661,.T.);
#2452=FACE_OUTER_BOUND('',#3662,.T.);
#2453=FACE_OUTER_BOUND('',#3663,.T.);
#2454=FACE_OUTER_BOUND('',#3664,.T.);
#2455=FACE_OUTER_BOUND('',#3665,.T.);
#2456=FACE_OUTER_BOUND('',#3666,.T.);
#2457=FACE_OUTER_BOUND('',#3667,.T.);
#2458=FACE_OUTER_BOUND('',#3668,.T.);
#2459=FACE_OUTER_BOUND('',#3669,.T.);
#2460=FACE_OUTER_BOUND('',#3670,.T.);
#2461=FACE_OUTER_BOUND('',#3671,.T.);
#2462=FACE_OUTER_BOUND('',#3672,.T.);
#2463=FACE_OUTER_BOUND('',#3673,.T.);
#2464=FACE_OUTER_BOUND('',#3674,.T.);
#2465=FACE_OUTER_BOUND('',#3675,.T.);
#2466=FACE_OUTER_BOUND('',#3676,.T.);
#2467=FACE_OUTER_BOUND('',#3677,.T.);
#2468=FACE_OUTER_BOUND('',#3678,.T.);
#2469=FACE_OUTER_BOUND('',#3679,.T.);
#2470=FACE_OUTER_BOUND('',#3680,.T.);
#2471=FACE_OUTER_BOUND('',#3681,.T.);
#2472=FACE_OUTER_BOUND('',#3682,.T.);
#2473=FACE_OUTER_BOUND('',#3683,.T.);
#2474=FACE_OUTER_BOUND('',#3684,.T.);
#2475=FACE_OUTER_BOUND('',#3685,.T.);
#2476=FACE_OUTER_BOUND('',#3686,.T.);
#2477=FACE_OUTER_BOUND('',#3687,.T.);
#2478=FACE_OUTER_BOUND('',#3688,.T.);
#2479=FACE_OUTER_BOUND('',#3689,.T.);
#2480=FACE_OUTER_BOUND('',#3690,.T.);
#2481=FACE_OUTER_BOUND('',#3691,.T.);
#2482=FACE_OUTER_BOUND('',#3692,.T.);
#2483=FACE_OUTER_BOUND('',#3693,.T.);
#2484=FACE_OUTER_BOUND('',#3694,.T.);
#2485=FACE_OUTER_BOUND('',#3695,.T.);
#2486=FACE_OUTER_BOUND('',#3696,.T.);
#2487=FACE_OUTER_BOUND('',#3697,.T.);
#2488=FACE_OUTER_BOUND('',#3698,.T.);
#2489=FACE_OUTER_BOUND('',#3699,.T.);
#2490=FACE_OUTER_BOUND('',#3700,.T.);
#2491=FACE_OUTER_BOUND('',#3701,.T.);
#2492=FACE_OUTER_BOUND('',#3702,.T.);
#2493=FACE_OUTER_BOUND('',#3703,.T.);
#2494=FACE_OUTER_BOUND('',#3704,.T.);
#2495=FACE_OUTER_BOUND('',#3705,.T.);
#2496=FACE_OUTER_BOUND('',#3706,.T.);
#2497=FACE_OUTER_BOUND('',#3707,.T.);
#2498=FACE_OUTER_BOUND('',#3708,.T.);
#2499=FACE_OUTER_BOUND('',#3709,.T.);
#2500=FACE_OUTER_BOUND('',#3710,.T.);
#2501=FACE_OUTER_BOUND('',#3711,.T.);
#2502=FACE_OUTER_BOUND('',#3712,.T.);
#2503=FACE_OUTER_BOUND('',#3713,.T.);
#2504=FACE_OUTER_BOUND('',#3714,.T.);
#2505=FACE_OUTER_BOUND('',#3715,.T.);
#2506=FACE_OUTER_BOUND('',#3716,.T.);
#2507=FACE_OUTER_BOUND('',#3717,.T.);
#2508=FACE_OUTER_BOUND('',#3718,.T.);
#2509=FACE_OUTER_BOUND('',#3719,.T.);
#2510=FACE_OUTER_BOUND('',#3720,.T.);
#2511=FACE_OUTER_BOUND('',#3721,.T.);
#2512=FACE_OUTER_BOUND('',#3722,.T.);
#2513=FACE_OUTER_BOUND('',#3723,.T.);
#2514=FACE_OUTER_BOUND('',#3724,.T.);
#2515=FACE_OUTER_BOUND('',#3725,.T.);
#2516=FACE_OUTER_BOUND('',#3726,.T.);
#2517=FACE_OUTER_BOUND('',#3727,.T.);
#2518=FACE_OUTER_BOUND('',#3728,.T.);
#2519=FACE_OUTER_BOUND('',#3729,.T.);
#2520=FACE_OUTER_BOUND('',#3730,.T.);
#2521=FACE_OUTER_BOUND('',#3731,.T.);
#2522=FACE_OUTER_BOUND('',#3732,.T.);
#2523=FACE_OUTER_BOUND('',#3733,.T.);
#2524=FACE_OUTER_BOUND('',#3734,.T.);
#2525=FACE_OUTER_BOUND('',#3735,.T.);
#2526=FACE_OUTER_BOUND('',#3736,.T.);
#2527=FACE_OUTER_BOUND('',#3737,.T.);
#2528=FACE_OUTER_BOUND('',#3738,.T.);
#2529=FACE_OUTER_BOUND('',#3739,.T.);
#2530=FACE_OUTER_BOUND('',#3740,.T.);
#2531=FACE_OUTER_BOUND('',#3741,.T.);
#2532=FACE_OUTER_BOUND('',#3742,.T.);
#2533=FACE_OUTER_BOUND('',#3743,.T.);
#2534=FACE_OUTER_BOUND('',#3744,.T.);
#2535=FACE_OUTER_BOUND('',#3745,.T.);
#2536=FACE_OUTER_BOUND('',#3746,.T.);
#2537=FACE_OUTER_BOUND('',#3747,.T.);
#2538=FACE_OUTER_BOUND('',#3748,.T.);
#2539=FACE_OUTER_BOUND('',#3749,.T.);
#2540=FACE_OUTER_BOUND('',#3750,.T.);
#2541=FACE_OUTER_BOUND('',#3751,.T.);
#2542=FACE_OUTER_BOUND('',#3752,.T.);
#2543=FACE_OUTER_BOUND('',#3753,.T.);
#2544=FACE_OUTER_BOUND('',#3754,.T.);
#2545=FACE_OUTER_BOUND('',#3755,.T.);
#2546=FACE_OUTER_BOUND('',#3756,.T.);
#2547=FACE_OUTER_BOUND('',#3757,.T.);
#2548=FACE_OUTER_BOUND('',#3760,.T.);
#2549=FACE_OUTER_BOUND('',#3761,.T.);
#2550=FACE_OUTER_BOUND('',#3789,.T.);
#2551=FACE_OUTER_BOUND('',#3790,.T.);
#2552=FACE_OUTER_BOUND('',#3791,.T.);
#2553=FACE_OUTER_BOUND('',#3792,.T.);
#2554=FACE_OUTER_BOUND('',#3793,.T.);
#2555=FACE_OUTER_BOUND('',#3794,.T.);
#2556=FACE_OUTER_BOUND('',#3795,.T.);
#2557=FACE_OUTER_BOUND('',#3796,.T.);
#2558=FACE_OUTER_BOUND('',#3797,.T.);
#2559=FACE_OUTER_BOUND('',#3798,.T.);
#2560=FACE_OUTER_BOUND('',#3799,.T.);
#2561=FACE_OUTER_BOUND('',#3800,.T.);
#2562=FACE_OUTER_BOUND('',#3802,.T.);
#2563=FACE_OUTER_BOUND('',#3804,.T.);
#2564=FACE_OUTER_BOUND('',#3806,.T.);
#2565=FACE_OUTER_BOUND('',#3807,.T.);
#2566=FACE_OUTER_BOUND('',#3808,.T.);
#2567=FACE_OUTER_BOUND('',#3809,.T.);
#2568=FACE_OUTER_BOUND('',#3810,.T.);
#2569=FACE_OUTER_BOUND('',#3811,.T.);
#2570=FACE_OUTER_BOUND('',#3813,.T.);
#2571=FACE_OUTER_BOUND('',#3814,.T.);
#2572=FACE_OUTER_BOUND('',#3817,.T.);
#2573=FACE_OUTER_BOUND('',#3818,.T.);
#2574=FACE_OUTER_BOUND('',#3820,.T.);
#2575=FACE_OUTER_BOUND('',#3821,.T.);
#2576=FACE_OUTER_BOUND('',#3823,.T.);
#2577=FACE_OUTER_BOUND('',#3824,.T.);
#2578=FACE_OUTER_BOUND('',#3826,.T.);
#2579=FACE_OUTER_BOUND('',#3827,.T.);
#2580=FACE_OUTER_BOUND('',#3829,.T.);
#2581=FACE_OUTER_BOUND('',#3830,.T.);
#2582=FACE_OUTER_BOUND('',#3831,.T.);
#2583=FACE_OUTER_BOUND('',#3832,.T.);
#2584=FACE_OUTER_BOUND('',#3833,.T.);
#2585=FACE_OUTER_BOUND('',#3834,.T.);
#2586=FACE_OUTER_BOUND('',#3835,.T.);
#2587=FACE_OUTER_BOUND('',#3836,.T.);
#2588=FACE_OUTER_BOUND('',#3837,.T.);
#2589=FACE_OUTER_BOUND('',#3838,.T.);
#2590=FACE_OUTER_BOUND('',#3839,.T.);
#2591=FACE_OUTER_BOUND('',#3840,.T.);
#2592=FACE_OUTER_BOUND('',#3841,.T.);
#2593=FACE_OUTER_BOUND('',#3842,.T.);
#2594=FACE_OUTER_BOUND('',#3844,.T.);
#2595=FACE_OUTER_BOUND('',#3845,.T.);
#2596=FACE_OUTER_BOUND('',#3846,.T.);
#2597=FACE_OUTER_BOUND('',#3847,.T.);
#2598=FACE_OUTER_BOUND('',#3848,.T.);
#2599=FACE_OUTER_BOUND('',#3849,.T.);
#2600=FACE_OUTER_BOUND('',#3850,.T.);
#2601=FACE_OUTER_BOUND('',#3852,.T.);
#2602=FACE_OUTER_BOUND('',#3853,.T.);
#2603=FACE_OUTER_BOUND('',#3855,.T.);
#2604=FACE_OUTER_BOUND('',#3856,.T.);
#2605=FACE_OUTER_BOUND('',#3857,.T.);
#2606=FACE_OUTER_BOUND('',#3858,.T.);
#2607=FACE_OUTER_BOUND('',#3860,.T.);
#2608=FACE_OUTER_BOUND('',#3861,.T.);
#2609=FACE_OUTER_BOUND('',#3862,.T.);
#2610=FACE_OUTER_BOUND('',#3863,.T.);
#2611=FACE_OUTER_BOUND('',#3865,.T.);
#2612=FACE_OUTER_BOUND('',#3866,.T.);
#2613=FACE_OUTER_BOUND('',#3867,.T.);
#2614=FACE_OUTER_BOUND('',#3868,.T.);
#2615=FACE_OUTER_BOUND('',#3869,.T.);
#2616=FACE_OUTER_BOUND('',#3870,.T.);
#2617=FACE_OUTER_BOUND('',#3871,.T.);
#2618=FACE_OUTER_BOUND('',#3872,.T.);
#2619=FACE_OUTER_BOUND('',#3873,.T.);
#2620=FACE_OUTER_BOUND('',#3874,.T.);
#2621=FACE_OUTER_BOUND('',#3875,.T.);
#2622=FACE_OUTER_BOUND('',#3876,.T.);
#2623=FACE_OUTER_BOUND('',#3877,.T.);
#2624=FACE_OUTER_BOUND('',#3878,.T.);
#2625=FACE_OUTER_BOUND('',#3879,.T.);
#2626=FACE_OUTER_BOUND('',#3880,.T.);
#2627=FACE_OUTER_BOUND('',#3881,.T.);
#2628=FACE_OUTER_BOUND('',#3882,.T.);
#2629=FACE_OUTER_BOUND('',#3883,.T.);
#2630=FACE_OUTER_BOUND('',#3884,.T.);
#2631=FACE_OUTER_BOUND('',#3885,.T.);
#2632=FACE_OUTER_BOUND('',#3886,.T.);
#2633=FACE_OUTER_BOUND('',#3887,.T.);
#2634=FACE_OUTER_BOUND('',#3888,.T.);
#2635=FACE_OUTER_BOUND('',#3890,.T.);
#2636=FACE_OUTER_BOUND('',#3891,.T.);
#2637=FACE_OUTER_BOUND('',#3893,.T.);
#2638=FACE_OUTER_BOUND('',#3894,.T.);
#2639=FACE_OUTER_BOUND('',#3896,.T.);
#2640=FACE_OUTER_BOUND('',#3897,.T.);
#2641=FACE_OUTER_BOUND('',#3899,.T.);
#2642=FACE_OUTER_BOUND('',#3900,.T.);
#2643=FACE_OUTER_BOUND('',#3902,.T.);
#2644=FACE_OUTER_BOUND('',#3903,.T.);
#2645=FACE_OUTER_BOUND('',#3904,.T.);
#2646=FACE_OUTER_BOUND('',#3905,.T.);
#2647=FACE_OUTER_BOUND('',#3906,.T.);
#2648=FACE_OUTER_BOUND('',#3907,.T.);
#2649=FACE_OUTER_BOUND('',#3909,.T.);
#2650=FACE_OUTER_BOUND('',#3910,.T.);
#2651=FACE_OUTER_BOUND('',#3912,.T.);
#2652=FACE_OUTER_BOUND('',#3913,.T.);
#2653=FACE_OUTER_BOUND('',#3914,.T.);
#2654=FACE_OUTER_BOUND('',#3915,.T.);
#2655=FACE_OUTER_BOUND('',#3917,.T.);
#2656=FACE_OUTER_BOUND('',#3918,.T.);
#2657=FACE_OUTER_BOUND('',#3919,.T.);
#2658=FACE_OUTER_BOUND('',#3920,.T.);
#2659=FACE_OUTER_BOUND('',#3922,.T.);
#2660=FACE_OUTER_BOUND('',#3923,.T.);
#2661=FACE_OUTER_BOUND('',#3924,.T.);
#2662=FACE_OUTER_BOUND('',#3925,.T.);
#2663=FACE_OUTER_BOUND('',#3926,.T.);
#2664=FACE_OUTER_BOUND('',#3927,.T.);
#2665=FACE_OUTER_BOUND('',#3928,.T.);
#2666=FACE_OUTER_BOUND('',#3929,.T.);
#2667=FACE_OUTER_BOUND('',#3930,.T.);
#2668=FACE_OUTER_BOUND('',#3931,.T.);
#2669=FACE_OUTER_BOUND('',#3932,.T.);
#2670=FACE_OUTER_BOUND('',#3933,.T.);
#2671=FACE_OUTER_BOUND('',#3934,.T.);
#2672=FACE_OUTER_BOUND('',#3935,.T.);
#2673=FACE_OUTER_BOUND('',#3936,.T.);
#2674=FACE_OUTER_BOUND('',#3937,.T.);
#2675=FACE_OUTER_BOUND('',#3938,.T.);
#2676=FACE_OUTER_BOUND('',#3939,.T.);
#2677=FACE_OUTER_BOUND('',#3940,.T.);
#2678=FACE_OUTER_BOUND('',#3941,.T.);
#2679=FACE_OUTER_BOUND('',#3942,.T.);
#2680=FACE_OUTER_BOUND('',#3943,.T.);
#2681=FACE_OUTER_BOUND('',#3944,.T.);
#2682=FACE_OUTER_BOUND('',#3945,.T.);
#2683=FACE_OUTER_BOUND('',#3946,.T.);
#2684=FACE_OUTER_BOUND('',#3947,.T.);
#2685=FACE_OUTER_BOUND('',#3948,.T.);
#2686=FACE_OUTER_BOUND('',#3950,.T.);
#2687=FACE_OUTER_BOUND('',#3951,.T.);
#2688=FACE_OUTER_BOUND('',#3953,.T.);
#2689=FACE_OUTER_BOUND('',#3954,.T.);
#2690=FACE_OUTER_BOUND('',#3956,.T.);
#2691=FACE_OUTER_BOUND('',#3957,.T.);
#2692=FACE_OUTER_BOUND('',#3959,.T.);
#2693=FACE_OUTER_BOUND('',#3960,.T.);
#2694=FACE_OUTER_BOUND('',#3962,.T.);
#2695=FACE_OUTER_BOUND('',#3963,.T.);
#2696=FACE_OUTER_BOUND('',#3964,.T.);
#2697=FACE_OUTER_BOUND('',#3966,.T.);
#2698=FACE_OUTER_BOUND('',#3967,.T.);
#2699=FACE_OUTER_BOUND('',#3968,.T.);
#2700=FACE_OUTER_BOUND('',#3969,.T.);
#2701=FACE_OUTER_BOUND('',#3970,.T.);
#2702=FACE_OUTER_BOUND('',#3971,.T.);
#2703=FACE_OUTER_BOUND('',#3973,.T.);
#2704=FACE_OUTER_BOUND('',#3974,.T.);
#2705=FACE_OUTER_BOUND('',#3975,.T.);
#2706=FACE_OUTER_BOUND('',#3976,.T.);
#2707=FACE_OUTER_BOUND('',#3977,.T.);
#2708=FACE_OUTER_BOUND('',#3978,.T.);
#2709=FACE_OUTER_BOUND('',#3979,.T.);
#2710=FACE_OUTER_BOUND('',#3980,.T.);
#2711=FACE_OUTER_BOUND('',#3981,.T.);
#2712=FACE_OUTER_BOUND('',#3982,.T.);
#2713=FACE_OUTER_BOUND('',#3983,.T.);
#2714=FACE_OUTER_BOUND('',#3984,.T.);
#2715=FACE_OUTER_BOUND('',#3985,.T.);
#2716=FACE_OUTER_BOUND('',#3986,.T.);
#2717=FACE_OUTER_BOUND('',#3987,.T.);
#2718=FACE_OUTER_BOUND('',#3988,.T.);
#2719=FACE_OUTER_BOUND('',#3989,.T.);
#2720=FACE_OUTER_BOUND('',#3990,.T.);
#2721=FACE_OUTER_BOUND('',#3991,.T.);
#2722=FACE_OUTER_BOUND('',#3992,.T.);
#2723=FACE_OUTER_BOUND('',#3993,.T.);
#2724=FACE_OUTER_BOUND('',#3994,.T.);
#2725=FACE_OUTER_BOUND('',#3995,.T.);
#2726=FACE_OUTER_BOUND('',#3996,.T.);
#2727=FACE_OUTER_BOUND('',#3998,.T.);
#2728=FACE_OUTER_BOUND('',#3999,.T.);
#2729=FACE_OUTER_BOUND('',#4000,.T.);
#2730=FACE_OUTER_BOUND('',#4001,.T.);
#2731=FACE_OUTER_BOUND('',#4002,.T.);
#2732=FACE_OUTER_BOUND('',#4003,.T.);
#2733=FACE_OUTER_BOUND('',#4004,.T.);
#2734=FACE_OUTER_BOUND('',#4005,.T.);
#2735=FACE_OUTER_BOUND('',#4006,.T.);
#2736=FACE_OUTER_BOUND('',#4007,.T.);
#2737=FACE_OUTER_BOUND('',#4008,.T.);
#2738=FACE_OUTER_BOUND('',#4009,.T.);
#2739=FACE_OUTER_BOUND('',#4010,.T.);
#2740=FACE_OUTER_BOUND('',#4011,.T.);
#2741=FACE_OUTER_BOUND('',#4012,.T.);
#2742=FACE_OUTER_BOUND('',#4013,.T.);
#2743=FACE_OUTER_BOUND('',#4014,.T.);
#2744=FACE_OUTER_BOUND('',#4015,.T.);
#2745=FACE_OUTER_BOUND('',#4016,.T.);
#2746=FACE_OUTER_BOUND('',#4017,.T.);
#2747=FACE_OUTER_BOUND('',#4018,.T.);
#2748=FACE_OUTER_BOUND('',#4019,.T.);
#2749=FACE_OUTER_BOUND('',#4020,.T.);
#2750=FACE_OUTER_BOUND('',#4021,.T.);
#2751=FACE_OUTER_BOUND('',#4022,.T.);
#2752=FACE_OUTER_BOUND('',#4023,.T.);
#2753=FACE_OUTER_BOUND('',#4024,.T.);
#2754=FACE_OUTER_BOUND('',#4025,.T.);
#2755=FACE_OUTER_BOUND('',#4026,.T.);
#2756=FACE_OUTER_BOUND('',#4027,.T.);
#2757=FACE_OUTER_BOUND('',#4028,.T.);
#2758=FACE_OUTER_BOUND('',#4029,.T.);
#2759=FACE_OUTER_BOUND('',#4030,.T.);
#2760=FACE_OUTER_BOUND('',#4031,.T.);
#2761=FACE_OUTER_BOUND('',#4032,.T.);
#2762=FACE_OUTER_BOUND('',#4033,.T.);
#2763=FACE_OUTER_BOUND('',#4034,.T.);
#2764=FACE_OUTER_BOUND('',#4035,.T.);
#2765=FACE_OUTER_BOUND('',#4036,.T.);
#2766=FACE_OUTER_BOUND('',#4037,.T.);
#2767=FACE_OUTER_BOUND('',#4038,.T.);
#2768=FACE_OUTER_BOUND('',#4039,.T.);
#2769=FACE_OUTER_BOUND('',#4040,.T.);
#2770=FACE_OUTER_BOUND('',#4041,.T.);
#2771=FACE_OUTER_BOUND('',#4042,.T.);
#2772=FACE_OUTER_BOUND('',#4043,.T.);
#2773=FACE_OUTER_BOUND('',#4044,.T.);
#2774=FACE_OUTER_BOUND('',#4045,.T.);
#2775=FACE_OUTER_BOUND('',#4047,.T.);
#2776=FACE_OUTER_BOUND('',#4049,.T.);
#2777=FACE_OUTER_BOUND('',#4050,.T.);
#2778=FACE_OUTER_BOUND('',#4051,.T.);
#2779=FACE_OUTER_BOUND('',#4052,.T.);
#2780=FACE_OUTER_BOUND('',#4053,.T.);
#2781=FACE_OUTER_BOUND('',#4055,.T.);
#2782=FACE_OUTER_BOUND('',#4056,.T.);
#2783=FACE_OUTER_BOUND('',#4057,.T.);
#2784=FACE_OUTER_BOUND('',#4058,.T.);
#2785=FACE_OUTER_BOUND('',#4059,.T.);
#2786=FACE_OUTER_BOUND('',#4060,.T.);
#2787=FACE_OUTER_BOUND('',#4061,.T.);
#2788=FACE_OUTER_BOUND('',#4062,.T.);
#2789=FACE_OUTER_BOUND('',#4063,.T.);
#2790=FACE_OUTER_BOUND('',#4064,.T.);
#2791=FACE_OUTER_BOUND('',#4065,.T.);
#2792=FACE_OUTER_BOUND('',#4066,.T.);
#2793=FACE_OUTER_BOUND('',#4067,.T.);
#2794=FACE_OUTER_BOUND('',#4068,.T.);
#2795=FACE_OUTER_BOUND('',#4069,.T.);
#2796=FACE_OUTER_BOUND('',#4071,.T.);
#2797=FACE_OUTER_BOUND('',#4072,.T.);
#2798=FACE_OUTER_BOUND('',#4073,.T.);
#2799=FACE_OUTER_BOUND('',#4074,.T.);
#2800=FACE_OUTER_BOUND('',#4075,.T.);
#2801=FACE_OUTER_BOUND('',#4076,.T.);
#2802=FACE_OUTER_BOUND('',#4077,.T.);
#2803=FACE_OUTER_BOUND('',#4078,.T.);
#2804=FACE_OUTER_BOUND('',#4079,.T.);
#2805=FACE_OUTER_BOUND('',#4080,.T.);
#2806=FACE_OUTER_BOUND('',#4081,.T.);
#2807=FACE_OUTER_BOUND('',#4082,.T.);
#2808=FACE_OUTER_BOUND('',#4084,.T.);
#2809=FACE_OUTER_BOUND('',#4085,.T.);
#2810=FACE_OUTER_BOUND('',#4086,.T.);
#2811=FACE_OUTER_BOUND('',#4087,.T.);
#2812=FACE_OUTER_BOUND('',#4088,.T.);
#2813=FACE_OUTER_BOUND('',#4090,.T.);
#2814=FACE_OUTER_BOUND('',#4091,.T.);
#2815=FACE_OUTER_BOUND('',#4092,.T.);
#2816=FACE_OUTER_BOUND('',#4093,.T.);
#2817=FACE_OUTER_BOUND('',#4094,.T.);
#2818=FACE_OUTER_BOUND('',#4095,.T.);
#2819=FACE_OUTER_BOUND('',#4096,.T.);
#2820=FACE_OUTER_BOUND('',#4097,.T.);
#2821=FACE_OUTER_BOUND('',#4098,.T.);
#2822=FACE_OUTER_BOUND('',#4099,.T.);
#2823=FACE_OUTER_BOUND('',#4100,.T.);
#2824=FACE_OUTER_BOUND('',#4101,.T.);
#2825=FACE_OUTER_BOUND('',#4102,.T.);
#2826=FACE_OUTER_BOUND('',#4103,.T.);
#2827=FACE_OUTER_BOUND('',#4104,.T.);
#2828=FACE_OUTER_BOUND('',#4105,.T.);
#2829=FACE_OUTER_BOUND('',#4106,.T.);
#2830=FACE_OUTER_BOUND('',#4107,.T.);
#2831=FACE_OUTER_BOUND('',#4108,.T.);
#2832=FACE_OUTER_BOUND('',#4109,.T.);
#2833=FACE_OUTER_BOUND('',#4110,.T.);
#2834=FACE_OUTER_BOUND('',#4111,.T.);
#2835=FACE_OUTER_BOUND('',#4112,.T.);
#2836=FACE_OUTER_BOUND('',#4113,.T.);
#2837=FACE_OUTER_BOUND('',#4114,.T.);
#2838=FACE_OUTER_BOUND('',#4115,.T.);
#2839=FACE_OUTER_BOUND('',#4116,.T.);
#2840=FACE_OUTER_BOUND('',#4117,.T.);
#2841=FACE_OUTER_BOUND('',#4118,.T.);
#2842=FACE_OUTER_BOUND('',#4119,.T.);
#2843=FACE_OUTER_BOUND('',#4120,.T.);
#2844=FACE_OUTER_BOUND('',#4121,.T.);
#2845=FACE_OUTER_BOUND('',#4140,.T.);
#2846=FACE_OUTER_BOUND('',#4159,.T.);
#2847=FACE_OUTER_BOUND('',#4160,.T.);
#2848=FACE_OUTER_BOUND('',#4161,.T.);
#2849=FACE_OUTER_BOUND('',#4162,.T.);
#2850=FACE_OUTER_BOUND('',#4163,.T.);
#2851=FACE_OUTER_BOUND('',#4164,.T.);
#2852=FACE_OUTER_BOUND('',#4165,.T.);
#2853=FACE_OUTER_BOUND('',#4166,.T.);
#2854=FACE_OUTER_BOUND('',#4167,.T.);
#2855=FACE_OUTER_BOUND('',#4168,.T.);
#2856=FACE_OUTER_BOUND('',#4169,.T.);
#2857=FACE_OUTER_BOUND('',#4171,.T.);
#2858=FACE_OUTER_BOUND('',#4173,.T.);
#2859=FACE_OUTER_BOUND('',#4174,.T.);
#2860=FACE_OUTER_BOUND('',#4175,.T.);
#2861=FACE_OUTER_BOUND('',#4181,.T.);
#2862=FACE_OUTER_BOUND('',#4183,.T.);
#2863=FACE_OUTER_BOUND('',#4184,.T.);
#2864=FACE_OUTER_BOUND('',#4185,.T.);
#2865=FACE_OUTER_BOUND('',#4186,.T.);
#2866=FACE_OUTER_BOUND('',#4187,.T.);
#2867=FACE_OUTER_BOUND('',#4188,.T.);
#2868=FACE_OUTER_BOUND('',#4189,.T.);
#2869=FACE_OUTER_BOUND('',#4190,.T.);
#2870=FACE_OUTER_BOUND('',#4191,.T.);
#2871=FACE_OUTER_BOUND('',#4192,.T.);
#2872=FACE_OUTER_BOUND('',#4193,.T.);
#2873=FACE_OUTER_BOUND('',#4195,.T.);
#2874=FACE_OUTER_BOUND('',#4197,.T.);
#2875=FACE_OUTER_BOUND('',#4198,.T.);
#2876=FACE_OUTER_BOUND('',#4199,.T.);
#2877=FACE_OUTER_BOUND('',#4205,.T.);
#2878=FACE_OUTER_BOUND('',#4207,.T.);
#2879=FACE_OUTER_BOUND('',#4208,.T.);
#2880=FACE_OUTER_BOUND('',#4209,.T.);
#2881=FACE_OUTER_BOUND('',#4210,.T.);
#2882=FACE_OUTER_BOUND('',#4211,.T.);
#2883=FACE_OUTER_BOUND('',#4212,.T.);
#2884=FACE_OUTER_BOUND('',#4213,.T.);
#2885=FACE_OUTER_BOUND('',#4214,.T.);
#2886=FACE_OUTER_BOUND('',#4215,.T.);
#2887=FACE_OUTER_BOUND('',#4220,.T.);
#2888=FACE_OUTER_BOUND('',#4222,.T.);
#2889=FACE_OUTER_BOUND('',#4223,.T.);
#2890=FACE_OUTER_BOUND('',#4224,.T.);
#2891=FACE_OUTER_BOUND('',#4225,.T.);
#2892=FACE_OUTER_BOUND('',#4228,.T.);
#2893=FACE_OUTER_BOUND('',#4231,.T.);
#2894=FACE_OUTER_BOUND('',#4232,.T.);
#2895=FACE_OUTER_BOUND('',#4233,.T.);
#2896=FACE_OUTER_BOUND('',#4234,.T.);
#2897=FACE_OUTER_BOUND('',#4235,.T.);
#2898=FACE_OUTER_BOUND('',#4236,.T.);
#2899=FACE_OUTER_BOUND('',#4237,.T.);
#2900=FACE_OUTER_BOUND('',#4240,.T.);
#2901=FACE_OUTER_BOUND('',#4241,.T.);
#2902=FACE_OUTER_BOUND('',#4242,.T.);
#2903=FACE_OUTER_BOUND('',#4243,.T.);
#2904=FACE_OUTER_BOUND('',#4244,.T.);
#2905=FACE_OUTER_BOUND('',#4245,.T.);
#2906=FACE_OUTER_BOUND('',#4246,.T.);
#2907=FACE_OUTER_BOUND('',#4249,.T.);
#2908=FACE_OUTER_BOUND('',#4250,.T.);
#2909=FACE_OUTER_BOUND('',#4251,.T.);
#2910=FACE_OUTER_BOUND('',#4252,.T.);
#2911=FACE_OUTER_BOUND('',#4253,.T.);
#2912=FACE_OUTER_BOUND('',#4254,.T.);
#2913=FACE_OUTER_BOUND('',#4255,.T.);
#2914=FACE_OUTER_BOUND('',#4257,.T.);
#2915=FACE_OUTER_BOUND('',#4258,.T.);
#2916=FACE_OUTER_BOUND('',#4260,.T.);
#2917=FACE_OUTER_BOUND('',#4261,.T.);
#2918=FACE_OUTER_BOUND('',#4263,.T.);
#2919=FACE_OUTER_BOUND('',#4264,.T.);
#2920=FACE_OUTER_BOUND('',#4266,.T.);
#2921=FACE_OUTER_BOUND('',#4267,.T.);
#2922=FACE_OUTER_BOUND('',#4269,.T.);
#2923=FACE_OUTER_BOUND('',#4270,.T.);
#2924=FACE_OUTER_BOUND('',#4272,.T.);
#2925=FACE_OUTER_BOUND('',#4274,.T.);
#2926=FACE_OUTER_BOUND('',#4275,.T.);
#2927=FACE_OUTER_BOUND('',#4276,.T.);
#2928=FACE_OUTER_BOUND('',#4277,.T.);
#2929=FACE_OUTER_BOUND('',#4278,.T.);
#2930=FACE_OUTER_BOUND('',#4280,.T.);
#2931=FACE_OUTER_BOUND('',#4282,.T.);
#2932=FACE_OUTER_BOUND('',#4284,.T.);
#2933=FACE_OUTER_BOUND('',#4286,.T.);
#2934=FACE_OUTER_BOUND('',#4287,.T.);
#2935=FACE_OUTER_BOUND('',#4288,.T.);
#2936=FACE_OUTER_BOUND('',#4289,.T.);
#2937=FACE_OUTER_BOUND('',#4290,.T.);
#2938=FACE_OUTER_BOUND('',#4291,.T.);
#2939=FACE_OUTER_BOUND('',#4292,.T.);
#2940=FACE_OUTER_BOUND('',#4293,.T.);
#2941=FACE_OUTER_BOUND('',#4294,.T.);
#2942=FACE_OUTER_BOUND('',#4295,.T.);
#2943=FACE_OUTER_BOUND('',#4296,.T.);
#2944=FACE_OUTER_BOUND('',#4297,.T.);
#2945=FACE_OUTER_BOUND('',#4298,.T.);
#2946=FACE_OUTER_BOUND('',#4299,.T.);
#2947=FACE_OUTER_BOUND('',#4300,.T.);
#2948=FACE_OUTER_BOUND('',#4301,.T.);
#2949=FACE_OUTER_BOUND('',#4302,.T.);
#2950=FACE_OUTER_BOUND('',#4303,.T.);
#2951=FACE_OUTER_BOUND('',#4304,.T.);
#2952=FACE_OUTER_BOUND('',#4305,.T.);
#2953=FACE_OUTER_BOUND('',#4306,.T.);
#2954=FACE_OUTER_BOUND('',#4307,.T.);
#2955=FACE_OUTER_BOUND('',#4312,.T.);
#2956=FACE_OUTER_BOUND('',#4313,.T.);
#2957=FACE_OUTER_BOUND('',#4314,.T.);
#2958=FACE_OUTER_BOUND('',#4315,.T.);
#2959=FACE_OUTER_BOUND('',#4316,.T.);
#2960=FACE_OUTER_BOUND('',#4321,.T.);
#2961=FACE_OUTER_BOUND('',#4322,.T.);
#2962=FACE_OUTER_BOUND('',#4323,.T.);
#2963=FACE_OUTER_BOUND('',#4324,.T.);
#2964=FACE_OUTER_BOUND('',#4326,.T.);
#2965=FACE_OUTER_BOUND('',#4327,.T.);
#2966=FACE_OUTER_BOUND('',#4328,.T.);
#2967=FACE_OUTER_BOUND('',#4329,.T.);
#2968=FACE_OUTER_BOUND('',#4330,.T.);
#2969=FACE_OUTER_BOUND('',#4331,.T.);
#2970=FACE_OUTER_BOUND('',#4332,.T.);
#2971=FACE_OUTER_BOUND('',#4333,.T.);
#2972=FACE_OUTER_BOUND('',#4334,.T.);
#2973=FACE_OUTER_BOUND('',#4336,.T.);
#2974=FACE_OUTER_BOUND('',#4337,.T.);
#2975=FACE_OUTER_BOUND('',#4338,.T.);
#2976=FACE_OUTER_BOUND('',#4339,.T.);
#2977=FACE_OUTER_BOUND('',#4340,.T.);
#2978=FACE_OUTER_BOUND('',#4341,.T.);
#2979=FACE_OUTER_BOUND('',#4342,.T.);
#2980=FACE_OUTER_BOUND('',#4344,.T.);
#2981=FACE_OUTER_BOUND('',#4345,.T.);
#2982=FACE_OUTER_BOUND('',#4346,.T.);
#2983=FACE_OUTER_BOUND('',#4347,.T.);
#2984=FACE_OUTER_BOUND('',#4348,.T.);
#2985=FACE_OUTER_BOUND('',#4349,.T.);
#2986=FACE_OUTER_BOUND('',#4350,.T.);
#2987=FACE_OUTER_BOUND('',#4352,.T.);
#2988=FACE_OUTER_BOUND('',#4353,.T.);
#2989=FACE_OUTER_BOUND('',#4354,.T.);
#2990=FACE_OUTER_BOUND('',#4355,.T.);
#2991=FACE_OUTER_BOUND('',#4356,.T.);
#2992=FACE_OUTER_BOUND('',#4357,.T.);
#2993=FACE_OUTER_BOUND('',#4358,.T.);
#2994=FACE_OUTER_BOUND('',#4359,.T.);
#2995=FACE_OUTER_BOUND('',#4360,.T.);
#2996=FACE_OUTER_BOUND('',#4361,.T.);
#2997=FACE_OUTER_BOUND('',#4362,.T.);
#2998=FACE_OUTER_BOUND('',#4363,.T.);
#2999=FACE_OUTER_BOUND('',#4364,.T.);
#3000=FACE_OUTER_BOUND('',#4365,.T.);
#3001=FACE_OUTER_BOUND('',#4366,.T.);
#3002=FACE_OUTER_BOUND('',#4367,.T.);
#3003=FACE_OUTER_BOUND('',#4368,.T.);
#3004=FACE_OUTER_BOUND('',#4369,.T.);
#3005=FACE_OUTER_BOUND('',#4370,.T.);
#3006=FACE_OUTER_BOUND('',#4371,.T.);
#3007=FACE_OUTER_BOUND('',#4372,.T.);
#3008=FACE_OUTER_BOUND('',#4373,.T.);
#3009=FACE_OUTER_BOUND('',#4374,.T.);
#3010=FACE_OUTER_BOUND('',#4375,.T.);
#3011=FACE_OUTER_BOUND('',#4376,.T.);
#3012=FACE_OUTER_BOUND('',#4377,.T.);
#3013=FACE_OUTER_BOUND('',#4378,.T.);
#3014=FACE_OUTER_BOUND('',#4379,.T.);
#3015=FACE_OUTER_BOUND('',#4380,.T.);
#3016=FACE_OUTER_BOUND('',#4381,.T.);
#3017=FACE_OUTER_BOUND('',#4382,.T.);
#3018=FACE_OUTER_BOUND('',#4383,.T.);
#3019=FACE_OUTER_BOUND('',#4384,.T.);
#3020=FACE_OUTER_BOUND('',#4385,.T.);
#3021=FACE_OUTER_BOUND('',#4386,.T.);
#3022=FACE_OUTER_BOUND('',#4387,.T.);
#3023=FACE_OUTER_BOUND('',#4388,.T.);
#3024=FACE_OUTER_BOUND('',#4389,.T.);
#3025=FACE_OUTER_BOUND('',#4390,.T.);
#3026=FACE_OUTER_BOUND('',#4391,.T.);
#3027=FACE_OUTER_BOUND('',#4392,.T.);
#3028=FACE_OUTER_BOUND('',#4393,.T.);
#3029=FACE_OUTER_BOUND('',#4394,.T.);
#3030=FACE_OUTER_BOUND('',#4395,.T.);
#3031=FACE_OUTER_BOUND('',#4396,.T.);
#3032=FACE_OUTER_BOUND('',#4397,.T.);
#3033=FACE_OUTER_BOUND('',#4398,.T.);
#3034=FACE_OUTER_BOUND('',#4399,.T.);
#3035=FACE_OUTER_BOUND('',#4400,.T.);
#3036=FACE_OUTER_BOUND('',#4401,.T.);
#3037=FACE_OUTER_BOUND('',#4402,.T.);
#3038=FACE_OUTER_BOUND('',#4403,.T.);
#3039=FACE_OUTER_BOUND('',#4404,.T.);
#3040=FACE_OUTER_BOUND('',#4405,.T.);
#3041=FACE_OUTER_BOUND('',#4406,.T.);
#3042=FACE_OUTER_BOUND('',#4407,.T.);
#3043=FACE_OUTER_BOUND('',#4408,.T.);
#3044=FACE_OUTER_BOUND('',#4409,.T.);
#3045=FACE_OUTER_BOUND('',#4410,.T.);
#3046=FACE_OUTER_BOUND('',#4411,.T.);
#3047=FACE_OUTER_BOUND('',#4412,.T.);
#3048=FACE_OUTER_BOUND('',#4413,.T.);
#3049=FACE_OUTER_BOUND('',#4414,.T.);
#3050=FACE_OUTER_BOUND('',#4415,.T.);
#3051=FACE_OUTER_BOUND('',#4416,.T.);
#3052=FACE_OUTER_BOUND('',#4417,.T.);
#3053=FACE_OUTER_BOUND('',#4418,.T.);
#3054=FACE_OUTER_BOUND('',#4419,.T.);
#3055=FACE_OUTER_BOUND('',#4420,.T.);
#3056=FACE_OUTER_BOUND('',#4421,.T.);
#3057=FACE_OUTER_BOUND('',#4422,.T.);
#3058=FACE_OUTER_BOUND('',#4423,.T.);
#3059=FACE_OUTER_BOUND('',#4424,.T.);
#3060=FACE_OUTER_BOUND('',#4425,.T.);
#3061=FACE_OUTER_BOUND('',#4426,.T.);
#3062=FACE_OUTER_BOUND('',#4427,.T.);
#3063=FACE_OUTER_BOUND('',#4428,.T.);
#3064=FACE_OUTER_BOUND('',#4429,.T.);
#3065=FACE_OUTER_BOUND('',#4430,.T.);
#3066=FACE_OUTER_BOUND('',#4431,.T.);
#3067=FACE_OUTER_BOUND('',#4432,.T.);
#3068=FACE_OUTER_BOUND('',#4433,.T.);
#3069=FACE_OUTER_BOUND('',#4434,.T.);
#3070=FACE_OUTER_BOUND('',#4435,.T.);
#3071=FACE_OUTER_BOUND('',#4436,.T.);
#3072=FACE_OUTER_BOUND('',#4437,.T.);
#3073=FACE_OUTER_BOUND('',#4438,.T.);
#3074=FACE_OUTER_BOUND('',#4439,.T.);
#3075=FACE_OUTER_BOUND('',#4440,.T.);
#3076=FACE_OUTER_BOUND('',#4441,.T.);
#3077=FACE_OUTER_BOUND('',#4442,.T.);
#3078=FACE_OUTER_BOUND('',#4443,.T.);
#3079=FACE_OUTER_BOUND('',#4444,.T.);
#3080=FACE_OUTER_BOUND('',#4445,.T.);
#3081=FACE_OUTER_BOUND('',#4446,.T.);
#3082=FACE_OUTER_BOUND('',#4447,.T.);
#3083=FACE_OUTER_BOUND('',#4448,.T.);
#3084=FACE_OUTER_BOUND('',#4449,.T.);
#3085=FACE_OUTER_BOUND('',#4450,.T.);
#3086=FACE_OUTER_BOUND('',#4451,.T.);
#3087=FACE_OUTER_BOUND('',#4452,.T.);
#3088=FACE_OUTER_BOUND('',#4453,.T.);
#3089=FACE_OUTER_BOUND('',#4454,.T.);
#3090=FACE_OUTER_BOUND('',#4455,.T.);
#3091=FACE_OUTER_BOUND('',#4456,.T.);
#3092=FACE_OUTER_BOUND('',#4457,.T.);
#3093=FACE_OUTER_BOUND('',#4458,.T.);
#3094=FACE_OUTER_BOUND('',#4459,.T.);
#3095=FACE_OUTER_BOUND('',#4460,.T.);
#3096=FACE_OUTER_BOUND('',#4461,.T.);
#3097=FACE_OUTER_BOUND('',#4462,.T.);
#3098=FACE_OUTER_BOUND('',#4463,.T.);
#3099=FACE_OUTER_BOUND('',#4464,.T.);
#3100=FACE_OUTER_BOUND('',#4465,.T.);
#3101=FACE_OUTER_BOUND('',#4466,.T.);
#3102=FACE_OUTER_BOUND('',#4467,.T.);
#3103=FACE_OUTER_BOUND('',#4468,.T.);
#3104=FACE_OUTER_BOUND('',#4469,.T.);
#3105=FACE_OUTER_BOUND('',#4470,.T.);
#3106=FACE_OUTER_BOUND('',#4471,.T.);
#3107=FACE_OUTER_BOUND('',#4472,.T.);
#3108=FACE_OUTER_BOUND('',#4473,.T.);
#3109=FACE_OUTER_BOUND('',#4474,.T.);
#3110=FACE_OUTER_BOUND('',#4475,.T.);
#3111=FACE_OUTER_BOUND('',#4476,.T.);
#3112=FACE_OUTER_BOUND('',#4477,.T.);
#3113=FACE_OUTER_BOUND('',#4478,.T.);
#3114=FACE_OUTER_BOUND('',#4479,.T.);
#3115=FACE_OUTER_BOUND('',#4480,.T.);
#3116=FACE_OUTER_BOUND('',#4481,.T.);
#3117=FACE_OUTER_BOUND('',#4482,.T.);
#3118=FACE_OUTER_BOUND('',#4483,.T.);
#3119=FACE_OUTER_BOUND('',#4484,.T.);
#3120=FACE_OUTER_BOUND('',#4485,.T.);
#3121=FACE_OUTER_BOUND('',#4486,.T.);
#3122=FACE_OUTER_BOUND('',#4487,.T.);
#3123=FACE_OUTER_BOUND('',#4488,.T.);
#3124=FACE_OUTER_BOUND('',#4489,.T.);
#3125=FACE_OUTER_BOUND('',#4490,.T.);
#3126=FACE_OUTER_BOUND('',#4492,.T.);
#3127=FACE_OUTER_BOUND('',#4493,.T.);
#3128=FACE_OUTER_BOUND('',#4494,.T.);
#3129=FACE_OUTER_BOUND('',#4495,.T.);
#3130=FACE_OUTER_BOUND('',#4496,.T.);
#3131=FACE_OUTER_BOUND('',#4497,.T.);
#3132=FACE_OUTER_BOUND('',#4498,.T.);
#3133=FACE_OUTER_BOUND('',#4499,.T.);
#3134=FACE_OUTER_BOUND('',#4500,.T.);
#3135=FACE_OUTER_BOUND('',#4501,.T.);
#3136=FACE_OUTER_BOUND('',#4502,.T.);
#3137=FACE_OUTER_BOUND('',#4504,.T.);
#3138=FACE_OUTER_BOUND('',#4505,.T.);
#3139=FACE_OUTER_BOUND('',#4507,.T.);
#3140=FACE_OUTER_BOUND('',#4508,.T.);
#3141=FACE_OUTER_BOUND('',#4510,.T.);
#3142=FACE_OUTER_BOUND('',#4511,.T.);
#3143=FACE_OUTER_BOUND('',#4512,.T.);
#3144=FACE_OUTER_BOUND('',#4513,.T.);
#3145=FACE_OUTER_BOUND('',#4515,.T.);
#3146=FACE_OUTER_BOUND('',#4517,.T.);
#3147=FACE_OUTER_BOUND('',#4518,.T.);
#3148=FACE_OUTER_BOUND('',#4519,.T.);
#3149=FACE_OUTER_BOUND('',#4520,.T.);
#3150=FACE_OUTER_BOUND('',#4522,.T.);
#3151=FACE_OUTER_BOUND('',#4524,.T.);
#3152=FACE_OUTER_BOUND('',#4526,.T.);
#3153=FACE_OUTER_BOUND('',#4528,.T.);
#3154=FACE_OUTER_BOUND('',#4529,.T.);
#3155=FACE_OUTER_BOUND('',#4530,.T.);
#3156=FACE_OUTER_BOUND('',#4531,.T.);
#3157=FACE_OUTER_BOUND('',#4532,.T.);
#3158=FACE_OUTER_BOUND('',#4533,.T.);
#3159=FACE_OUTER_BOUND('',#4534,.T.);
#3160=FACE_OUTER_BOUND('',#4535,.T.);
#3161=FACE_OUTER_BOUND('',#4538,.T.);
#3162=FACE_OUTER_BOUND('',#4541,.T.);
#3163=FACE_OUTER_BOUND('',#4542,.T.);
#3164=FACE_OUTER_BOUND('',#4544,.T.);
#3165=FACE_OUTER_BOUND('',#4546,.T.);
#3166=FACE_OUTER_BOUND('',#4547,.T.);
#3167=FACE_OUTER_BOUND('',#4548,.T.);
#3168=FACE_OUTER_BOUND('',#4549,.T.);
#3169=FACE_OUTER_BOUND('',#4551,.T.);
#3170=FACE_OUTER_BOUND('',#4553,.T.);
#3171=FACE_OUTER_BOUND('',#4554,.T.);
#3172=FACE_OUTER_BOUND('',#4555,.T.);
#3173=FACE_OUTER_BOUND('',#4557,.T.);
#3174=FACE_OUTER_BOUND('',#4559,.T.);
#3175=FACE_OUTER_BOUND('',#4560,.T.);
#3176=FACE_OUTER_BOUND('',#4561,.T.);
#3177=FACE_OUTER_BOUND('',#4562,.T.);
#3178=FACE_OUTER_BOUND('',#4563,.T.);
#3179=FACE_OUTER_BOUND('',#4564,.T.);
#3180=FACE_OUTER_BOUND('',#4565,.T.);
#3181=FACE_OUTER_BOUND('',#4566,.T.);
#3182=FACE_OUTER_BOUND('',#4567,.T.);
#3183=FACE_OUTER_BOUND('',#4568,.T.);
#3184=FACE_OUTER_BOUND('',#4569,.T.);
#3185=FACE_OUTER_BOUND('',#4570,.T.);
#3186=FACE_OUTER_BOUND('',#4571,.T.);
#3187=FACE_OUTER_BOUND('',#4572,.T.);
#3188=FACE_OUTER_BOUND('',#4573,.T.);
#3189=FACE_OUTER_BOUND('',#4574,.T.);
#3190=FACE_OUTER_BOUND('',#4575,.T.);
#3191=FACE_OUTER_BOUND('',#4576,.T.);
#3192=FACE_OUTER_BOUND('',#4578,.T.);
#3193=FACE_OUTER_BOUND('',#4579,.T.);
#3194=FACE_OUTER_BOUND('',#4580,.T.);
#3195=FACE_OUTER_BOUND('',#4581,.T.);
#3196=FACE_OUTER_BOUND('',#4582,.T.);
#3197=FACE_OUTER_BOUND('',#4583,.T.);
#3198=FACE_OUTER_BOUND('',#4584,.T.);
#3199=FACE_OUTER_BOUND('',#4586,.T.);
#3200=FACE_OUTER_BOUND('',#4588,.T.);
#3201=FACE_OUTER_BOUND('',#4589,.T.);
#3202=FACE_OUTER_BOUND('',#4590,.T.);
#3203=FACE_OUTER_BOUND('',#4591,.T.);
#3204=FACE_OUTER_BOUND('',#4592,.T.);
#3205=FACE_OUTER_BOUND('',#4594,.T.);
#3206=FACE_OUTER_BOUND('',#4595,.T.);
#3207=FACE_OUTER_BOUND('',#4596,.T.);
#3208=FACE_OUTER_BOUND('',#4597,.T.);
#3209=FACE_OUTER_BOUND('',#4598,.T.);
#3210=FACE_OUTER_BOUND('',#4599,.T.);
#3211=FACE_OUTER_BOUND('',#4600,.T.);
#3212=FACE_OUTER_BOUND('',#4601,.T.);
#3213=FACE_OUTER_BOUND('',#4602,.T.);
#3214=FACE_OUTER_BOUND('',#4603,.T.);
#3215=FACE_OUTER_BOUND('',#4604,.T.);
#3216=FACE_OUTER_BOUND('',#4605,.T.);
#3217=EDGE_LOOP('',(#12217,#12218,#12219,#12220));
#3218=EDGE_LOOP('',(#12221,#12222,#12223,#12224));
#3219=EDGE_LOOP('',(#12225,#12226,#12227,#12228));
#3220=EDGE_LOOP('',(#12229,#12230,#12231,#12232));
#3221=EDGE_LOOP('',(#12233,#12234,#12235,#12236));
#3222=EDGE_LOOP('',(#12237,#12238,#12239,#12240));
#3223=EDGE_LOOP('',(#12241,#12242,#12243,#12244));
#3224=EDGE_LOOP('',(#12245));
#3225=EDGE_LOOP('',(#12246,#12247,#12248,#12249));
#3226=EDGE_LOOP('',(#12250));
#3227=EDGE_LOOP('',(#12251,#12252,#12253,#12254));
#3228=EDGE_LOOP('',(#12255));
#3229=EDGE_LOOP('',(#12256,#12257,#12258,#12259));
#3230=EDGE_LOOP('',(#12260));
#3231=EDGE_LOOP('',(#12261,#12262,#12263,#12264));
#3232=EDGE_LOOP('',(#12265,#12266,#12267,#12268));
#3233=EDGE_LOOP('',(#12269,#12270,#12271,#12272));
#3234=EDGE_LOOP('',(#12273,#12274,#12275,#12276));
#3235=EDGE_LOOP('',(#12277,#12278,#12279,#12280));
#3236=EDGE_LOOP('',(#12281,#12282,#12283,#12284));
#3237=EDGE_LOOP('',(#12285,#12286,#12287,#12288));
#3238=EDGE_LOOP('',(#12289,#12290,#12291,#12292));
#3239=EDGE_LOOP('',(#12293,#12294,#12295,#12296));
#3240=EDGE_LOOP('',(#12297,#12298,#12299,#12300));
#3241=EDGE_LOOP('',(#12301,#12302,#12303,#12304));
#3242=EDGE_LOOP('',(#12305,#12306,#12307,#12308));
#3243=EDGE_LOOP('',(#12309,#12310,#12311,#12312));
#3244=EDGE_LOOP('',(#12313,#12314,#12315,#12316));
#3245=EDGE_LOOP('',(#12317,#12318,#12319,#12320));
#3246=EDGE_LOOP('',(#12321,#12322,#12323,#12324));
#3247=EDGE_LOOP('',(#12325,#12326,#12327,#12328));
#3248=EDGE_LOOP('',(#12329,#12330,#12331,#12332));
#3249=EDGE_LOOP('',(#12333,#12334,#12335,#12336,#12337,#12338,#12339,#12340));
#3250=EDGE_LOOP('',(#12341));
#3251=EDGE_LOOP('',(#12342));
#3252=EDGE_LOOP('',(#12343));
#3253=EDGE_LOOP('',(#12344));
#3254=EDGE_LOOP('',(#12345));
#3255=EDGE_LOOP('',(#12346));
#3256=EDGE_LOOP('',(#12347));
#3257=EDGE_LOOP('',(#12348));
#3258=EDGE_LOOP('',(#12349));
#3259=EDGE_LOOP('',(#12350));
#3260=EDGE_LOOP('',(#12351));
#3261=EDGE_LOOP('',(#12352));
#3262=EDGE_LOOP('',(#12353));
#3263=EDGE_LOOP('',(#12354));
#3264=EDGE_LOOP('',(#12355));
#3265=EDGE_LOOP('',(#12356));
#3266=EDGE_LOOP('',(#12357));
#3267=EDGE_LOOP('',(#12358));
#3268=EDGE_LOOP('',(#12359));
#3269=EDGE_LOOP('',(#12360));
#3270=EDGE_LOOP('',(#12361,#12362,#12363,#12364,#12365,#12366,#12367,#12368));
#3271=EDGE_LOOP('',(#12369));
#3272=EDGE_LOOP('',(#12370));
#3273=EDGE_LOOP('',(#12371));
#3274=EDGE_LOOP('',(#12372));
#3275=EDGE_LOOP('',(#12373));
#3276=EDGE_LOOP('',(#12374));
#3277=EDGE_LOOP('',(#12375));
#3278=EDGE_LOOP('',(#12376));
#3279=EDGE_LOOP('',(#12377));
#3280=EDGE_LOOP('',(#12378));
#3281=EDGE_LOOP('',(#12379));
#3282=EDGE_LOOP('',(#12380));
#3283=EDGE_LOOP('',(#12381));
#3284=EDGE_LOOP('',(#12382));
#3285=EDGE_LOOP('',(#12383));
#3286=EDGE_LOOP('',(#12384));
#3287=EDGE_LOOP('',(#12385,#12386,#12387,#12388));
#3288=EDGE_LOOP('',(#12389,#12390,#12391,#12392));
#3289=EDGE_LOOP('',(#12393,#12394,#12395,#12396));
#3290=EDGE_LOOP('',(#12397,#12398,#12399,#12400));
#3291=EDGE_LOOP('',(#12401,#12402,#12403,#12404));
#3292=EDGE_LOOP('',(#12405,#12406,#12407,#12408));
#3293=EDGE_LOOP('',(#12409,#12410,#12411,#12412));
#3294=EDGE_LOOP('',(#12413,#12414,#12415,#12416));
#3295=EDGE_LOOP('',(#12417,#12418,#12419,#12420));
#3296=EDGE_LOOP('',(#12421,#12422,#12423,#12424));
#3297=EDGE_LOOP('',(#12425,#12426,#12427,#12428));
#3298=EDGE_LOOP('',(#12429,#12430,#12431,#12432));
#3299=EDGE_LOOP('',(#12433,#12434,#12435,#12436));
#3300=EDGE_LOOP('',(#12437,#12438,#12439,#12440));
#3301=EDGE_LOOP('',(#12441,#12442,#12443,#12444));
#3302=EDGE_LOOP('',(#12445,#12446,#12447,#12448));
#3303=EDGE_LOOP('',(#12449,#12450,#12451,#12452));
#3304=EDGE_LOOP('',(#12453,#12454,#12455,#12456));
#3305=EDGE_LOOP('',(#12457,#12458,#12459,#12460));
#3306=EDGE_LOOP('',(#12461,#12462,#12463,#12464));
#3307=EDGE_LOOP('',(#12465,#12466,#12467,#12468));
#3308=EDGE_LOOP('',(#12469,#12470,#12471,#12472));
#3309=EDGE_LOOP('',(#12473,#12474,#12475,#12476));
#3310=EDGE_LOOP('',(#12477,#12478,#12479,#12480));
#3311=EDGE_LOOP('',(#12481,#12482,#12483,#12484));
#3312=EDGE_LOOP('',(#12485,#12486,#12487,#12488));
#3313=EDGE_LOOP('',(#12489,#12490,#12491,#12492));
#3314=EDGE_LOOP('',(#12493,#12494,#12495,#12496));
#3315=EDGE_LOOP('',(#12497,#12498,#12499,#12500));
#3316=EDGE_LOOP('',(#12501,#12502,#12503,#12504));
#3317=EDGE_LOOP('',(#12505,#12506,#12507,#12508));
#3318=EDGE_LOOP('',(#12509));
#3319=EDGE_LOOP('',(#12510));
#3320=EDGE_LOOP('',(#12511));
#3321=EDGE_LOOP('',(#12512));
#3322=EDGE_LOOP('',(#12513,#12514,#12515,#12516));
#3323=EDGE_LOOP('',(#12517));
#3324=EDGE_LOOP('',(#12518));
#3325=EDGE_LOOP('',(#12519));
#3326=EDGE_LOOP('',(#12520));
#3327=EDGE_LOOP('',(#12521));
#3328=EDGE_LOOP('',(#12522));
#3329=EDGE_LOOP('',(#12523,#12524,#12525,#12526));
#3330=EDGE_LOOP('',(#12527));
#3331=EDGE_LOOP('',(#12528));
#3332=EDGE_LOOP('',(#12529));
#3333=EDGE_LOOP('',(#12530));
#3334=EDGE_LOOP('',(#12531,#12532,#12533,#12534));
#3335=EDGE_LOOP('',(#12535));
#3336=EDGE_LOOP('',(#12536));
#3337=EDGE_LOOP('',(#12537));
#3338=EDGE_LOOP('',(#12538));
#3339=EDGE_LOOP('',(#12539));
#3340=EDGE_LOOP('',(#12540));
#3341=EDGE_LOOP('',(#12541,#12542,#12543,#12544));
#3342=EDGE_LOOP('',(#12545,#12546,#12547,#12548));
#3343=EDGE_LOOP('',(#12549,#12550,#12551,#12552));
#3344=EDGE_LOOP('',(#12553));
#3345=EDGE_LOOP('',(#12554,#12555,#12556,#12557));
#3346=EDGE_LOOP('',(#12558));
#3347=EDGE_LOOP('',(#12559,#12560,#12561,#12562));
#3348=EDGE_LOOP('',(#12563));
#3349=EDGE_LOOP('',(#12564,#12565,#12566,#12567));
#3350=EDGE_LOOP('',(#12568));
#3351=EDGE_LOOP('',(#12569,#12570,#12571,#12572));
#3352=EDGE_LOOP('',(#12573,#12574,#12575,#12576));
#3353=EDGE_LOOP('',(#12577));
#3354=EDGE_LOOP('',(#12578));
#3355=EDGE_LOOP('',(#12579,#12580,#12581,#12582));
#3356=EDGE_LOOP('',(#12583,#12584,#12585,#12586));
#3357=EDGE_LOOP('',(#12587));
#3358=EDGE_LOOP('',(#12588));
#3359=EDGE_LOOP('',(#12589,#12590,#12591,#12592));
#3360=EDGE_LOOP('',(#12593));
#3361=EDGE_LOOP('',(#12594));
#3362=EDGE_LOOP('',(#12595,#12596,#12597,#12598));
#3363=EDGE_LOOP('',(#12599));
#3364=EDGE_LOOP('',(#12600));
#3365=EDGE_LOOP('',(#12601,#12602,#12603,#12604));
#3366=EDGE_LOOP('',(#12605,#12606,#12607,#12608));
#3367=EDGE_LOOP('',(#12609,#12610,#12611,#12612));
#3368=EDGE_LOOP('',(#12613));
#3369=EDGE_LOOP('',(#12614,#12615,#12616,#12617));
#3370=EDGE_LOOP('',(#12618));
#3371=EDGE_LOOP('',(#12619,#12620,#12621,#12622));
#3372=EDGE_LOOP('',(#12623));
#3373=EDGE_LOOP('',(#12624,#12625,#12626,#12627));
#3374=EDGE_LOOP('',(#12628));
#3375=EDGE_LOOP('',(#12629,#12630,#12631,#12632));
#3376=EDGE_LOOP('',(#12633,#12634,#12635,#12636));
#3377=EDGE_LOOP('',(#12637));
#3378=EDGE_LOOP('',(#12638));
#3379=EDGE_LOOP('',(#12639,#12640,#12641,#12642));
#3380=EDGE_LOOP('',(#12643,#12644,#12645,#12646));
#3381=EDGE_LOOP('',(#12647));
#3382=EDGE_LOOP('',(#12648));
#3383=EDGE_LOOP('',(#12649,#12650,#12651,#12652));
#3384=EDGE_LOOP('',(#12653));
#3385=EDGE_LOOP('',(#12654));
#3386=EDGE_LOOP('',(#12655,#12656,#12657,#12658));
#3387=EDGE_LOOP('',(#12659));
#3388=EDGE_LOOP('',(#12660));
#3389=EDGE_LOOP('',(#12661,#12662,#12663,#12664));
#3390=EDGE_LOOP('',(#12665));
#3391=EDGE_LOOP('',(#12666,#12667,#12668,#12669));
#3392=EDGE_LOOP('',(#12670));
#3393=EDGE_LOOP('',(#12671,#12672,#12673,#12674));
#3394=EDGE_LOOP('',(#12675,#12676,#12677,#12678));
#3395=EDGE_LOOP('',(#12679,#12680,#12681,#12682));
#3396=EDGE_LOOP('',(#12683));
#3397=EDGE_LOOP('',(#12684));
#3398=EDGE_LOOP('',(#12685,#12686,#12687,#12688));
#3399=EDGE_LOOP('',(#12689,#12690,#12691,#12692));
#3400=EDGE_LOOP('',(#12693));
#3401=EDGE_LOOP('',(#12694));
#3402=EDGE_LOOP('',(#12695,#12696,#12697,#12698));
#3403=EDGE_LOOP('',(#12699,#12700,#12701,#12702));
#3404=EDGE_LOOP('',(#12703,#12704,#12705,#12706));
#3405=EDGE_LOOP('',(#12707));
#3406=EDGE_LOOP('',(#12708));
#3407=EDGE_LOOP('',(#12709,#12710,#12711,#12712));
#3408=EDGE_LOOP('',(#12713,#12714,#12715,#12716));
#3409=EDGE_LOOP('',(#12717,#12718,#12719,#12720,#12721,#12722,#12723,#12724));
#3410=EDGE_LOOP('',(#12725,#12726,#12727));
#3411=EDGE_LOOP('',(#12728,#12729,#12730,#12731,#12732,#12733,#12734,#12735));
#3412=EDGE_LOOP('',(#12736,#12737,#12738));
#3413=EDGE_LOOP('',(#12739,#12740,#12741,#12742,#12743,#12744,#12745,#12746));
#3414=EDGE_LOOP('',(#12747,#12748,#12749,#12750,#12751,#12752,#12753,#12754,
#12755,#12756,#12757,#12758));
#3415=EDGE_LOOP('',(#12759));
#3416=EDGE_LOOP('',(#12760));
#3417=EDGE_LOOP('',(#12761,#12762,#12763,#12764));
#3418=EDGE_LOOP('',(#12765,#12766,#12767,#12768,#12769,#12770));
#3419=EDGE_LOOP('',(#12771,#12772,#12773,#12774));
#3420=EDGE_LOOP('',(#12775));
#3421=EDGE_LOOP('',(#12776));
#3422=EDGE_LOOP('',(#12777,#12778,#12779,#12780,#12781,#12782));
#3423=EDGE_LOOP('',(#12783,#12784,#12785,#12786));
#3424=EDGE_LOOP('',(#12787));
#3425=EDGE_LOOP('',(#12788));
#3426=EDGE_LOOP('',(#12789,#12790,#12791,#12792));
#3427=EDGE_LOOP('',(#12793,#12794,#12795,#12796));
#3428=EDGE_LOOP('',(#12797));
#3429=EDGE_LOOP('',(#12798,#12799,#12800,#12801));
#3430=EDGE_LOOP('',(#12802));
#3431=EDGE_LOOP('',(#12803,#12804,#12805,#12806));
#3432=EDGE_LOOP('',(#12807,#12808,#12809,#12810));
#3433=EDGE_LOOP('',(#12811,#12812,#12813,#12814));
#3434=EDGE_LOOP('',(#12815));
#3435=EDGE_LOOP('',(#12816));
#3436=EDGE_LOOP('',(#12817,#12818,#12819,#12820));
#3437=EDGE_LOOP('',(#12821,#12822,#12823,#12824));
#3438=EDGE_LOOP('',(#12825));
#3439=EDGE_LOOP('',(#12826));
#3440=EDGE_LOOP('',(#12827,#12828,#12829,#12830));
#3441=EDGE_LOOP('',(#12831,#12832,#12833,#12834));
#3442=EDGE_LOOP('',(#12835,#12836,#12837,#12838));
#3443=EDGE_LOOP('',(#12839));
#3444=EDGE_LOOP('',(#12840));
#3445=EDGE_LOOP('',(#12841,#12842,#12843,#12844));
#3446=EDGE_LOOP('',(#12845,#12846,#12847,#12848));
#3447=EDGE_LOOP('',(#12849,#12850,#12851,#12852,#12853,#12854,#12855,#12856));
#3448=EDGE_LOOP('',(#12857,#12858,#12859));
#3449=EDGE_LOOP('',(#12860,#12861,#12862,#12863,#12864,#12865,#12866,#12867));
#3450=EDGE_LOOP('',(#12868,#12869,#12870));
#3451=EDGE_LOOP('',(#12871,#12872,#12873,#12874,#12875,#12876,#12877,#12878));
#3452=EDGE_LOOP('',(#12879,#12880,#12881,#12882,#12883,#12884,#12885,#12886,
#12887,#12888,#12889,#12890));
#3453=EDGE_LOOP('',(#12891));
#3454=EDGE_LOOP('',(#12892));
#3455=EDGE_LOOP('',(#12893,#12894,#12895,#12896));
#3456=EDGE_LOOP('',(#12897,#12898,#12899,#12900,#12901,#12902));
#3457=EDGE_LOOP('',(#12903,#12904,#12905,#12906));
#3458=EDGE_LOOP('',(#12907));
#3459=EDGE_LOOP('',(#12908));
#3460=EDGE_LOOP('',(#12909,#12910,#12911,#12912,#12913,#12914));
#3461=EDGE_LOOP('',(#12915,#12916,#12917,#12918));
#3462=EDGE_LOOP('',(#12919));
#3463=EDGE_LOOP('',(#12920));
#3464=EDGE_LOOP('',(#12921,#12922,#12923,#12924));
#3465=EDGE_LOOP('',(#12925,#12926,#12927,#12928));
#3466=EDGE_LOOP('',(#12929,#12930,#12931,#12932));
#3467=EDGE_LOOP('',(#12933,#12934,#12935,#12936));
#3468=EDGE_LOOP('',(#12937,#12938,#12939,#12940));
#3469=EDGE_LOOP('',(#12941));
#3470=EDGE_LOOP('',(#12942,#12943,#12944,#12945));
#3471=EDGE_LOOP('',(#12946));
#3472=EDGE_LOOP('',(#12947,#12948,#12949,#12950));
#3473=EDGE_LOOP('',(#12951));
#3474=EDGE_LOOP('',(#12952,#12953,#12954,#12955));
#3475=EDGE_LOOP('',(#12956));
#3476=EDGE_LOOP('',(#12957,#12958,#12959,#12960));
#3477=EDGE_LOOP('',(#12961));
#3478=EDGE_LOOP('',(#12962));
#3479=EDGE_LOOP('',(#12963,#12964,#12965,#12966));
#3480=EDGE_LOOP('',(#12967,#12968,#12969,#12970));
#3481=EDGE_LOOP('',(#12971));
#3482=EDGE_LOOP('',(#12972));
#3483=EDGE_LOOP('',(#12973));
#3484=EDGE_LOOP('',(#12974));
#3485=EDGE_LOOP('',(#12975));
#3486=EDGE_LOOP('',(#12976,#12977,#12978,#12979));
#3487=EDGE_LOOP('',(#12980,#12981,#12982,#12983));
#3488=EDGE_LOOP('',(#12984,#12985,#12986,#12987));
#3489=EDGE_LOOP('',(#12988,#12989,#12990,#12991));
#3490=EDGE_LOOP('',(#12992,#12993,#12994,#12995));
#3491=EDGE_LOOP('',(#12996));
#3492=EDGE_LOOP('',(#12997));
#3493=EDGE_LOOP('',(#12998));
#3494=EDGE_LOOP('',(#12999));
#3495=EDGE_LOOP('',(#13000,#13001,#13002,#13003));
#3496=EDGE_LOOP('',(#13004));
#3497=EDGE_LOOP('',(#13005));
#3498=EDGE_LOOP('',(#13006));
#3499=EDGE_LOOP('',(#13007));
#3500=EDGE_LOOP('',(#13008));
#3501=EDGE_LOOP('',(#13009,#13010,#13011,#13012));
#3502=EDGE_LOOP('',(#13013,#13014,#13015,#13016));
#3503=EDGE_LOOP('',(#13017,#13018,#13019,#13020));
#3504=EDGE_LOOP('',(#13021,#13022,#13023,#13024));
#3505=EDGE_LOOP('',(#13025,#13026,#13027,#13028));
#3506=EDGE_LOOP('',(#13029,#13030,#13031,#13032));
#3507=EDGE_LOOP('',(#13033));
#3508=EDGE_LOOP('',(#13034,#13035,#13036,#13037));
#3509=EDGE_LOOP('',(#13038));
#3510=EDGE_LOOP('',(#13039,#13040,#13041,#13042));
#3511=EDGE_LOOP('',(#13043));
#3512=EDGE_LOOP('',(#13044,#13045,#13046,#13047));
#3513=EDGE_LOOP('',(#13048));
#3514=EDGE_LOOP('',(#13049,#13050,#13051,#13052));
#3515=EDGE_LOOP('',(#13053));
#3516=EDGE_LOOP('',(#13054));
#3517=EDGE_LOOP('',(#13055,#13056,#13057,#13058));
#3518=EDGE_LOOP('',(#13059,#13060,#13061,#13062));
#3519=EDGE_LOOP('',(#13063,#13064,#13065,#13066));
#3520=EDGE_LOOP('',(#13067,#13068,#13069,#13070));
#3521=EDGE_LOOP('',(#13071));
#3522=EDGE_LOOP('',(#13072));
#3523=EDGE_LOOP('',(#13073,#13074,#13075,#13076,#13077,#13078));
#3524=EDGE_LOOP('',(#13079));
#3525=EDGE_LOOP('',(#13080));
#3526=EDGE_LOOP('',(#13081));
#3527=EDGE_LOOP('',(#13082));
#3528=EDGE_LOOP('',(#13083));
#3529=EDGE_LOOP('',(#13084));
#3530=EDGE_LOOP('',(#13085,#13086,#13087,#13088));
#3531=EDGE_LOOP('',(#13089,#13090,#13091,#13092));
#3532=EDGE_LOOP('',(#13093,#13094,#13095,#13096));
#3533=EDGE_LOOP('',(#13097));
#3534=EDGE_LOOP('',(#13098));
#3535=EDGE_LOOP('',(#13099,#13100,#13101,#13102,#13103,#13104));
#3536=EDGE_LOOP('',(#13105));
#3537=EDGE_LOOP('',(#13106));
#3538=EDGE_LOOP('',(#13107));
#3539=EDGE_LOOP('',(#13108));
#3540=EDGE_LOOP('',(#13109));
#3541=EDGE_LOOP('',(#13110));
#3542=EDGE_LOOP('',(#13111,#13112,#13113,#13114));
#3543=EDGE_LOOP('',(#13115,#13116,#13117,#13118));
#3544=EDGE_LOOP('',(#13119,#13120,#13121,#13122));
#3545=EDGE_LOOP('',(#13123,#13124,#13125,#13126));
#3546=EDGE_LOOP('',(#13127));
#3547=EDGE_LOOP('',(#13128));
#3548=EDGE_LOOP('',(#13129,#13130,#13131,#13132));
#3549=EDGE_LOOP('',(#13133,#13134,#13135,#13136));
#3550=EDGE_LOOP('',(#13137));
#3551=EDGE_LOOP('',(#13138));
#3552=EDGE_LOOP('',(#13139));
#3553=EDGE_LOOP('',(#13140));
#3554=EDGE_LOOP('',(#13141));
#3555=EDGE_LOOP('',(#13142));
#3556=EDGE_LOOP('',(#13143));
#3557=EDGE_LOOP('',(#13144));
#3558=EDGE_LOOP('',(#13145));
#3559=EDGE_LOOP('',(#13146));
#3560=EDGE_LOOP('',(#13147,#13148,#13149,#13150));
#3561=EDGE_LOOP('',(#13151,#13152,#13153,#13154));
#3562=EDGE_LOOP('',(#13155,#13156,#13157,#13158));
#3563=EDGE_LOOP('',(#13159,#13160,#13161,#13162));
#3564=EDGE_LOOP('',(#13163));
#3565=EDGE_LOOP('',(#13164));
#3566=EDGE_LOOP('',(#13165,#13166,#13167,#13168));
#3567=EDGE_LOOP('',(#13169,#13170,#13171,#13172));
#3568=EDGE_LOOP('',(#13173));
#3569=EDGE_LOOP('',(#13174));
#3570=EDGE_LOOP('',(#13175));
#3571=EDGE_LOOP('',(#13176));
#3572=EDGE_LOOP('',(#13177));
#3573=EDGE_LOOP('',(#13178));
#3574=EDGE_LOOP('',(#13179));
#3575=EDGE_LOOP('',(#13180));
#3576=EDGE_LOOP('',(#13181));
#3577=EDGE_LOOP('',(#13182));
#3578=EDGE_LOOP('',(#13183,#13184,#13185,#13186));
#3579=EDGE_LOOP('',(#13187));
#3580=EDGE_LOOP('',(#13188,#13189,#13190,#13191));
#3581=EDGE_LOOP('',(#13192));
#3582=EDGE_LOOP('',(#13193));
#3583=EDGE_LOOP('',(#13194));
#3584=EDGE_LOOP('',(#13195,#13196,#13197,#13198));
#3585=EDGE_LOOP('',(#13199));
#3586=EDGE_LOOP('',(#13200,#13201,#13202,#13203));
#3587=EDGE_LOOP('',(#13204));
#3588=EDGE_LOOP('',(#13205));
#3589=EDGE_LOOP('',(#13206));
#3590=EDGE_LOOP('',(#13207,#13208,#13209,#13210));
#3591=EDGE_LOOP('',(#13211));
#3592=EDGE_LOOP('',(#13212,#13213,#13214,#13215));
#3593=EDGE_LOOP('',(#13216));
#3594=EDGE_LOOP('',(#13217));
#3595=EDGE_LOOP('',(#13218));
#3596=EDGE_LOOP('',(#13219,#13220,#13221,#13222));
#3597=EDGE_LOOP('',(#13223));
#3598=EDGE_LOOP('',(#13224,#13225,#13226,#13227));
#3599=EDGE_LOOP('',(#13228));
#3600=EDGE_LOOP('',(#13229));
#3601=EDGE_LOOP('',(#13230));
#3602=EDGE_LOOP('',(#13231,#13232,#13233,#13234));
#3603=EDGE_LOOP('',(#13235));
#3604=EDGE_LOOP('',(#13236));
#3605=EDGE_LOOP('',(#13237,#13238,#13239,#13240));
#3606=EDGE_LOOP('',(#13241));
#3607=EDGE_LOOP('',(#13242));
#3608=EDGE_LOOP('',(#13243,#13244,#13245,#13246));
#3609=EDGE_LOOP('',(#13247));
#3610=EDGE_LOOP('',(#13248));
#3611=EDGE_LOOP('',(#13249,#13250,#13251,#13252));
#3612=EDGE_LOOP('',(#13253));
#3613=EDGE_LOOP('',(#13254));
#3614=EDGE_LOOP('',(#13255,#13256,#13257,#13258));
#3615=EDGE_LOOP('',(#13259,#13260,#13261,#13262));
#3616=EDGE_LOOP('',(#13263,#13264,#13265,#13266));
#3617=EDGE_LOOP('',(#13267,#13268,#13269,#13270));
#3618=EDGE_LOOP('',(#13271,#13272,#13273,#13274));
#3619=EDGE_LOOP('',(#13275));
#3620=EDGE_LOOP('',(#13276));
#3621=EDGE_LOOP('',(#13277));
#3622=EDGE_LOOP('',(#13278));
#3623=EDGE_LOOP('',(#13279));
#3624=EDGE_LOOP('',(#13280));
#3625=EDGE_LOOP('',(#13281));
#3626=EDGE_LOOP('',(#13282));
#3627=EDGE_LOOP('',(#13283));
#3628=EDGE_LOOP('',(#13284));
#3629=EDGE_LOOP('',(#13285,#13286,#13287,#13288));
#3630=EDGE_LOOP('',(#13289,#13290,#13291,#13292));
#3631=EDGE_LOOP('',(#13293,#13294,#13295,#13296));
#3632=EDGE_LOOP('',(#13297,#13298,#13299,#13300));
#3633=EDGE_LOOP('',(#13301,#13302,#13303,#13304));
#3634=EDGE_LOOP('',(#13305,#13306,#13307,#13308));
#3635=EDGE_LOOP('',(#13309,#13310,#13311,#13312));
#3636=EDGE_LOOP('',(#13313,#13314,#13315,#13316));
#3637=EDGE_LOOP('',(#13317,#13318,#13319,#13320));
#3638=EDGE_LOOP('',(#13321,#13322,#13323,#13324));
#3639=EDGE_LOOP('',(#13325,#13326,#13327,#13328));
#3640=EDGE_LOOP('',(#13329,#13330,#13331,#13332));
#3641=EDGE_LOOP('',(#13333,#13334,#13335,#13336));
#3642=EDGE_LOOP('',(#13337,#13338,#13339,#13340));
#3643=EDGE_LOOP('',(#13341,#13342,#13343,#13344));
#3644=EDGE_LOOP('',(#13345,#13346,#13347,#13348));
#3645=EDGE_LOOP('',(#13349,#13350,#13351,#13352));
#3646=EDGE_LOOP('',(#13353,#13354,#13355,#13356));
#3647=EDGE_LOOP('',(#13357,#13358,#13359,#13360));
#3648=EDGE_LOOP('',(#13361,#13362,#13363,#13364));
#3649=EDGE_LOOP('',(#13365,#13366,#13367,#13368));
#3650=EDGE_LOOP('',(#13369,#13370,#13371,#13372));
#3651=EDGE_LOOP('',(#13373,#13374,#13375,#13376));
#3652=EDGE_LOOP('',(#13377,#13378,#13379,#13380));
#3653=EDGE_LOOP('',(#13381,#13382,#13383,#13384));
#3654=EDGE_LOOP('',(#13385,#13386,#13387,#13388));
#3655=EDGE_LOOP('',(#13389,#13390,#13391,#13392));
#3656=EDGE_LOOP('',(#13393,#13394,#13395,#13396));
#3657=EDGE_LOOP('',(#13397,#13398,#13399,#13400));
#3658=EDGE_LOOP('',(#13401,#13402,#13403,#13404));
#3659=EDGE_LOOP('',(#13405,#13406,#13407,#13408));
#3660=EDGE_LOOP('',(#13409,#13410,#13411,#13412));
#3661=EDGE_LOOP('',(#13413,#13414,#13415,#13416));
#3662=EDGE_LOOP('',(#13417,#13418,#13419,#13420));
#3663=EDGE_LOOP('',(#13421,#13422,#13423,#13424));
#3664=EDGE_LOOP('',(#13425,#13426,#13427,#13428));
#3665=EDGE_LOOP('',(#13429,#13430,#13431,#13432));
#3666=EDGE_LOOP('',(#13433,#13434,#13435,#13436));
#3667=EDGE_LOOP('',(#13437,#13438,#13439,#13440));
#3668=EDGE_LOOP('',(#13441,#13442,#13443,#13444));
#3669=EDGE_LOOP('',(#13445,#13446,#13447,#13448));
#3670=EDGE_LOOP('',(#13449,#13450,#13451,#13452));
#3671=EDGE_LOOP('',(#13453,#13454,#13455,#13456));
#3672=EDGE_LOOP('',(#13457,#13458,#13459,#13460));
#3673=EDGE_LOOP('',(#13461,#13462,#13463,#13464));
#3674=EDGE_LOOP('',(#13465,#13466,#13467,#13468));
#3675=EDGE_LOOP('',(#13469,#13470,#13471,#13472));
#3676=EDGE_LOOP('',(#13473,#13474,#13475,#13476));
#3677=EDGE_LOOP('',(#13477,#13478,#13479,#13480));
#3678=EDGE_LOOP('',(#13481,#13482,#13483,#13484));
#3679=EDGE_LOOP('',(#13485,#13486,#13487,#13488));
#3680=EDGE_LOOP('',(#13489,#13490,#13491,#13492));
#3681=EDGE_LOOP('',(#13493,#13494,#13495,#13496));
#3682=EDGE_LOOP('',(#13497,#13498,#13499,#13500));
#3683=EDGE_LOOP('',(#13501,#13502,#13503,#13504));
#3684=EDGE_LOOP('',(#13505,#13506,#13507,#13508));
#3685=EDGE_LOOP('',(#13509,#13510,#13511,#13512));
#3686=EDGE_LOOP('',(#13513,#13514,#13515,#13516));
#3687=EDGE_LOOP('',(#13517,#13518,#13519,#13520));
#3688=EDGE_LOOP('',(#13521,#13522,#13523,#13524));
#3689=EDGE_LOOP('',(#13525,#13526,#13527,#13528));
#3690=EDGE_LOOP('',(#13529,#13530,#13531,#13532));
#3691=EDGE_LOOP('',(#13533,#13534,#13535,#13536));
#3692=EDGE_LOOP('',(#13537,#13538,#13539,#13540));
#3693=EDGE_LOOP('',(#13541,#13542,#13543,#13544));
#3694=EDGE_LOOP('',(#13545,#13546,#13547,#13548));
#3695=EDGE_LOOP('',(#13549,#13550,#13551,#13552));
#3696=EDGE_LOOP('',(#13553,#13554,#13555,#13556));
#3697=EDGE_LOOP('',(#13557,#13558,#13559,#13560));
#3698=EDGE_LOOP('',(#13561,#13562,#13563,#13564));
#3699=EDGE_LOOP('',(#13565,#13566,#13567,#13568));
#3700=EDGE_LOOP('',(#13569,#13570,#13571,#13572));
#3701=EDGE_LOOP('',(#13573,#13574,#13575,#13576));
#3702=EDGE_LOOP('',(#13577,#13578,#13579,#13580));
#3703=EDGE_LOOP('',(#13581,#13582,#13583,#13584));
#3704=EDGE_LOOP('',(#13585,#13586,#13587,#13588));
#3705=EDGE_LOOP('',(#13589,#13590,#13591,#13592));
#3706=EDGE_LOOP('',(#13593,#13594,#13595,#13596));
#3707=EDGE_LOOP('',(#13597,#13598,#13599,#13600));
#3708=EDGE_LOOP('',(#13601,#13602,#13603,#13604));
#3709=EDGE_LOOP('',(#13605,#13606,#13607,#13608));
#3710=EDGE_LOOP('',(#13609,#13610,#13611,#13612));
#3711=EDGE_LOOP('',(#13613,#13614,#13615,#13616));
#3712=EDGE_LOOP('',(#13617,#13618,#13619,#13620));
#3713=EDGE_LOOP('',(#13621,#13622,#13623,#13624));
#3714=EDGE_LOOP('',(#13625,#13626,#13627,#13628));
#3715=EDGE_LOOP('',(#13629,#13630,#13631,#13632));
#3716=EDGE_LOOP('',(#13633,#13634,#13635,#13636));
#3717=EDGE_LOOP('',(#13637,#13638,#13639,#13640));
#3718=EDGE_LOOP('',(#13641,#13642,#13643,#13644));
#3719=EDGE_LOOP('',(#13645,#13646,#13647,#13648));
#3720=EDGE_LOOP('',(#13649,#13650,#13651,#13652));
#3721=EDGE_LOOP('',(#13653,#13654,#13655,#13656));
#3722=EDGE_LOOP('',(#13657,#13658,#13659,#13660));
#3723=EDGE_LOOP('',(#13661,#13662,#13663,#13664));
#3724=EDGE_LOOP('',(#13665,#13666,#13667,#13668));
#3725=EDGE_LOOP('',(#13669,#13670,#13671,#13672));
#3726=EDGE_LOOP('',(#13673,#13674,#13675,#13676));
#3727=EDGE_LOOP('',(#13677,#13678,#13679,#13680));
#3728=EDGE_LOOP('',(#13681,#13682,#13683,#13684));
#3729=EDGE_LOOP('',(#13685,#13686,#13687,#13688));
#3730=EDGE_LOOP('',(#13689,#13690,#13691,#13692));
#3731=EDGE_LOOP('',(#13693,#13694,#13695,#13696));
#3732=EDGE_LOOP('',(#13697,#13698,#13699,#13700));
#3733=EDGE_LOOP('',(#13701,#13702,#13703,#13704));
#3734=EDGE_LOOP('',(#13705,#13706,#13707,#13708));
#3735=EDGE_LOOP('',(#13709,#13710,#13711,#13712));
#3736=EDGE_LOOP('',(#13713,#13714,#13715,#13716));
#3737=EDGE_LOOP('',(#13717,#13718,#13719,#13720));
#3738=EDGE_LOOP('',(#13721,#13722,#13723,#13724));
#3739=EDGE_LOOP('',(#13725,#13726,#13727,#13728));
#3740=EDGE_LOOP('',(#13729,#13730,#13731,#13732));
#3741=EDGE_LOOP('',(#13733,#13734,#13735,#13736));
#3742=EDGE_LOOP('',(#13737,#13738,#13739,#13740));
#3743=EDGE_LOOP('',(#13741,#13742,#13743,#13744));
#3744=EDGE_LOOP('',(#13745,#13746,#13747,#13748));
#3745=EDGE_LOOP('',(#13749,#13750,#13751,#13752));
#3746=EDGE_LOOP('',(#13753,#13754,#13755,#13756));
#3747=EDGE_LOOP('',(#13757,#13758,#13759,#13760));
#3748=EDGE_LOOP('',(#13761,#13762,#13763,#13764));
#3749=EDGE_LOOP('',(#13765,#13766,#13767,#13768));
#3750=EDGE_LOOP('',(#13769,#13770,#13771,#13772));
#3751=EDGE_LOOP('',(#13773,#13774,#13775,#13776));
#3752=EDGE_LOOP('',(#13777,#13778,#13779,#13780));
#3753=EDGE_LOOP('',(#13781,#13782,#13783,#13784));
#3754=EDGE_LOOP('',(#13785,#13786,#13787,#13788));
#3755=EDGE_LOOP('',(#13789,#13790,#13791,#13792));
#3756=EDGE_LOOP('',(#13793,#13794,#13795,#13796));
#3757=EDGE_LOOP('',(#13797,#13798,#13799,#13800));
#3758=EDGE_LOOP('',(#13801));
#3759=EDGE_LOOP('',(#13802));
#3760=EDGE_LOOP('',(#13803,#13804,#13805,#13806));
#3761=EDGE_LOOP('',(#13807,#13808,#13809,#13810));
#3762=EDGE_LOOP('',(#13811,#13812,#13813,#13814));
#3763=EDGE_LOOP('',(#13815,#13816,#13817,#13818));
#3764=EDGE_LOOP('',(#13819,#13820,#13821,#13822));
#3765=EDGE_LOOP('',(#13823,#13824,#13825,#13826));
#3766=EDGE_LOOP('',(#13827,#13828,#13829,#13830));
#3767=EDGE_LOOP('',(#13831,#13832,#13833,#13834));
#3768=EDGE_LOOP('',(#13835,#13836,#13837,#13838));
#3769=EDGE_LOOP('',(#13839,#13840,#13841,#13842));
#3770=EDGE_LOOP('',(#13843,#13844,#13845,#13846));
#3771=EDGE_LOOP('',(#13847,#13848,#13849,#13850));
#3772=EDGE_LOOP('',(#13851,#13852,#13853,#13854));
#3773=EDGE_LOOP('',(#13855,#13856,#13857,#13858));
#3774=EDGE_LOOP('',(#13859,#13860,#13861,#13862));
#3775=EDGE_LOOP('',(#13863,#13864,#13865,#13866));
#3776=EDGE_LOOP('',(#13867,#13868,#13869,#13870));
#3777=EDGE_LOOP('',(#13871));
#3778=EDGE_LOOP('',(#13872));
#3779=EDGE_LOOP('',(#13873,#13874,#13875,#13876));
#3780=EDGE_LOOP('',(#13877,#13878,#13879,#13880));
#3781=EDGE_LOOP('',(#13881,#13882,#13883,#13884));
#3782=EDGE_LOOP('',(#13885,#13886,#13887,#13888));
#3783=EDGE_LOOP('',(#13889,#13890,#13891,#13892));
#3784=EDGE_LOOP('',(#13893,#13894,#13895,#13896));
#3785=EDGE_LOOP('',(#13897,#13898,#13899,#13900));
#3786=EDGE_LOOP('',(#13901,#13902,#13903,#13904));
#3787=EDGE_LOOP('',(#13905,#13906,#13907,#13908));
#3788=EDGE_LOOP('',(#13909,#13910,#13911,#13912));
#3789=EDGE_LOOP('',(#13913,#13914,#13915,#13916));
#3790=EDGE_LOOP('',(#13917,#13918,#13919,#13920));
#3791=EDGE_LOOP('',(#13921,#13922,#13923,#13924));
#3792=EDGE_LOOP('',(#13925,#13926,#13927,#13928));
#3793=EDGE_LOOP('',(#13929));
#3794=EDGE_LOOP('',(#13930,#13931,#13932,#13933));
#3795=EDGE_LOOP('',(#13934));
#3796=EDGE_LOOP('',(#13935,#13936));
#3797=EDGE_LOOP('',(#13937,#13938,#13939,#13940));
#3798=EDGE_LOOP('',(#13941,#13942,#13943,#13944));
#3799=EDGE_LOOP('',(#13945,#13946));
#3800=EDGE_LOOP('',(#13947,#13948,#13949,#13950,#13951,#13952));
#3801=EDGE_LOOP('',(#13953));
#3802=EDGE_LOOP('',(#13954,#13955,#13956,#13957,#13958,#13959,#13960,#13961));
#3803=EDGE_LOOP('',(#13962));
#3804=EDGE_LOOP('',(#13963,#13964,#13965,#13966,#13967,#13968));
#3805=EDGE_LOOP('',(#13969));
#3806=EDGE_LOOP('',(#13970,#13971,#13972,#13973));
#3807=EDGE_LOOP('',(#13974,#13975,#13976,#13977));
#3808=EDGE_LOOP('',(#13978,#13979,#13980,#13981));
#3809=EDGE_LOOP('',(#13982,#13983,#13984,#13985));
#3810=EDGE_LOOP('',(#13986,#13987,#13988,#13989));
#3811=EDGE_LOOP('',(#13990,#13991,#13992,#13993,#13994,#13995,#13996,#13997,
#13998,#13999,#14000,#14001));
#3812=EDGE_LOOP('',(#14002));
#3813=EDGE_LOOP('',(#14003,#14004,#14005,#14006));
#3814=EDGE_LOOP('',(#14007,#14008,#14009,#14010));
#3815=EDGE_LOOP('',(#14011));
#3816=EDGE_LOOP('',(#14012));
#3817=EDGE_LOOP('',(#14013,#14014,#14015,#14016));
#3818=EDGE_LOOP('',(#14017,#14018,#14019,#14020,#14021,#14022,#14023,#14024));
#3819=EDGE_LOOP('',(#14025));
#3820=EDGE_LOOP('',(#14026,#14027,#14028,#14029));
#3821=EDGE_LOOP('',(#14030,#14031,#14032,#14033));
#3822=EDGE_LOOP('',(#14034));
#3823=EDGE_LOOP('',(#14035,#14036,#14037,#14038));
#3824=EDGE_LOOP('',(#14039,#14040,#14041,#14042));
#3825=EDGE_LOOP('',(#14043));
#3826=EDGE_LOOP('',(#14044,#14045,#14046,#14047));
#3827=EDGE_LOOP('',(#14048,#14049,#14050,#14051,#14052,#14053,#14054,#14055,
#14056,#14057,#14058,#14059));
#3828=EDGE_LOOP('',(#14060));
#3829=EDGE_LOOP('',(#14061,#14062,#14063,#14064));
#3830=EDGE_LOOP('',(#14065,#14066,#14067,#14068));
#3831=EDGE_LOOP('',(#14069,#14070,#14071,#14072));
#3832=EDGE_LOOP('',(#14073,#14074,#14075,#14076));
#3833=EDGE_LOOP('',(#14077,#14078,#14079,#14080));
#3834=EDGE_LOOP('',(#14081,#14082,#14083,#14084));
#3835=EDGE_LOOP('',(#14085,#14086,#14087,#14088,#14089,#14090));
#3836=EDGE_LOOP('',(#14091,#14092,#14093,#14094,#14095,#14096));
#3837=EDGE_LOOP('',(#14097));
#3838=EDGE_LOOP('',(#14098));
#3839=EDGE_LOOP('',(#14099,#14100,#14101,#14102));
#3840=EDGE_LOOP('',(#14103,#14104,#14105,#14106));
#3841=EDGE_LOOP('',(#14107,#14108,#14109,#14110));
#3842=EDGE_LOOP('',(#14111));
#3843=EDGE_LOOP('',(#14112));
#3844=EDGE_LOOP('',(#14113,#14114,#14115,#14116));
#3845=EDGE_LOOP('',(#14117,#14118,#14119,#14120));
#3846=EDGE_LOOP('',(#14121,#14122,#14123,#14124,#14125,#14126));
#3847=EDGE_LOOP('',(#14127,#14128,#14129,#14130,#14131));
#3848=EDGE_LOOP('',(#14132,#14133,#14134,#14135));
#3849=EDGE_LOOP('',(#14136,#14137,#14138,#14139));
#3850=EDGE_LOOP('',(#14140));
#3851=EDGE_LOOP('',(#14141));
#3852=EDGE_LOOP('',(#14142,#14143,#14144,#14145,#14146));
#3853=EDGE_LOOP('',(#14147));
#3854=EDGE_LOOP('',(#14148));
#3855=EDGE_LOOP('',(#14149,#14150,#14151,#14152));
#3856=EDGE_LOOP('',(#14153,#14154,#14155,#14156,#14157,#14158));
#3857=EDGE_LOOP('',(#14159,#14160,#14161,#14162,#14163));
#3858=EDGE_LOOP('',(#14164));
#3859=EDGE_LOOP('',(#14165));
#3860=EDGE_LOOP('',(#14166,#14167,#14168,#14169));
#3861=EDGE_LOOP('',(#14170,#14171,#14172,#14173));
#3862=EDGE_LOOP('',(#14174,#14175,#14176,#14177));
#3863=EDGE_LOOP('',(#14178));
#3864=EDGE_LOOP('',(#14179));
#3865=EDGE_LOOP('',(#14180,#14181,#14182,#14183,#14184));
#3866=EDGE_LOOP('',(#14185,#14186));
#3867=EDGE_LOOP('',(#14187,#14188));
#3868=EDGE_LOOP('',(#14189,#14190));
#3869=EDGE_LOOP('',(#14191,#14192));
#3870=EDGE_LOOP('',(#14193,#14194));
#3871=EDGE_LOOP('',(#14195,#14196));
#3872=EDGE_LOOP('',(#14197,#14198));
#3873=EDGE_LOOP('',(#14199,#14200,#14201,#14202));
#3874=EDGE_LOOP('',(#14203,#14204,#14205,#14206,#14207,#14208,#14209,#14210,
#14211,#14212,#14213,#14214,#14215,#14216,#14217,#14218,#14219,#14220));
#3875=EDGE_LOOP('',(#14221,#14222,#14223,#14224));
#3876=EDGE_LOOP('',(#14225,#14226,#14227,#14228));
#3877=EDGE_LOOP('',(#14229,#14230,#14231,#14232));
#3878=EDGE_LOOP('',(#14233,#14234,#14235,#14236));
#3879=EDGE_LOOP('',(#14237,#14238,#14239,#14240,#14241,#14242));
#3880=EDGE_LOOP('',(#14243,#14244,#14245,#14246));
#3881=EDGE_LOOP('',(#14247,#14248,#14249,#14250));
#3882=EDGE_LOOP('',(#14251,#14252,#14253,#14254));
#3883=EDGE_LOOP('',(#14255,#14256,#14257,#14258));
#3884=EDGE_LOOP('',(#14259,#14260,#14261,#14262));
#3885=EDGE_LOOP('',(#14263,#14264,#14265,#14266,#14267,#14268,#14269,#14270,
#14271,#14272,#14273,#14274,#14275,#14276,#14277,#14278,#14279,#14280));
#3886=EDGE_LOOP('',(#14281,#14282,#14283,#14284));
#3887=EDGE_LOOP('',(#14285,#14286,#14287,#14288));
#3888=EDGE_LOOP('',(#14289));
#3889=EDGE_LOOP('',(#14290));
#3890=EDGE_LOOP('',(#14291,#14292,#14293,#14294));
#3891=EDGE_LOOP('',(#14295));
#3892=EDGE_LOOP('',(#14296));
#3893=EDGE_LOOP('',(#14297,#14298,#14299,#14300));
#3894=EDGE_LOOP('',(#14301));
#3895=EDGE_LOOP('',(#14302));
#3896=EDGE_LOOP('',(#14303,#14304,#14305,#14306));
#3897=EDGE_LOOP('',(#14307));
#3898=EDGE_LOOP('',(#14308));
#3899=EDGE_LOOP('',(#14309,#14310,#14311,#14312));
#3900=EDGE_LOOP('',(#14313));
#3901=EDGE_LOOP('',(#14314));
#3902=EDGE_LOOP('',(#14315,#14316,#14317,#14318));
#3903=EDGE_LOOP('',(#14319,#14320,#14321,#14322,#14323,#14324));
#3904=EDGE_LOOP('',(#14325,#14326,#14327,#14328,#14329));
#3905=EDGE_LOOP('',(#14330,#14331,#14332,#14333));
#3906=EDGE_LOOP('',(#14334,#14335,#14336,#14337));
#3907=EDGE_LOOP('',(#14338));
#3908=EDGE_LOOP('',(#14339));
#3909=EDGE_LOOP('',(#14340,#14341,#14342,#14343,#14344));
#3910=EDGE_LOOP('',(#14345));
#3911=EDGE_LOOP('',(#14346));
#3912=EDGE_LOOP('',(#14347,#14348,#14349,#14350));
#3913=EDGE_LOOP('',(#14351,#14352,#14353,#14354,#14355,#14356));
#3914=EDGE_LOOP('',(#14357,#14358,#14359,#14360,#14361));
#3915=EDGE_LOOP('',(#14362));
#3916=EDGE_LOOP('',(#14363));
#3917=EDGE_LOOP('',(#14364,#14365,#14366,#14367));
#3918=EDGE_LOOP('',(#14368,#14369,#14370,#14371));
#3919=EDGE_LOOP('',(#14372,#14373,#14374,#14375));
#3920=EDGE_LOOP('',(#14376));
#3921=EDGE_LOOP('',(#14377));
#3922=EDGE_LOOP('',(#14378,#14379,#14380,#14381,#14382));
#3923=EDGE_LOOP('',(#14383,#14384));
#3924=EDGE_LOOP('',(#14385,#14386));
#3925=EDGE_LOOP('',(#14387,#14388));
#3926=EDGE_LOOP('',(#14389,#14390));
#3927=EDGE_LOOP('',(#14391,#14392));
#3928=EDGE_LOOP('',(#14393,#14394));
#3929=EDGE_LOOP('',(#14395,#14396));
#3930=EDGE_LOOP('',(#14397,#14398));
#3931=EDGE_LOOP('',(#14399,#14400,#14401,#14402));
#3932=EDGE_LOOP('',(#14403,#14404,#14405,#14406,#14407,#14408,#14409,#14410,
#14411,#14412,#14413,#14414,#14415,#14416,#14417,#14418,#14419,#14420,#14421,
#14422));
#3933=EDGE_LOOP('',(#14423,#14424,#14425,#14426));
#3934=EDGE_LOOP('',(#14427,#14428,#14429,#14430));
#3935=EDGE_LOOP('',(#14431,#14432,#14433,#14434));
#3936=EDGE_LOOP('',(#14435,#14436,#14437,#14438));
#3937=EDGE_LOOP('',(#14439,#14440,#14441,#14442));
#3938=EDGE_LOOP('',(#14443,#14444,#14445,#14446,#14447,#14448));
#3939=EDGE_LOOP('',(#14449,#14450,#14451,#14452));
#3940=EDGE_LOOP('',(#14453,#14454,#14455,#14456));
#3941=EDGE_LOOP('',(#14457,#14458,#14459,#14460));
#3942=EDGE_LOOP('',(#14461,#14462,#14463,#14464));
#3943=EDGE_LOOP('',(#14465,#14466,#14467,#14468));
#3944=EDGE_LOOP('',(#14469,#14470,#14471,#14472));
#3945=EDGE_LOOP('',(#14473,#14474,#14475,#14476,#14477,#14478,#14479,#14480,
#14481,#14482,#14483,#14484,#14485,#14486,#14487,#14488,#14489,#14490,#14491,
#14492));
#3946=EDGE_LOOP('',(#14493,#14494,#14495,#14496));
#3947=EDGE_LOOP('',(#14497,#14498,#14499,#14500));
#3948=EDGE_LOOP('',(#14501));
#3949=EDGE_LOOP('',(#14502));
#3950=EDGE_LOOP('',(#14503,#14504,#14505,#14506));
#3951=EDGE_LOOP('',(#14507));
#3952=EDGE_LOOP('',(#14508));
#3953=EDGE_LOOP('',(#14509,#14510,#14511,#14512));
#3954=EDGE_LOOP('',(#14513));
#3955=EDGE_LOOP('',(#14514));
#3956=EDGE_LOOP('',(#14515,#14516,#14517,#14518));
#3957=EDGE_LOOP('',(#14519));
#3958=EDGE_LOOP('',(#14520));
#3959=EDGE_LOOP('',(#14521,#14522,#14523,#14524));
#3960=EDGE_LOOP('',(#14525));
#3961=EDGE_LOOP('',(#14526));
#3962=EDGE_LOOP('',(#14527,#14528,#14529,#14530));
#3963=EDGE_LOOP('',(#14531));
#3964=EDGE_LOOP('',(#14532));
#3965=EDGE_LOOP('',(#14533));
#3966=EDGE_LOOP('',(#14534,#14535,#14536,#14537));
#3967=EDGE_LOOP('',(#14538));
#3968=EDGE_LOOP('',(#14539,#14540,#14541,#14542));
#3969=EDGE_LOOP('',(#14543,#14544,#14545,#14546));
#3970=EDGE_LOOP('',(#14547,#14548,#14549,#14550));
#3971=EDGE_LOOP('',(#14551));
#3972=EDGE_LOOP('',(#14552));
#3973=EDGE_LOOP('',(#14553,#14554,#14555,#14556));
#3974=EDGE_LOOP('',(#14557,#14558,#14559,#14560));
#3975=EDGE_LOOP('',(#14561,#14562,#14563,#14564));
#3976=EDGE_LOOP('',(#14565,#14566,#14567,#14568));
#3977=EDGE_LOOP('',(#14569,#14570,#14571,#14572));
#3978=EDGE_LOOP('',(#14573,#14574,#14575,#14576));
#3979=EDGE_LOOP('',(#14577,#14578,#14579,#14580));
#3980=EDGE_LOOP('',(#14581,#14582,#14583,#14584));
#3981=EDGE_LOOP('',(#14585,#14586,#14587,#14588,#14589,#14590));
#3982=EDGE_LOOP('',(#14591,#14592,#14593,#14594,#14595,#14596));
#3983=EDGE_LOOP('',(#14597,#14598,#14599,#14600));
#3984=EDGE_LOOP('',(#14601,#14602,#14603,#14604));
#3985=EDGE_LOOP('',(#14605,#14606,#14607,#14608));
#3986=EDGE_LOOP('',(#14609,#14610,#14611,#14612));
#3987=EDGE_LOOP('',(#14613,#14614,#14615,#14616));
#3988=EDGE_LOOP('',(#14617,#14618,#14619,#14620));
#3989=EDGE_LOOP('',(#14621,#14622,#14623,#14624,#14625,#14626));
#3990=EDGE_LOOP('',(#14627,#14628,#14629,#14630,#14631,#14632));
#3991=EDGE_LOOP('',(#14633));
#3992=EDGE_LOOP('',(#14634));
#3993=EDGE_LOOP('',(#14635,#14636,#14637,#14638));
#3994=EDGE_LOOP('',(#14639,#14640,#14641,#14642));
#3995=EDGE_LOOP('',(#14643,#14644,#14645,#14646));
#3996=EDGE_LOOP('',(#14647));
#3997=EDGE_LOOP('',(#14648));
#3998=EDGE_LOOP('',(#14649,#14650,#14651,#14652));
#3999=EDGE_LOOP('',(#14653,#14654,#14655,#14656));
#4000=EDGE_LOOP('',(#14657,#14658,#14659,#14660));
#4001=EDGE_LOOP('',(#14661,#14662,#14663,#14664));
#4002=EDGE_LOOP('',(#14665,#14666,#14667,#14668));
#4003=EDGE_LOOP('',(#14669,#14670,#14671,#14672));
#4004=EDGE_LOOP('',(#14673,#14674,#14675,#14676));
#4005=EDGE_LOOP('',(#14677,#14678,#14679,#14680));
#4006=EDGE_LOOP('',(#14681,#14682,#14683,#14684));
#4007=EDGE_LOOP('',(#14685,#14686,#14687,#14688));
#4008=EDGE_LOOP('',(#14689,#14690,#14691,#14692));
#4009=EDGE_LOOP('',(#14693,#14694,#14695,#14696));
#4010=EDGE_LOOP('',(#14697,#14698,#14699,#14700));
#4011=EDGE_LOOP('',(#14701,#14702,#14703,#14704));
#4012=EDGE_LOOP('',(#14705,#14706,#14707,#14708));
#4013=EDGE_LOOP('',(#14709,#14710,#14711,#14712));
#4014=EDGE_LOOP('',(#14713,#14714,#14715,#14716));
#4015=EDGE_LOOP('',(#14717,#14718,#14719,#14720));
#4016=EDGE_LOOP('',(#14721,#14722,#14723,#14724));
#4017=EDGE_LOOP('',(#14725,#14726,#14727,#14728));
#4018=EDGE_LOOP('',(#14729,#14730,#14731,#14732));
#4019=EDGE_LOOP('',(#14733,#14734,#14735,#14736));
#4020=EDGE_LOOP('',(#14737,#14738,#14739,#14740));
#4021=EDGE_LOOP('',(#14741,#14742,#14743,#14744));
#4022=EDGE_LOOP('',(#14745,#14746,#14747,#14748));
#4023=EDGE_LOOP('',(#14749,#14750,#14751,#14752));
#4024=EDGE_LOOP('',(#14753,#14754,#14755,#14756));
#4025=EDGE_LOOP('',(#14757,#14758,#14759,#14760));
#4026=EDGE_LOOP('',(#14761,#14762,#14763,#14764));
#4027=EDGE_LOOP('',(#14765,#14766,#14767,#14768));
#4028=EDGE_LOOP('',(#14769,#14770,#14771,#14772));
#4029=EDGE_LOOP('',(#14773,#14774,#14775,#14776));
#4030=EDGE_LOOP('',(#14777,#14778,#14779,#14780));
#4031=EDGE_LOOP('',(#14781,#14782,#14783,#14784));
#4032=EDGE_LOOP('',(#14785,#14786,#14787,#14788));
#4033=EDGE_LOOP('',(#14789,#14790,#14791,#14792));
#4034=EDGE_LOOP('',(#14793,#14794,#14795,#14796));
#4035=EDGE_LOOP('',(#14797,#14798,#14799,#14800));
#4036=EDGE_LOOP('',(#14801,#14802,#14803,#14804));
#4037=EDGE_LOOP('',(#14805,#14806,#14807,#14808));
#4038=EDGE_LOOP('',(#14809,#14810,#14811,#14812));
#4039=EDGE_LOOP('',(#14813,#14814,#14815,#14816));
#4040=EDGE_LOOP('',(#14817,#14818,#14819,#14820));
#4041=EDGE_LOOP('',(#14821,#14822,#14823,#14824));
#4042=EDGE_LOOP('',(#14825,#14826,#14827,#14828));
#4043=EDGE_LOOP('',(#14829,#14830,#14831,#14832));
#4044=EDGE_LOOP('',(#14833,#14834,#14835,#14836));
#4045=EDGE_LOOP('',(#14837,#14838,#14839,#14840,#14841,#14842,#14843,#14844,
#14845,#14846,#14847,#14848,#14849,#14850,#14851,#14852,#14853,#14854,#14855,
#14856,#14857,#14858,#14859,#14860,#14861,#14862,#14863,#14864,#14865,#14866,
#14867,#14868,#14869,#14870,#14871,#14872,#14873,#14874,#14875,#14876,#14877,
#14878,#14879,#14880));
#4046=EDGE_LOOP('',(#14881));
#4047=EDGE_LOOP('',(#14882,#14883,#14884,#14885,#14886,#14887,#14888,#14889,
#14890,#14891,#14892,#14893,#14894,#14895,#14896,#14897,#14898,#14899,#14900,
#14901,#14902,#14903,#14904,#14905,#14906,#14907,#14908,#14909,#14910,#14911,
#14912,#14913,#14914,#14915,#14916,#14917,#14918,#14919,#14920,#14921,#14922,
#14923,#14924,#14925));
#4048=EDGE_LOOP('',(#14926));
#4049=EDGE_LOOP('',(#14927));
#4050=EDGE_LOOP('',(#14928,#14929,#14930,#14931));
#4051=EDGE_LOOP('',(#14932,#14933,#14934,#14935));
#4052=EDGE_LOOP('',(#14936,#14937,#14938,#14939));
#4053=EDGE_LOOP('',(#14940));
#4054=EDGE_LOOP('',(#14941));
#4055=EDGE_LOOP('',(#14942,#14943,#14944,#14945));
#4056=EDGE_LOOP('',(#14946,#14947,#14948,#14949));
#4057=EDGE_LOOP('',(#14950,#14951,#14952,#14953));
#4058=EDGE_LOOP('',(#14954));
#4059=EDGE_LOOP('',(#14955,#14956,#14957,#14958));
#4060=EDGE_LOOP('',(#14959,#14960,#14961,#14962));
#4061=EDGE_LOOP('',(#14963,#14964,#14965,#14966));
#4062=EDGE_LOOP('',(#14967,#14968,#14969,#14970));
#4063=EDGE_LOOP('',(#14971,#14972,#14973,#14974));
#4064=EDGE_LOOP('',(#14975,#14976,#14977,#14978));
#4065=EDGE_LOOP('',(#14979,#14980,#14981,#14982,#14983,#14984));
#4066=EDGE_LOOP('',(#14985,#14986,#14987,#14988,#14989,#14990));
#4067=EDGE_LOOP('',(#14991,#14992,#14993,#14994));
#4068=EDGE_LOOP('',(#14995,#14996,#14997,#14998));
#4069=EDGE_LOOP('',(#14999,#15000,#15001,#15002));
#4070=EDGE_LOOP('',(#15003));
#4071=EDGE_LOOP('',(#15004,#15005,#15006,#15007,#15008,#15009,#15010,#15011,
#15012,#15013));
#4072=EDGE_LOOP('',(#15014,#15015,#15016,#15017));
#4073=EDGE_LOOP('',(#15018,#15019,#15020,#15021));
#4074=EDGE_LOOP('',(#15022,#15023,#15024,#15025,#15026,#15027,#15028,#15029,
#15030,#15031));
#4075=EDGE_LOOP('',(#15032,#15033,#15034,#15035));
#4076=EDGE_LOOP('',(#15036,#15037,#15038,#15039,#15040,#15041));
#4077=EDGE_LOOP('',(#15042,#15043,#15044,#15045,#15046,#15047,#15048,#15049));
#4078=EDGE_LOOP('',(#15050,#15051,#15052,#15053,#15054));
#4079=EDGE_LOOP('',(#15055,#15056,#15057,#15058));
#4080=EDGE_LOOP('',(#15059,#15060,#15061,#15062,#15063,#15064));
#4081=EDGE_LOOP('',(#15065,#15066,#15067,#15068));
#4082=EDGE_LOOP('',(#15069));
#4083=EDGE_LOOP('',(#15070,#15071,#15072,#15073,#15074,#15075));
#4084=EDGE_LOOP('',(#15076));
#4085=EDGE_LOOP('',(#15077,#15078,#15079,#15080));
#4086=EDGE_LOOP('',(#15081,#15082,#15083,#15084));
#4087=EDGE_LOOP('',(#15085,#15086,#15087,#15088));
#4088=EDGE_LOOP('',(#15089));
#4089=EDGE_LOOP('',(#15090));
#4090=EDGE_LOOP('',(#15091,#15092,#15093,#15094));
#4091=EDGE_LOOP('',(#15095,#15096,#15097,#15098));
#4092=EDGE_LOOP('',(#15099,#15100,#15101,#15102));
#4093=EDGE_LOOP('',(#15103,#15104,#15105,#15106));
#4094=EDGE_LOOP('',(#15107,#15108,#15109,#15110));
#4095=EDGE_LOOP('',(#15111,#15112,#15113,#15114));
#4096=EDGE_LOOP('',(#15115,#15116,#15117,#15118));
#4097=EDGE_LOOP('',(#15119,#15120,#15121,#15122));
#4098=EDGE_LOOP('',(#15123,#15124,#15125,#15126,#15127,#15128));
#4099=EDGE_LOOP('',(#15129,#15130,#15131,#15132));
#4100=EDGE_LOOP('',(#15133,#15134,#15135,#15136));
#4101=EDGE_LOOP('',(#15137,#15138,#15139,#15140));
#4102=EDGE_LOOP('',(#15141,#15142,#15143,#15144));
#4103=EDGE_LOOP('',(#15145,#15146,#15147,#15148));
#4104=EDGE_LOOP('',(#15149,#15150,#15151,#15152));
#4105=EDGE_LOOP('',(#15153,#15154,#15155,#15156));
#4106=EDGE_LOOP('',(#15157,#15158,#15159,#15160));
#4107=EDGE_LOOP('',(#15161,#15162,#15163,#15164));
#4108=EDGE_LOOP('',(#15165,#15166,#15167,#15168));
#4109=EDGE_LOOP('',(#15169,#15170,#15171,#15172));
#4110=EDGE_LOOP('',(#15173,#15174,#15175,#15176));
#4111=EDGE_LOOP('',(#15177,#15178,#15179,#15180));
#4112=EDGE_LOOP('',(#15181,#15182,#15183,#15184));
#4113=EDGE_LOOP('',(#15185,#15186,#15187,#15188));
#4114=EDGE_LOOP('',(#15189,#15190,#15191,#15192));
#4115=EDGE_LOOP('',(#15193,#15194,#15195,#15196));
#4116=EDGE_LOOP('',(#15197,#15198,#15199,#15200));
#4117=EDGE_LOOP('',(#15201,#15202,#15203,#15204));
#4118=EDGE_LOOP('',(#15205,#15206,#15207,#15208));
#4119=EDGE_LOOP('',(#15209,#15210,#15211,#15212));
#4120=EDGE_LOOP('',(#15213,#15214,#15215,#15216));
#4121=EDGE_LOOP('',(#15217,#15218,#15219,#15220));
#4122=EDGE_LOOP('',(#15221));
#4123=EDGE_LOOP('',(#15222));
#4124=EDGE_LOOP('',(#15223));
#4125=EDGE_LOOP('',(#15224));
#4126=EDGE_LOOP('',(#15225));
#4127=EDGE_LOOP('',(#15226));
#4128=EDGE_LOOP('',(#15227));
#4129=EDGE_LOOP('',(#15228));
#4130=EDGE_LOOP('',(#15229));
#4131=EDGE_LOOP('',(#15230));
#4132=EDGE_LOOP('',(#15231));
#4133=EDGE_LOOP('',(#15232));
#4134=EDGE_LOOP('',(#15233));
#4135=EDGE_LOOP('',(#15234));
#4136=EDGE_LOOP('',(#15235));
#4137=EDGE_LOOP('',(#15236));
#4138=EDGE_LOOP('',(#15237));
#4139=EDGE_LOOP('',(#15238));
#4140=EDGE_LOOP('',(#15239,#15240,#15241,#15242));
#4141=EDGE_LOOP('',(#15243));
#4142=EDGE_LOOP('',(#15244));
#4143=EDGE_LOOP('',(#15245));
#4144=EDGE_LOOP('',(#15246));
#4145=EDGE_LOOP('',(#15247));
#4146=EDGE_LOOP('',(#15248));
#4147=EDGE_LOOP('',(#15249));
#4148=EDGE_LOOP('',(#15250));
#4149=EDGE_LOOP('',(#15251));
#4150=EDGE_LOOP('',(#15252));
#4151=EDGE_LOOP('',(#15253));
#4152=EDGE_LOOP('',(#15254));
#4153=EDGE_LOOP('',(#15255));
#4154=EDGE_LOOP('',(#15256));
#4155=EDGE_LOOP('',(#15257));
#4156=EDGE_LOOP('',(#15258));
#4157=EDGE_LOOP('',(#15259));
#4158=EDGE_LOOP('',(#15260));
#4159=EDGE_LOOP('',(#15261,#15262));
#4160=EDGE_LOOP('',(#15263,#15264,#15265,#15266,#15267,#15268,#15269,#15270));
#4161=EDGE_LOOP('',(#15271,#15272));
#4162=EDGE_LOOP('',(#15273,#15274,#15275,#15276,#15277,#15278,#15279,#15280));
#4163=EDGE_LOOP('',(#15281,#15282,#15283));
#4164=EDGE_LOOP('',(#15284,#15285,#15286,#15287,#15288,#15289,#15290,#15291));
#4165=EDGE_LOOP('',(#15292,#15293,#15294));
#4166=EDGE_LOOP('',(#15295,#15296,#15297,#15298,#15299,#15300,#15301,#15302));
#4167=EDGE_LOOP('',(#15303,#15304,#15305,#15306,#15307,#15308,#15309,#15310,
#15311,#15312,#15313,#15314,#15315,#15316,#15317,#15318,#15319,#15320,#15321,
#15322));
#4168=EDGE_LOOP('',(#15323,#15324,#15325,#15326));
#4169=EDGE_LOOP('',(#15327));
#4170=EDGE_LOOP('',(#15328));
#4171=EDGE_LOOP('',(#15329));
#4172=EDGE_LOOP('',(#15330,#15331,#15332,#15333,#15334,#15335,#15336,#15337,
#15338,#15339,#15340));
#4173=EDGE_LOOP('',(#15341,#15342,#15343,#15344));
#4174=EDGE_LOOP('',(#15345,#15346,#15347,#15348));
#4175=EDGE_LOOP('',(#15349));
#4176=EDGE_LOOP('',(#15350));
#4177=EDGE_LOOP('',(#15351));
#4178=EDGE_LOOP('',(#15352));
#4179=EDGE_LOOP('',(#15353));
#4180=EDGE_LOOP('',(#15354));
#4181=EDGE_LOOP('',(#15355));
#4182=EDGE_LOOP('',(#15356));
#4183=EDGE_LOOP('',(#15357,#15358));
#4184=EDGE_LOOP('',(#15359,#15360,#15361,#15362,#15363,#15364,#15365,#15366));
#4185=EDGE_LOOP('',(#15367,#15368));
#4186=EDGE_LOOP('',(#15369,#15370,#15371,#15372,#15373,#15374,#15375,#15376));
#4187=EDGE_LOOP('',(#15377,#15378,#15379));
#4188=EDGE_LOOP('',(#15380,#15381,#15382,#15383,#15384,#15385,#15386,#15387));
#4189=EDGE_LOOP('',(#15388,#15389,#15390));
#4190=EDGE_LOOP('',(#15391,#15392,#15393,#15394,#15395,#15396,#15397,#15398));
#4191=EDGE_LOOP('',(#15399,#15400,#15401,#15402,#15403,#15404,#15405,#15406,
#15407,#15408,#15409,#15410,#15411,#15412,#15413,#15414,#15415,#15416,#15417,
#15418));
#4192=EDGE_LOOP('',(#15419,#15420,#15421,#15422));
#4193=EDGE_LOOP('',(#15423));
#4194=EDGE_LOOP('',(#15424));
#4195=EDGE_LOOP('',(#15425));
#4196=EDGE_LOOP('',(#15426,#15427,#15428,#15429,#15430,#15431,#15432,#15433,
#15434,#15435,#15436));
#4197=EDGE_LOOP('',(#15437,#15438,#15439,#15440));
#4198=EDGE_LOOP('',(#15441,#15442,#15443,#15444));
#4199=EDGE_LOOP('',(#15445));
#4200=EDGE_LOOP('',(#15446));
#4201=EDGE_LOOP('',(#15447));
#4202=EDGE_LOOP('',(#15448));
#4203=EDGE_LOOP('',(#15449));
#4204=EDGE_LOOP('',(#15450));
#4205=EDGE_LOOP('',(#15451));
#4206=EDGE_LOOP('',(#15452));
#4207=EDGE_LOOP('',(#15453,#15454,#15455,#15456));
#4208=EDGE_LOOP('',(#15457));
#4209=EDGE_LOOP('',(#15458,#15459,#15460,#15461));
#4210=EDGE_LOOP('',(#15462));
#4211=EDGE_LOOP('',(#15463,#15464,#15465,#15466));
#4212=EDGE_LOOP('',(#15467));
#4213=EDGE_LOOP('',(#15468,#15469,#15470,#15471));
#4214=EDGE_LOOP('',(#15472,#15473,#15474,#15475));
#4215=EDGE_LOOP('',(#15476));
#4216=EDGE_LOOP('',(#15477));
#4217=EDGE_LOOP('',(#15478));
#4218=EDGE_LOOP('',(#15479));
#4219=EDGE_LOOP('',(#15480));
#4220=EDGE_LOOP('',(#15481));
#4221=EDGE_LOOP('',(#15482));
#4222=EDGE_LOOP('',(#15483,#15484,#15485,#15486));
#4223=EDGE_LOOP('',(#15487,#15488,#15489,#15490));
#4224=EDGE_LOOP('',(#15491,#15492,#15493,#15494));
#4225=EDGE_LOOP('',(#15495));
#4226=EDGE_LOOP('',(#15496));
#4227=EDGE_LOOP('',(#15497));
#4228=EDGE_LOOP('',(#15498));
#4229=EDGE_LOOP('',(#15499));
#4230=EDGE_LOOP('',(#15500));
#4231=EDGE_LOOP('',(#15501,#15502,#15503,#15504));
#4232=EDGE_LOOP('',(#15505,#15506,#15507,#15508));
#4233=EDGE_LOOP('',(#15509,#15510,#15511,#15512));
#4234=EDGE_LOOP('',(#15513,#15514,#15515,#15516));
#4235=EDGE_LOOP('',(#15517,#15518,#15519));
#4236=EDGE_LOOP('',(#15520,#15521,#15522,#15523));
#4237=EDGE_LOOP('',(#15524,#15525,#15526,#15527));
#4238=EDGE_LOOP('',(#15528));
#4239=EDGE_LOOP('',(#15529));
#4240=EDGE_LOOP('',(#15530,#15531,#15532,#15533));
#4241=EDGE_LOOP('',(#15534,#15535,#15536,#15537));
#4242=EDGE_LOOP('',(#15538,#15539,#15540,#15541,#15542,#15543,#15544,#15545));
#4243=EDGE_LOOP('',(#15546,#15547,#15548,#15549));
#4244=EDGE_LOOP('',(#15550,#15551,#15552,#15553));
#4245=EDGE_LOOP('',(#15554,#15555,#15556,#15557,#15558,#15559,#15560,#15561));
#4246=EDGE_LOOP('',(#15562,#15563,#15564,#15565,#15566,#15567,#15568,#15569));
#4247=EDGE_LOOP('',(#15570));
#4248=EDGE_LOOP('',(#15571));
#4249=EDGE_LOOP('',(#15572,#15573,#15574,#15575,#15576,#15577,#15578));
#4250=EDGE_LOOP('',(#15579,#15580,#15581,#15582));
#4251=EDGE_LOOP('',(#15583,#15584,#15585,#15586));
#4252=EDGE_LOOP('',(#15587,#15588,#15589,#15590));
#4253=EDGE_LOOP('',(#15591,#15592,#15593,#15594));
#4254=EDGE_LOOP('',(#15595,#15596,#15597,#15598));
#4255=EDGE_LOOP('',(#15599));
#4256=EDGE_LOOP('',(#15600));
#4257=EDGE_LOOP('',(#15601,#15602,#15603,#15604));
#4258=EDGE_LOOP('',(#15605));
#4259=EDGE_LOOP('',(#15606));
#4260=EDGE_LOOP('',(#15607,#15608,#15609,#15610));
#4261=EDGE_LOOP('',(#15611));
#4262=EDGE_LOOP('',(#15612));
#4263=EDGE_LOOP('',(#15613,#15614,#15615,#15616));
#4264=EDGE_LOOP('',(#15617));
#4265=EDGE_LOOP('',(#15618));
#4266=EDGE_LOOP('',(#15619,#15620,#15621,#15622));
#4267=EDGE_LOOP('',(#15623));
#4268=EDGE_LOOP('',(#15624));
#4269=EDGE_LOOP('',(#15625,#15626,#15627,#15628));
#4270=EDGE_LOOP('',(#15629));
#4271=EDGE_LOOP('',(#15630));
#4272=EDGE_LOOP('',(#15631,#15632,#15633,#15634));
#4273=EDGE_LOOP('',(#15635,#15636,#15637,#15638));
#4274=EDGE_LOOP('',(#15639,#15640,#15641,#15642));
#4275=EDGE_LOOP('',(#15643,#15644,#15645,#15646));
#4276=EDGE_LOOP('',(#15647,#15648,#15649,#15650));
#4277=EDGE_LOOP('',(#15651,#15652,#15653,#15654));
#4278=EDGE_LOOP('',(#15655));
#4279=EDGE_LOOP('',(#15656));
#4280=EDGE_LOOP('',(#15657,#15658,#15659,#15660));
#4281=EDGE_LOOP('',(#15661,#15662,#15663,#15664));
#4282=EDGE_LOOP('',(#15665));
#4283=EDGE_LOOP('',(#15666));
#4284=EDGE_LOOP('',(#15667,#15668,#15669,#15670));
#4285=EDGE_LOOP('',(#15671,#15672,#15673,#15674));
#4286=EDGE_LOOP('',(#15675,#15676,#15677,#15678));
#4287=EDGE_LOOP('',(#15679,#15680,#15681,#15682));
#4288=EDGE_LOOP('',(#15683,#15684,#15685,#15686));
#4289=EDGE_LOOP('',(#15687,#15688,#15689,#15690));
#4290=EDGE_LOOP('',(#15691,#15692,#15693,#15694));
#4291=EDGE_LOOP('',(#15695,#15696,#15697,#15698));
#4292=EDGE_LOOP('',(#15699,#15700,#15701,#15702));
#4293=EDGE_LOOP('',(#15703,#15704,#15705,#15706));
#4294=EDGE_LOOP('',(#15707,#15708,#15709));
#4295=EDGE_LOOP('',(#15710,#15711,#15712,#15713));
#4296=EDGE_LOOP('',(#15714,#15715,#15716,#15717));
#4297=EDGE_LOOP('',(#15718,#15719,#15720,#15721));
#4298=EDGE_LOOP('',(#15722,#15723,#15724,#15725));
#4299=EDGE_LOOP('',(#15726,#15727,#15728,#15729));
#4300=EDGE_LOOP('',(#15730,#15731,#15732,#15733));
#4301=EDGE_LOOP('',(#15734,#15735,#15736,#15737));
#4302=EDGE_LOOP('',(#15738,#15739,#15740,#15741));
#4303=EDGE_LOOP('',(#15742,#15743,#15744,#15745));
#4304=EDGE_LOOP('',(#15746,#15747,#15748,#15749));
#4305=EDGE_LOOP('',(#15750,#15751,#15752,#15753,#15754,#15755,#15756,#15757,
#15758,#15759,#15760,#15761,#15762,#15763,#15764,#15765,#15766,#15767,#15768,
#15769,#15770,#15771));
#4306=EDGE_LOOP('',(#15772,#15773,#15774,#15775,#15776,#15777,#15778,#15779,
#15780,#15781,#15782,#15783,#15784,#15785,#15786,#15787,#15788,#15789,#15790,
#15791,#15792));
#4307=EDGE_LOOP('',(#15793,#15794));
#4308=EDGE_LOOP('',(#15795,#15796,#15797,#15798,#15799));
#4309=EDGE_LOOP('',(#15800));
#4310=EDGE_LOOP('',(#15801));
#4311=EDGE_LOOP('',(#15802));
#4312=EDGE_LOOP('',(#15803,#15804,#15805,#15806));
#4313=EDGE_LOOP('',(#15807,#15808,#15809,#15810));
#4314=EDGE_LOOP('',(#15811,#15812,#15813,#15814));
#4315=EDGE_LOOP('',(#15815,#15816,#15817,#15818));
#4316=EDGE_LOOP('',(#15819,#15820));
#4317=EDGE_LOOP('',(#15821));
#4318=EDGE_LOOP('',(#15822));
#4319=EDGE_LOOP('',(#15823));
#4320=EDGE_LOOP('',(#15824));
#4321=EDGE_LOOP('',(#15825,#15826,#15827,#15828));
#4322=EDGE_LOOP('',(#15829,#15830,#15831,#15832,#15833));
#4323=EDGE_LOOP('',(#15834,#15835,#15836,#15837));
#4324=EDGE_LOOP('',(#15838));
#4325=EDGE_LOOP('',(#15839,#15840,#15841,#15842));
#4326=EDGE_LOOP('',(#15843,#15844,#15845,#15846));
#4327=EDGE_LOOP('',(#15847,#15848,#15849,#15850));
#4328=EDGE_LOOP('',(#15851,#15852,#15853,#15854));
#4329=EDGE_LOOP('',(#15855,#15856,#15857,#15858));
#4330=EDGE_LOOP('',(#15859,#15860,#15861,#15862));
#4331=EDGE_LOOP('',(#15863,#15864,#15865,#15866));
#4332=EDGE_LOOP('',(#15867,#15868,#15869,#15870,#15871,#15872));
#4333=EDGE_LOOP('',(#15873,#15874,#15875,#15876,#15877,#15878));
#4334=EDGE_LOOP('',(#15879));
#4335=EDGE_LOOP('',(#15880));
#4336=EDGE_LOOP('',(#15881,#15882,#15883,#15884));
#4337=EDGE_LOOP('',(#15885));
#4338=EDGE_LOOP('',(#15886));
#4339=EDGE_LOOP('',(#15887,#15888,#15889,#15890));
#4340=EDGE_LOOP('',(#15891,#15892,#15893,#15894));
#4341=EDGE_LOOP('',(#15895,#15896,#15897,#15898));
#4342=EDGE_LOOP('',(#15899));
#4343=EDGE_LOOP('',(#15900));
#4344=EDGE_LOOP('',(#15901,#15902,#15903,#15904));
#4345=EDGE_LOOP('',(#15905,#15906,#15907,#15908));
#4346=EDGE_LOOP('',(#15909));
#4347=EDGE_LOOP('',(#15910,#15911,#15912,#15913));
#4348=EDGE_LOOP('',(#15914,#15915,#15916,#15917));
#4349=EDGE_LOOP('',(#15918,#15919,#15920,#15921));
#4350=EDGE_LOOP('',(#15922));
#4351=EDGE_LOOP('',(#15923));
#4352=EDGE_LOOP('',(#15924,#15925,#15926,#15927));
#4353=EDGE_LOOP('',(#15928,#15929,#15930,#15931));
#4354=EDGE_LOOP('',(#15932,#15933,#15934,#15935));
#4355=EDGE_LOOP('',(#15936));
#4356=EDGE_LOOP('',(#15937,#15938,#15939,#15940));
#4357=EDGE_LOOP('',(#15941,#15942,#15943,#15944));
#4358=EDGE_LOOP('',(#15945,#15946,#15947,#15948));
#4359=EDGE_LOOP('',(#15949,#15950,#15951,#15952));
#4360=EDGE_LOOP('',(#15953,#15954,#15955,#15956));
#4361=EDGE_LOOP('',(#15957,#15958,#15959,#15960));
#4362=EDGE_LOOP('',(#15961,#15962,#15963,#15964,#15965,#15966));
#4363=EDGE_LOOP('',(#15967,#15968,#15969,#15970,#15971,#15972));
#4364=EDGE_LOOP('',(#15973,#15974,#15975,#15976));
#4365=EDGE_LOOP('',(#15977,#15978,#15979,#15980));
#4366=EDGE_LOOP('',(#15981,#15982,#15983,#15984));
#4367=EDGE_LOOP('',(#15985,#15986,#15987,#15988));
#4368=EDGE_LOOP('',(#15989,#15990,#15991,#15992));
#4369=EDGE_LOOP('',(#15993,#15994,#15995,#15996));
#4370=EDGE_LOOP('',(#15997,#15998,#15999,#16000));
#4371=EDGE_LOOP('',(#16001,#16002,#16003,#16004));
#4372=EDGE_LOOP('',(#16005,#16006,#16007,#16008));
#4373=EDGE_LOOP('',(#16009,#16010,#16011,#16012));
#4374=EDGE_LOOP('',(#16013,#16014,#16015,#16016));
#4375=EDGE_LOOP('',(#16017,#16018,#16019,#16020));
#4376=EDGE_LOOP('',(#16021,#16022,#16023,#16024));
#4377=EDGE_LOOP('',(#16025,#16026,#16027,#16028));
#4378=EDGE_LOOP('',(#16029,#16030,#16031,#16032));
#4379=EDGE_LOOP('',(#16033,#16034,#16035,#16036));
#4380=EDGE_LOOP('',(#16037,#16038,#16039,#16040));
#4381=EDGE_LOOP('',(#16041,#16042,#16043,#16044));
#4382=EDGE_LOOP('',(#16045,#16046,#16047,#16048));
#4383=EDGE_LOOP('',(#16049,#16050,#16051,#16052));
#4384=EDGE_LOOP('',(#16053,#16054,#16055,#16056));
#4385=EDGE_LOOP('',(#16057,#16058,#16059,#16060));
#4386=EDGE_LOOP('',(#16061,#16062,#16063,#16064));
#4387=EDGE_LOOP('',(#16065,#16066,#16067,#16068));
#4388=EDGE_LOOP('',(#16069,#16070,#16071,#16072));
#4389=EDGE_LOOP('',(#16073,#16074,#16075,#16076));
#4390=EDGE_LOOP('',(#16077,#16078,#16079,#16080));
#4391=EDGE_LOOP('',(#16081,#16082,#16083,#16084));
#4392=EDGE_LOOP('',(#16085,#16086,#16087,#16088));
#4393=EDGE_LOOP('',(#16089,#16090,#16091,#16092));
#4394=EDGE_LOOP('',(#16093,#16094,#16095,#16096));
#4395=EDGE_LOOP('',(#16097,#16098,#16099,#16100));
#4396=EDGE_LOOP('',(#16101,#16102,#16103,#16104));
#4397=EDGE_LOOP('',(#16105,#16106,#16107,#16108));
#4398=EDGE_LOOP('',(#16109,#16110,#16111,#16112));
#4399=EDGE_LOOP('',(#16113,#16114,#16115,#16116));
#4400=EDGE_LOOP('',(#16117,#16118,#16119,#16120));
#4401=EDGE_LOOP('',(#16121,#16122,#16123,#16124));
#4402=EDGE_LOOP('',(#16125,#16126,#16127,#16128));
#4403=EDGE_LOOP('',(#16129,#16130,#16131,#16132));
#4404=EDGE_LOOP('',(#16133,#16134,#16135,#16136));
#4405=EDGE_LOOP('',(#16137,#16138,#16139,#16140));
#4406=EDGE_LOOP('',(#16141,#16142,#16143,#16144));
#4407=EDGE_LOOP('',(#16145,#16146,#16147,#16148));
#4408=EDGE_LOOP('',(#16149,#16150,#16151,#16152));
#4409=EDGE_LOOP('',(#16153,#16154,#16155,#16156));
#4410=EDGE_LOOP('',(#16157,#16158,#16159,#16160));
#4411=EDGE_LOOP('',(#16161,#16162,#16163,#16164));
#4412=EDGE_LOOP('',(#16165,#16166,#16167,#16168));
#4413=EDGE_LOOP('',(#16169,#16170,#16171,#16172));
#4414=EDGE_LOOP('',(#16173,#16174,#16175,#16176));
#4415=EDGE_LOOP('',(#16177,#16178,#16179,#16180));
#4416=EDGE_LOOP('',(#16181,#16182,#16183,#16184));
#4417=EDGE_LOOP('',(#16185,#16186,#16187,#16188));
#4418=EDGE_LOOP('',(#16189,#16190,#16191,#16192));
#4419=EDGE_LOOP('',(#16193,#16194,#16195,#16196));
#4420=EDGE_LOOP('',(#16197,#16198,#16199,#16200));
#4421=EDGE_LOOP('',(#16201,#16202,#16203,#16204));
#4422=EDGE_LOOP('',(#16205,#16206,#16207,#16208));
#4423=EDGE_LOOP('',(#16209,#16210,#16211,#16212));
#4424=EDGE_LOOP('',(#16213,#16214,#16215,#16216));
#4425=EDGE_LOOP('',(#16217,#16218,#16219,#16220));
#4426=EDGE_LOOP('',(#16221,#16222,#16223,#16224));
#4427=EDGE_LOOP('',(#16225,#16226,#16227));
#4428=EDGE_LOOP('',(#16228,#16229,#16230,#16231,#16232));
#4429=EDGE_LOOP('',(#16233,#16234,#16235,#16236));
#4430=EDGE_LOOP('',(#16237,#16238,#16239,#16240));
#4431=EDGE_LOOP('',(#16241,#16242,#16243,#16244));
#4432=EDGE_LOOP('',(#16245,#16246,#16247,#16248));
#4433=EDGE_LOOP('',(#16249,#16250,#16251,#16252));
#4434=EDGE_LOOP('',(#16253,#16254,#16255,#16256));
#4435=EDGE_LOOP('',(#16257,#16258,#16259,#16260));
#4436=EDGE_LOOP('',(#16261,#16262,#16263,#16264));
#4437=EDGE_LOOP('',(#16265,#16266,#16267,#16268));
#4438=EDGE_LOOP('',(#16269,#16270,#16271,#16272));
#4439=EDGE_LOOP('',(#16273,#16274,#16275,#16276));
#4440=EDGE_LOOP('',(#16277,#16278,#16279,#16280));
#4441=EDGE_LOOP('',(#16281,#16282,#16283,#16284));
#4442=EDGE_LOOP('',(#16285,#16286,#16287,#16288));
#4443=EDGE_LOOP('',(#16289,#16290,#16291,#16292));
#4444=EDGE_LOOP('',(#16293,#16294,#16295,#16296));
#4445=EDGE_LOOP('',(#16297,#16298,#16299,#16300));
#4446=EDGE_LOOP('',(#16301,#16302,#16303,#16304));
#4447=EDGE_LOOP('',(#16305,#16306,#16307,#16308));
#4448=EDGE_LOOP('',(#16309,#16310,#16311,#16312));
#4449=EDGE_LOOP('',(#16313,#16314,#16315,#16316));
#4450=EDGE_LOOP('',(#16317,#16318,#16319,#16320));
#4451=EDGE_LOOP('',(#16321,#16322,#16323,#16324));
#4452=EDGE_LOOP('',(#16325,#16326,#16327,#16328));
#4453=EDGE_LOOP('',(#16329,#16330,#16331,#16332));
#4454=EDGE_LOOP('',(#16333,#16334,#16335,#16336));
#4455=EDGE_LOOP('',(#16337,#16338,#16339,#16340));
#4456=EDGE_LOOP('',(#16341,#16342,#16343,#16344));
#4457=EDGE_LOOP('',(#16345,#16346,#16347,#16348));
#4458=EDGE_LOOP('',(#16349,#16350,#16351,#16352));
#4459=EDGE_LOOP('',(#16353,#16354,#16355,#16356));
#4460=EDGE_LOOP('',(#16357,#16358,#16359,#16360));
#4461=EDGE_LOOP('',(#16361,#16362,#16363,#16364));
#4462=EDGE_LOOP('',(#16365,#16366,#16367,#16368));
#4463=EDGE_LOOP('',(#16369,#16370,#16371,#16372));
#4464=EDGE_LOOP('',(#16373,#16374,#16375,#16376));
#4465=EDGE_LOOP('',(#16377,#16378,#16379,#16380));
#4466=EDGE_LOOP('',(#16381,#16382,#16383,#16384));
#4467=EDGE_LOOP('',(#16385,#16386,#16387,#16388));
#4468=EDGE_LOOP('',(#16389,#16390,#16391,#16392));
#4469=EDGE_LOOP('',(#16393,#16394,#16395,#16396));
#4470=EDGE_LOOP('',(#16397,#16398,#16399,#16400));
#4471=EDGE_LOOP('',(#16401,#16402,#16403,#16404));
#4472=EDGE_LOOP('',(#16405,#16406,#16407,#16408));
#4473=EDGE_LOOP('',(#16409,#16410,#16411,#16412));
#4474=EDGE_LOOP('',(#16413,#16414,#16415,#16416));
#4475=EDGE_LOOP('',(#16417,#16418,#16419,#16420));
#4476=EDGE_LOOP('',(#16421,#16422,#16423,#16424));
#4477=EDGE_LOOP('',(#16425,#16426,#16427,#16428));
#4478=EDGE_LOOP('',(#16429,#16430,#16431,#16432));
#4479=EDGE_LOOP('',(#16433,#16434,#16435,#16436));
#4480=EDGE_LOOP('',(#16437,#16438,#16439,#16440));
#4481=EDGE_LOOP('',(#16441,#16442,#16443,#16444));
#4482=EDGE_LOOP('',(#16445,#16446,#16447,#16448));
#4483=EDGE_LOOP('',(#16449,#16450,#16451,#16452));
#4484=EDGE_LOOP('',(#16453,#16454,#16455,#16456));
#4485=EDGE_LOOP('',(#16457,#16458,#16459,#16460));
#4486=EDGE_LOOP('',(#16461,#16462,#16463,#16464));
#4487=EDGE_LOOP('',(#16465,#16466,#16467,#16468));
#4488=EDGE_LOOP('',(#16469,#16470,#16471,#16472));
#4489=EDGE_LOOP('',(#16473,#16474,#16475,#16476));
#4490=EDGE_LOOP('',(#16477));
#4491=EDGE_LOOP('',(#16478,#16479,#16480,#16481));
#4492=EDGE_LOOP('',(#16482,#16483,#16484,#16485));
#4493=EDGE_LOOP('',(#16486));
#4494=EDGE_LOOP('',(#16487,#16488,#16489,#16490,#16491,#16492,#16493,#16494,
#16495,#16496,#16497,#16498,#16499,#16500,#16501,#16502,#16503,#16504,#16505,
#16506,#16507,#16508,#16509,#16510,#16511,#16512,#16513,#16514,#16515,#16516,
#16517,#16518,#16519,#16520,#16521,#16522,#16523,#16524,#16525,#16526,#16527,
#16528,#16529,#16530,#16531,#16532,#16533,#16534,#16535,#16536,#16537,#16538,
#16539,#16540,#16541,#16542,#16543,#16544,#16545,#16546,#16547,#16548,#16549,
#16550,#16551,#16552,#16553,#16554,#16555,#16556,#16557,#16558,#16559,#16560,
#16561,#16562,#16563,#16564,#16565,#16566,#16567,#16568,#16569,#16570,#16571,
#16572,#16573,#16574,#16575,#16576,#16577,#16578,#16579,#16580,#16581,#16582,
#16583,#16584,#16585,#16586,#16587,#16588,#16589,#16590,#16591,#16592,#16593,
#16594,#16595,#16596,#16597,#16598,#16599,#16600,#16601,#16602,#16603,#16604,
#16605,#16606,#16607,#16608,#16609,#16610,#16611,#16612,#16613,#16614,#16615));
#4495=EDGE_LOOP('',(#16616,#16617,#16618,#16619));
#4496=EDGE_LOOP('',(#16620,#16621,#16622,#16623,#16624,#16625,#16626,#16627,
#16628,#16629,#16630,#16631,#16632,#16633,#16634,#16635,#16636,#16637,#16638,
#16639,#16640,#16641,#16642,#16643,#16644,#16645,#16646,#16647,#16648,#16649,
#16650,#16651,#16652,#16653,#16654,#16655,#16656,#16657,#16658,#16659,#16660,
#16661,#16662,#16663,#16664,#16665,#16666,#16667,#16668,#16669,#16670,#16671,
#16672,#16673,#16674,#16675,#16676,#16677,#16678,#16679,#16680,#16681,#16682,
#16683,#16684,#16685,#16686,#16687,#16688,#16689,#16690,#16691,#16692,#16693,
#16694,#16695,#16696,#16697,#16698,#16699,#16700,#16701,#16702,#16703,#16704,
#16705,#16706,#16707,#16708,#16709,#16710,#16711,#16712,#16713,#16714,#16715,
#16716,#16717,#16718,#16719,#16720,#16721,#16722,#16723,#16724,#16725,#16726,
#16727,#16728,#16729,#16730,#16731,#16732,#16733,#16734,#16735,#16736,#16737,
#16738,#16739,#16740,#16741,#16742,#16743,#16744,#16745,#16746,#16747,#16748,
#16749));
#4497=EDGE_LOOP('',(#16750,#16751,#16752,#16753));
#4498=EDGE_LOOP('',(#16754,#16755,#16756,#16757));
#4499=EDGE_LOOP('',(#16758,#16759,#16760,#16761));
#4500=EDGE_LOOP('',(#16762,#16763,#16764,#16765));
#4501=EDGE_LOOP('',(#16766,#16767,#16768,#16769));
#4502=EDGE_LOOP('',(#16770,#16771,#16772,#16773));
#4503=EDGE_LOOP('',(#16774,#16775,#16776,#16777));
#4504=EDGE_LOOP('',(#16778));
#4505=EDGE_LOOP('',(#16779));
#4506=EDGE_LOOP('',(#16780,#16781,#16782,#16783,#16784));
#4507=EDGE_LOOP('',(#16785,#16786,#16787,#16788));
#4508=EDGE_LOOP('',(#16789));
#4509=EDGE_LOOP('',(#16790));
#4510=EDGE_LOOP('',(#16791,#16792,#16793,#16794));
#4511=EDGE_LOOP('',(#16795,#16796,#16797,#16798));
#4512=EDGE_LOOP('',(#16799,#16800,#16801,#16802));
#4513=EDGE_LOOP('',(#16803));
#4514=EDGE_LOOP('',(#16804));
#4515=EDGE_LOOP('',(#16805));
#4516=EDGE_LOOP('',(#16806));
#4517=EDGE_LOOP('',(#16807,#16808));
#4518=EDGE_LOOP('',(#16809,#16810,#16811,#16812,#16813,#16814,#16815,#16816,
#16817));
#4519=EDGE_LOOP('',(#16818,#16819));
#4520=EDGE_LOOP('',(#16820,#16821,#16822,#16823));
#4521=EDGE_LOOP('',(#16824,#16825,#16826,#16827,#16828));
#4522=EDGE_LOOP('',(#16829,#16830,#16831,#16832));
#4523=EDGE_LOOP('',(#16833,#16834));
#4524=EDGE_LOOP('',(#16835));
#4525=EDGE_LOOP('',(#16836));
#4526=EDGE_LOOP('',(#16837));
#4527=EDGE_LOOP('',(#16838));
#4528=EDGE_LOOP('',(#16839,#16840,#16841,#16842));
#4529=EDGE_LOOP('',(#16843,#16844));
#4530=EDGE_LOOP('',(#16845,#16846,#16847,#16848,#16849,#16850,#16851,#16852,
#16853));
#4531=EDGE_LOOP('',(#16854,#16855));
#4532=EDGE_LOOP('',(#16856,#16857,#16858,#16859,#16860,#16861));
#4533=EDGE_LOOP('',(#16862,#16863,#16864,#16865));
#4534=EDGE_LOOP('',(#16866,#16867,#16868,#16869,#16870,#16871));
#4535=EDGE_LOOP('',(#16872));
#4536=EDGE_LOOP('',(#16873));
#4537=EDGE_LOOP('',(#16874,#16875,#16876,#16877));
#4538=EDGE_LOOP('',(#16878));
#4539=EDGE_LOOP('',(#16879));
#4540=EDGE_LOOP('',(#16880,#16881,#16882,#16883));
#4541=EDGE_LOOP('',(#16884,#16885,#16886,#16887));
#4542=EDGE_LOOP('',(#16888,#16889,#16890,#16891));
#4543=EDGE_LOOP('',(#16892,#16893,#16894,#16895,#16896));
#4544=EDGE_LOOP('',(#16897,#16898,#16899,#16900));
#4545=EDGE_LOOP('',(#16901,#16902));
#4546=EDGE_LOOP('',(#16903,#16904,#16905,#16906));
#4547=EDGE_LOOP('',(#16907,#16908,#16909,#16910));
#4548=EDGE_LOOP('',(#16911,#16912,#16913,#16914));
#4549=EDGE_LOOP('',(#16915));
#4550=EDGE_LOOP('',(#16916));
#4551=EDGE_LOOP('',(#16917));
#4552=EDGE_LOOP('',(#16918));
#4553=EDGE_LOOP('',(#16919,#16920,#16921,#16922));
#4554=EDGE_LOOP('',(#16923,#16924,#16925,#16926));
#4555=EDGE_LOOP('',(#16927));
#4556=EDGE_LOOP('',(#16928));
#4557=EDGE_LOOP('',(#16929));
#4558=EDGE_LOOP('',(#16930));
#4559=EDGE_LOOP('',(#16931,#16932,#16933,#16934,#16935,#16936,#16937,#16938));
#4560=EDGE_LOOP('',(#16939,#16940,#16941,#16942));
#4561=EDGE_LOOP('',(#16943,#16944,#16945,#16946));
#4562=EDGE_LOOP('',(#16947,#16948,#16949,#16950));
#4563=EDGE_LOOP('',(#16951,#16952,#16953,#16954));
#4564=EDGE_LOOP('',(#16955,#16956,#16957,#16958,#16959,#16960,#16961,#16962));
#4565=EDGE_LOOP('',(#16963,#16964,#16965,#16966));
#4566=EDGE_LOOP('',(#16967,#16968,#16969,#16970));
#4567=EDGE_LOOP('',(#16971,#16972,#16973,#16974));
#4568=EDGE_LOOP('',(#16975,#16976,#16977,#16978));
#4569=EDGE_LOOP('',(#16979,#16980,#16981,#16982));
#4570=EDGE_LOOP('',(#16983,#16984,#16985,#16986));
#4571=EDGE_LOOP('',(#16987,#16988,#16989,#16990));
#4572=EDGE_LOOP('',(#16991,#16992,#16993,#16994));
#4573=EDGE_LOOP('',(#16995,#16996,#16997,#16998));
#4574=EDGE_LOOP('',(#16999,#17000,#17001,#17002));
#4575=EDGE_LOOP('',(#17003,#17004,#17005,#17006,#17007,#17008));
#4576=EDGE_LOOP('',(#17009));
#4577=EDGE_LOOP('',(#17010,#17011,#17012,#17013,#17014,#17015));
#4578=EDGE_LOOP('',(#17016,#17017,#17018,#17019));
#4579=EDGE_LOOP('',(#17020,#17021,#17022,#17023));
#4580=EDGE_LOOP('',(#17024,#17025,#17026,#17027));
#4581=EDGE_LOOP('',(#17028));
#4582=EDGE_LOOP('',(#17029,#17030,#17031,#17032));
#4583=EDGE_LOOP('',(#17033,#17034,#17035,#17036));
#4584=EDGE_LOOP('',(#17037));
#4585=EDGE_LOOP('',(#17038));
#4586=EDGE_LOOP('',(#17039));
#4587=EDGE_LOOP('',(#17040));
#4588=EDGE_LOOP('',(#17041));
#4589=EDGE_LOOP('',(#17042,#17043,#17044,#17045));
#4590=EDGE_LOOP('',(#17046,#17047,#17048,#17049));
#4591=EDGE_LOOP('',(#17050,#17051,#17052,#17053));
#4592=EDGE_LOOP('',(#17054));
#4593=EDGE_LOOP('',(#17055));
#4594=EDGE_LOOP('',(#17056,#17057,#17058,#17059));
#4595=EDGE_LOOP('',(#17060,#17061,#17062,#17063));
#4596=EDGE_LOOP('',(#17064,#17065,#17066,#17067));
#4597=EDGE_LOOP('',(#17068));
#4598=EDGE_LOOP('',(#17069,#17070,#17071,#17072));
#4599=EDGE_LOOP('',(#17073,#17074,#17075,#17076));
#4600=EDGE_LOOP('',(#17077,#17078,#17079,#17080));
#4601=EDGE_LOOP('',(#17081,#17082,#17083,#17084));
#4602=EDGE_LOOP('',(#17085,#17086,#17087,#17088));
#4603=EDGE_LOOP('',(#17089,#17090,#17091,#17092));
#4604=EDGE_LOOP('',(#17093,#17094,#17095,#17096,#17097,#17098));
#4605=EDGE_LOOP('',(#17099,#17100,#17101,#17102,#17103,#17104));
#4606=LINE('',#26459,#6038);
#4607=LINE('',#26464,#6039);
#4608=LINE('',#26466,#6040);
#4609=LINE('',#26468,#6041);
#4610=LINE('',#26469,#6042);
#4611=LINE('',#26473,#6043);
#4612=LINE('',#26474,#6044);
#4613=LINE('',#26475,#6045);
#4614=LINE('',#26479,#6046);
#4615=LINE('',#26480,#6047);
#4616=LINE('',#26481,#6048);
#4617=LINE('',#26484,#6049);
#4618=LINE('',#26486,#6050);
#4619=LINE('',#26487,#6051);
#4620=LINE('',#26490,#6052);
#4621=LINE('',#26492,#6053);
#4622=LINE('',#26493,#6054);
#4623=LINE('',#26498,#6055);
#4624=LINE('',#26505,#6056);
#4625=LINE('',#26512,#6057);
#4626=LINE('',#26519,#6058);
#4627=LINE('',#26526,#6059);
#4628=LINE('',#26532,#6060);
#4629=LINE('',#26538,#6061);
#4630=LINE('',#26544,#6062);
#4631=LINE('',#26550,#6063);
#4632=LINE('',#26556,#6064);
#4633=LINE('',#26562,#6065);
#4634=LINE('',#26568,#6066);
#4635=LINE('',#26574,#6067);
#4636=LINE('',#26580,#6068);
#4637=LINE('',#26586,#6069);
#4638=LINE('',#26592,#6070);
#4639=LINE('',#26598,#6071);
#4640=LINE('',#26604,#6072);
#4641=LINE('',#26610,#6073);
#4642=LINE('',#26614,#6074);
#4643=LINE('',#26616,#6075);
#4644=LINE('',#26617,#6076);
#4645=LINE('',#26620,#6077);
#4646=LINE('',#26622,#6078);
#4647=LINE('',#26623,#6079);
#4648=LINE('',#26625,#6080);
#4649=LINE('',#26626,#6081);
#4650=LINE('',#26633,#6082);
#4651=LINE('',#26635,#6083);
#4652=LINE('',#26637,#6084);
#4653=LINE('',#26638,#6085);
#4654=LINE('',#26641,#6086);
#4655=LINE('',#26643,#6087);
#4656=LINE('',#26644,#6088);
#4657=LINE('',#26647,#6089);
#4658=LINE('',#26649,#6090);
#4659=LINE('',#26650,#6091);
#4660=LINE('',#26652,#6092);
#4661=LINE('',#26653,#6093);
#4662=LINE('',#26660,#6094);
#4663=LINE('',#26662,#6095);
#4664=LINE('',#26664,#6096);
#4665=LINE('',#26665,#6097);
#4666=LINE('',#26668,#6098);
#4667=LINE('',#26670,#6099);
#4668=LINE('',#26671,#6100);
#4669=LINE('',#26674,#6101);
#4670=LINE('',#26676,#6102);
#4671=LINE('',#26677,#6103);
#4672=LINE('',#26679,#6104);
#4673=LINE('',#26680,#6105);
#4674=LINE('',#26688,#6106);
#4675=LINE('',#26694,#6107);
#4676=LINE('',#26700,#6108);
#4677=LINE('',#26706,#6109);
#4678=LINE('',#26712,#6110);
#4679=LINE('',#26718,#6111);
#4680=LINE('',#26724,#6112);
#4681=LINE('',#26730,#6113);
#4682=LINE('',#26735,#6114);
#4683=LINE('',#26737,#6115);
#4684=LINE('',#26739,#6116);
#4685=LINE('',#26740,#6117);
#4686=LINE('',#26743,#6118);
#4687=LINE('',#26745,#6119);
#4688=LINE('',#26746,#6120);
#4689=LINE('',#26749,#6121);
#4690=LINE('',#26751,#6122);
#4691=LINE('',#26752,#6123);
#4692=LINE('',#26754,#6124);
#4693=LINE('',#26755,#6125);
#4694=LINE('',#26760,#6126);
#4695=LINE('',#26766,#6127);
#4696=LINE('',#26771,#6128);
#4697=LINE('',#26773,#6129);
#4698=LINE('',#26775,#6130);
#4699=LINE('',#26776,#6131);
#4700=LINE('',#26779,#6132);
#4701=LINE('',#26781,#6133);
#4702=LINE('',#26782,#6134);
#4703=LINE('',#26785,#6135);
#4704=LINE('',#26787,#6136);
#4705=LINE('',#26788,#6137);
#4706=LINE('',#26790,#6138);
#4707=LINE('',#26791,#6139);
#4708=LINE('',#26799,#6140);
#4709=LINE('',#26805,#6141);
#4710=LINE('',#26811,#6142);
#4711=LINE('',#26818,#6143);
#4712=LINE('',#26825,#6144);
#4713=LINE('',#26832,#6145);
#4714=LINE('',#26838,#6146);
#4715=LINE('',#26840,#6147);
#4716=LINE('',#26842,#6148);
#4717=LINE('',#26843,#6149);
#4718=LINE('',#26846,#6150);
#4719=LINE('',#26848,#6151);
#4720=LINE('',#26849,#6152);
#4721=LINE('',#26852,#6153);
#4722=LINE('',#26854,#6154);
#4723=LINE('',#26855,#6155);
#4724=LINE('',#26857,#6156);
#4725=LINE('',#26858,#6157);
#4726=LINE('',#26866,#6158);
#4727=LINE('',#26872,#6159);
#4728=LINE('',#26878,#6160);
#4729=LINE('',#26885,#6161);
#4730=LINE('',#26892,#6162);
#4731=LINE('',#26899,#6163);
#4732=LINE('',#26905,#6164);
#4733=LINE('',#26907,#6165);
#4734=LINE('',#26909,#6166);
#4735=LINE('',#26910,#6167);
#4736=LINE('',#26913,#6168);
#4737=LINE('',#26915,#6169);
#4738=LINE('',#26916,#6170);
#4739=LINE('',#26919,#6171);
#4740=LINE('',#26921,#6172);
#4741=LINE('',#26922,#6173);
#4742=LINE('',#26924,#6174);
#4743=LINE('',#26925,#6175);
#4744=LINE('',#26933,#6176);
#4745=LINE('',#26940,#6177);
#4746=LINE('',#26947,#6178);
#4747=LINE('',#26953,#6179);
#4748=LINE('',#26958,#6180);
#4749=LINE('',#26960,#6181);
#4750=LINE('',#26962,#6182);
#4751=LINE('',#26963,#6183);
#4752=LINE('',#26966,#6184);
#4753=LINE('',#26968,#6185);
#4754=LINE('',#26969,#6186);
#4755=LINE('',#26972,#6187);
#4756=LINE('',#26974,#6188);
#4757=LINE('',#26975,#6189);
#4758=LINE('',#26977,#6190);
#4759=LINE('',#26978,#6191);
#4760=LINE('',#26986,#6192);
#4761=LINE('',#26992,#6193);
#4762=LINE('',#26998,#6194);
#4763=LINE('',#27002,#6195);
#4764=LINE('',#27006,#6196);
#4765=LINE('',#27009,#6197);
#4766=LINE('',#27014,#6198);
#4767=LINE('',#27018,#6199);
#4768=LINE('',#27022,#6200);
#4769=LINE('',#27025,#6201);
#4770=LINE('',#27027,#6202);
#4771=LINE('',#27029,#6203);
#4772=LINE('',#27031,#6204);
#4773=LINE('',#27033,#6205);
#4774=LINE('',#27035,#6206);
#4775=LINE('',#27036,#6207);
#4776=LINE('',#27039,#6208);
#4777=LINE('',#27041,#6209);
#4778=LINE('',#27042,#6210);
#4779=LINE('',#27046,#6211);
#4780=LINE('',#27047,#6212);
#4781=LINE('',#27048,#6213);
#4782=LINE('',#27052,#6214);
#4783=LINE('',#27053,#6215);
#4784=LINE('',#27054,#6216);
#4785=LINE('',#27058,#6217);
#4786=LINE('',#27059,#6218);
#4787=LINE('',#27060,#6219);
#4788=LINE('',#27062,#6220);
#4789=LINE('',#27063,#6221);
#4790=LINE('',#27071,#6222);
#4791=LINE('',#27078,#6223);
#4792=LINE('',#27085,#6224);
#4793=LINE('',#27091,#6225);
#4794=LINE('',#27096,#6226);
#4795=LINE('',#27098,#6227);
#4796=LINE('',#27100,#6228);
#4797=LINE('',#27101,#6229);
#4798=LINE('',#27104,#6230);
#4799=LINE('',#27106,#6231);
#4800=LINE('',#27107,#6232);
#4801=LINE('',#27110,#6233);
#4802=LINE('',#27112,#6234);
#4803=LINE('',#27113,#6235);
#4804=LINE('',#27115,#6236);
#4805=LINE('',#27116,#6237);
#4806=LINE('',#27124,#6238);
#4807=LINE('',#27130,#6239);
#4808=LINE('',#27136,#6240);
#4809=LINE('',#27140,#6241);
#4810=LINE('',#27144,#6242);
#4811=LINE('',#27147,#6243);
#4812=LINE('',#27152,#6244);
#4813=LINE('',#27156,#6245);
#4814=LINE('',#27160,#6246);
#4815=LINE('',#27163,#6247);
#4816=LINE('',#27165,#6248);
#4817=LINE('',#27167,#6249);
#4818=LINE('',#27169,#6250);
#4819=LINE('',#27171,#6251);
#4820=LINE('',#27173,#6252);
#4821=LINE('',#27174,#6253);
#4822=LINE('',#27177,#6254);
#4823=LINE('',#27179,#6255);
#4824=LINE('',#27180,#6256);
#4825=LINE('',#27184,#6257);
#4826=LINE('',#27185,#6258);
#4827=LINE('',#27186,#6259);
#4828=LINE('',#27190,#6260);
#4829=LINE('',#27191,#6261);
#4830=LINE('',#27192,#6262);
#4831=LINE('',#27196,#6263);
#4832=LINE('',#27197,#6264);
#4833=LINE('',#27198,#6265);
#4834=LINE('',#27200,#6266);
#4835=LINE('',#27201,#6267);
#4836=LINE('',#27209,#6268);
#4837=LINE('',#27215,#6269);
#4838=LINE('',#27221,#6270);
#4839=LINE('',#27227,#6271);
#4840=LINE('',#27234,#6272);
#4841=LINE('',#27241,#6273);
#4842=LINE('',#27248,#6274);
#4843=LINE('',#27255,#6275);
#4844=LINE('',#27262,#6276);
#4845=LINE('',#27268,#6277);
#4846=LINE('',#27274,#6278);
#4847=LINE('',#27276,#6279);
#4848=LINE('',#27278,#6280);
#4849=LINE('',#27279,#6281);
#4850=LINE('',#27282,#6282);
#4851=LINE('',#27284,#6283);
#4852=LINE('',#27285,#6284);
#4853=LINE('',#27288,#6285);
#4854=LINE('',#27290,#6286);
#4855=LINE('',#27291,#6287);
#4856=LINE('',#27293,#6288);
#4857=LINE('',#27294,#6289);
#4858=LINE('',#27302,#6290);
#4859=LINE('',#27308,#6291);
#4860=LINE('',#27314,#6292);
#4861=LINE('',#27320,#6293);
#4862=LINE('',#27326,#6294);
#4863=LINE('',#27332,#6295);
#4864=LINE('',#27339,#6296);
#4865=LINE('',#27346,#6297);
#4866=LINE('',#27353,#6298);
#4867=LINE('',#27360,#6299);
#4868=LINE('',#27368,#6300);
#4869=LINE('',#27372,#6301);
#4870=LINE('',#27376,#6302);
#4871=LINE('',#27381,#6303);
#4872=LINE('',#27385,#6304);
#4873=LINE('',#27389,#6305);
#4874=LINE('',#27391,#6306);
#4875=LINE('',#27392,#6307);
#4876=LINE('',#27395,#6308);
#4877=LINE('',#27396,#6309);
#4878=LINE('',#27397,#6310);
#4879=LINE('',#27399,#6311);
#4880=LINE('',#27402,#6312);
#4881=LINE('',#27403,#6313);
#4882=LINE('',#27405,#6314);
#4883=LINE('',#27412,#6315);
#4884=LINE('',#27418,#6316);
#4885=LINE('',#27424,#6317);
#4886=LINE('',#27430,#6318);
#4887=LINE('',#27437,#6319);
#4888=LINE('',#27443,#6320);
#4889=LINE('',#27452,#6321);
#4890=LINE('',#27458,#6322);
#4891=LINE('',#27464,#6323);
#4892=LINE('',#27470,#6324);
#4893=LINE('',#27478,#6325);
#4894=LINE('',#27483,#6326);
#4895=LINE('',#27492,#6327);
#4896=LINE('',#27499,#6328);
#4897=LINE('',#27508,#6329);
#4898=LINE('',#27515,#6330);
#4899=LINE('',#27524,#6331);
#4900=LINE('',#27531,#6332);
#4901=LINE('',#27540,#6333);
#4902=LINE('',#27547,#6334);
#4903=LINE('',#27556,#6335);
#4904=LINE('',#27565,#6336);
#4905=LINE('',#27574,#6337);
#4906=LINE('',#27583,#6338);
#4907=LINE('',#27591,#6339);
#4908=LINE('',#27595,#6340);
#4909=LINE('',#27599,#6341);
#4910=LINE('',#27603,#6342);
#4911=LINE('',#27608,#6343);
#4912=LINE('',#27616,#6344);
#4913=LINE('',#27618,#6345);
#4914=LINE('',#27620,#6346);
#4915=LINE('',#27621,#6347);
#4916=LINE('',#27624,#6348);
#4917=LINE('',#27626,#6349);
#4918=LINE('',#27627,#6350);
#4919=LINE('',#27630,#6351);
#4920=LINE('',#27632,#6352);
#4921=LINE('',#27633,#6353);
#4922=LINE('',#27635,#6354);
#4923=LINE('',#27636,#6355);
#4924=LINE('',#27641,#6356);
#4925=LINE('',#27643,#6357);
#4926=LINE('',#27645,#6358);
#4927=LINE('',#27646,#6359);
#4928=LINE('',#27649,#6360);
#4929=LINE('',#27651,#6361);
#4930=LINE('',#27652,#6362);
#4931=LINE('',#27655,#6363);
#4932=LINE('',#27657,#6364);
#4933=LINE('',#27658,#6365);
#4934=LINE('',#27660,#6366);
#4935=LINE('',#27661,#6367);
#4936=LINE('',#27666,#6368);
#4937=LINE('',#27668,#6369);
#4938=LINE('',#27670,#6370);
#4939=LINE('',#27671,#6371);
#4940=LINE('',#27674,#6372);
#4941=LINE('',#27676,#6373);
#4942=LINE('',#27677,#6374);
#4943=LINE('',#27680,#6375);
#4944=LINE('',#27682,#6376);
#4945=LINE('',#27683,#6377);
#4946=LINE('',#27685,#6378);
#4947=LINE('',#27686,#6379);
#4948=LINE('',#27691,#6380);
#4949=LINE('',#27693,#6381);
#4950=LINE('',#27695,#6382);
#4951=LINE('',#27696,#6383);
#4952=LINE('',#27699,#6384);
#4953=LINE('',#27701,#6385);
#4954=LINE('',#27702,#6386);
#4955=LINE('',#27705,#6387);
#4956=LINE('',#27707,#6388);
#4957=LINE('',#27708,#6389);
#4958=LINE('',#27710,#6390);
#4959=LINE('',#27711,#6391);
#4960=LINE('',#27716,#6392);
#4961=LINE('',#27718,#6393);
#4962=LINE('',#27720,#6394);
#4963=LINE('',#27721,#6395);
#4964=LINE('',#27724,#6396);
#4965=LINE('',#27726,#6397);
#4966=LINE('',#27727,#6398);
#4967=LINE('',#27730,#6399);
#4968=LINE('',#27732,#6400);
#4969=LINE('',#27733,#6401);
#4970=LINE('',#27735,#6402);
#4971=LINE('',#27736,#6403);
#4972=LINE('',#27741,#6404);
#4973=LINE('',#27743,#6405);
#4974=LINE('',#27745,#6406);
#4975=LINE('',#27746,#6407);
#4976=LINE('',#27749,#6408);
#4977=LINE('',#27751,#6409);
#4978=LINE('',#27752,#6410);
#4979=LINE('',#27755,#6411);
#4980=LINE('',#27757,#6412);
#4981=LINE('',#27758,#6413);
#4982=LINE('',#27760,#6414);
#4983=LINE('',#27761,#6415);
#4984=LINE('',#27766,#6416);
#4985=LINE('',#27768,#6417);
#4986=LINE('',#27770,#6418);
#4987=LINE('',#27771,#6419);
#4988=LINE('',#27774,#6420);
#4989=LINE('',#27776,#6421);
#4990=LINE('',#27777,#6422);
#4991=LINE('',#27780,#6423);
#4992=LINE('',#27782,#6424);
#4993=LINE('',#27783,#6425);
#4994=LINE('',#27785,#6426);
#4995=LINE('',#27786,#6427);
#4996=LINE('',#27791,#6428);
#4997=LINE('',#27793,#6429);
#4998=LINE('',#27795,#6430);
#4999=LINE('',#27796,#6431);
#5000=LINE('',#27799,#6432);
#5001=LINE('',#27801,#6433);
#5002=LINE('',#27802,#6434);
#5003=LINE('',#27805,#6435);
#5004=LINE('',#27807,#6436);
#5005=LINE('',#27808,#6437);
#5006=LINE('',#27810,#6438);
#5007=LINE('',#27811,#6439);
#5008=LINE('',#27816,#6440);
#5009=LINE('',#27818,#6441);
#5010=LINE('',#27820,#6442);
#5011=LINE('',#27821,#6443);
#5012=LINE('',#27824,#6444);
#5013=LINE('',#27826,#6445);
#5014=LINE('',#27827,#6446);
#5015=LINE('',#27830,#6447);
#5016=LINE('',#27832,#6448);
#5017=LINE('',#27833,#6449);
#5018=LINE('',#27835,#6450);
#5019=LINE('',#27836,#6451);
#5020=LINE('',#27841,#6452);
#5021=LINE('',#27843,#6453);
#5022=LINE('',#27845,#6454);
#5023=LINE('',#27846,#6455);
#5024=LINE('',#27849,#6456);
#5025=LINE('',#27851,#6457);
#5026=LINE('',#27852,#6458);
#5027=LINE('',#27855,#6459);
#5028=LINE('',#27857,#6460);
#5029=LINE('',#27858,#6461);
#5030=LINE('',#27860,#6462);
#5031=LINE('',#27861,#6463);
#5032=LINE('',#27866,#6464);
#5033=LINE('',#27868,#6465);
#5034=LINE('',#27870,#6466);
#5035=LINE('',#27871,#6467);
#5036=LINE('',#27874,#6468);
#5037=LINE('',#27876,#6469);
#5038=LINE('',#27877,#6470);
#5039=LINE('',#27880,#6471);
#5040=LINE('',#27882,#6472);
#5041=LINE('',#27883,#6473);
#5042=LINE('',#27885,#6474);
#5043=LINE('',#27886,#6475);
#5044=LINE('',#27891,#6476);
#5045=LINE('',#27893,#6477);
#5046=LINE('',#27895,#6478);
#5047=LINE('',#27896,#6479);
#5048=LINE('',#27899,#6480);
#5049=LINE('',#27901,#6481);
#5050=LINE('',#27902,#6482);
#5051=LINE('',#27905,#6483);
#5052=LINE('',#27907,#6484);
#5053=LINE('',#27908,#6485);
#5054=LINE('',#27910,#6486);
#5055=LINE('',#27911,#6487);
#5056=LINE('',#27916,#6488);
#5057=LINE('',#27918,#6489);
#5058=LINE('',#27920,#6490);
#5059=LINE('',#27921,#6491);
#5060=LINE('',#27924,#6492);
#5061=LINE('',#27926,#6493);
#5062=LINE('',#27927,#6494);
#5063=LINE('',#27930,#6495);
#5064=LINE('',#27932,#6496);
#5065=LINE('',#27933,#6497);
#5066=LINE('',#27935,#6498);
#5067=LINE('',#27936,#6499);
#5068=LINE('',#27941,#6500);
#5069=LINE('',#27943,#6501);
#5070=LINE('',#27945,#6502);
#5071=LINE('',#27946,#6503);
#5072=LINE('',#27949,#6504);
#5073=LINE('',#27951,#6505);
#5074=LINE('',#27952,#6506);
#5075=LINE('',#27955,#6507);
#5076=LINE('',#27957,#6508);
#5077=LINE('',#27958,#6509);
#5078=LINE('',#27960,#6510);
#5079=LINE('',#27961,#6511);
#5080=LINE('',#27966,#6512);
#5081=LINE('',#27968,#6513);
#5082=LINE('',#27970,#6514);
#5083=LINE('',#27971,#6515);
#5084=LINE('',#27974,#6516);
#5085=LINE('',#27976,#6517);
#5086=LINE('',#27977,#6518);
#5087=LINE('',#27980,#6519);
#5088=LINE('',#27982,#6520);
#5089=LINE('',#27983,#6521);
#5090=LINE('',#27985,#6522);
#5091=LINE('',#27986,#6523);
#5092=LINE('',#27991,#6524);
#5093=LINE('',#27993,#6525);
#5094=LINE('',#27995,#6526);
#5095=LINE('',#27996,#6527);
#5096=LINE('',#27999,#6528);
#5097=LINE('',#28001,#6529);
#5098=LINE('',#28002,#6530);
#5099=LINE('',#28005,#6531);
#5100=LINE('',#28007,#6532);
#5101=LINE('',#28008,#6533);
#5102=LINE('',#28010,#6534);
#5103=LINE('',#28011,#6535);
#5104=LINE('',#28016,#6536);
#5105=LINE('',#28018,#6537);
#5106=LINE('',#28020,#6538);
#5107=LINE('',#28021,#6539);
#5108=LINE('',#28024,#6540);
#5109=LINE('',#28026,#6541);
#5110=LINE('',#28027,#6542);
#5111=LINE('',#28030,#6543);
#5112=LINE('',#28032,#6544);
#5113=LINE('',#28033,#6545);
#5114=LINE('',#28035,#6546);
#5115=LINE('',#28036,#6547);
#5116=LINE('',#28041,#6548);
#5117=LINE('',#28043,#6549);
#5118=LINE('',#28045,#6550);
#5119=LINE('',#28046,#6551);
#5120=LINE('',#28049,#6552);
#5121=LINE('',#28051,#6553);
#5122=LINE('',#28052,#6554);
#5123=LINE('',#28055,#6555);
#5124=LINE('',#28057,#6556);
#5125=LINE('',#28058,#6557);
#5126=LINE('',#28060,#6558);
#5127=LINE('',#28061,#6559);
#5128=LINE('',#28066,#6560);
#5129=LINE('',#28068,#6561);
#5130=LINE('',#28070,#6562);
#5131=LINE('',#28071,#6563);
#5132=LINE('',#28074,#6564);
#5133=LINE('',#28076,#6565);
#5134=LINE('',#28077,#6566);
#5135=LINE('',#28080,#6567);
#5136=LINE('',#28082,#6568);
#5137=LINE('',#28083,#6569);
#5138=LINE('',#28085,#6570);
#5139=LINE('',#28086,#6571);
#5140=LINE('',#28091,#6572);
#5141=LINE('',#28093,#6573);
#5142=LINE('',#28095,#6574);
#5143=LINE('',#28096,#6575);
#5144=LINE('',#28099,#6576);
#5145=LINE('',#28101,#6577);
#5146=LINE('',#28102,#6578);
#5147=LINE('',#28105,#6579);
#5148=LINE('',#28107,#6580);
#5149=LINE('',#28108,#6581);
#5150=LINE('',#28110,#6582);
#5151=LINE('',#28111,#6583);
#5152=LINE('',#28116,#6584);
#5153=LINE('',#28118,#6585);
#5154=LINE('',#28120,#6586);
#5155=LINE('',#28121,#6587);
#5156=LINE('',#28124,#6588);
#5157=LINE('',#28126,#6589);
#5158=LINE('',#28127,#6590);
#5159=LINE('',#28130,#6591);
#5160=LINE('',#28132,#6592);
#5161=LINE('',#28133,#6593);
#5162=LINE('',#28135,#6594);
#5163=LINE('',#28136,#6595);
#5164=LINE('',#28141,#6596);
#5165=LINE('',#28143,#6597);
#5166=LINE('',#28145,#6598);
#5167=LINE('',#28146,#6599);
#5168=LINE('',#28149,#6600);
#5169=LINE('',#28151,#6601);
#5170=LINE('',#28152,#6602);
#5171=LINE('',#28155,#6603);
#5172=LINE('',#28157,#6604);
#5173=LINE('',#28158,#6605);
#5174=LINE('',#28160,#6606);
#5175=LINE('',#28161,#6607);
#5176=LINE('',#28166,#6608);
#5177=LINE('',#28168,#6609);
#5178=LINE('',#28170,#6610);
#5179=LINE('',#28171,#6611);
#5180=LINE('',#28174,#6612);
#5181=LINE('',#28176,#6613);
#5182=LINE('',#28177,#6614);
#5183=LINE('',#28180,#6615);
#5184=LINE('',#28182,#6616);
#5185=LINE('',#28183,#6617);
#5186=LINE('',#28185,#6618);
#5187=LINE('',#28186,#6619);
#5188=LINE('',#28191,#6620);
#5189=LINE('',#28193,#6621);
#5190=LINE('',#28195,#6622);
#5191=LINE('',#28196,#6623);
#5192=LINE('',#28199,#6624);
#5193=LINE('',#28201,#6625);
#5194=LINE('',#28202,#6626);
#5195=LINE('',#28205,#6627);
#5196=LINE('',#28207,#6628);
#5197=LINE('',#28208,#6629);
#5198=LINE('',#28210,#6630);
#5199=LINE('',#28211,#6631);
#5200=LINE('',#28216,#6632);
#5201=LINE('',#28218,#6633);
#5202=LINE('',#28220,#6634);
#5203=LINE('',#28221,#6635);
#5204=LINE('',#28224,#6636);
#5205=LINE('',#28226,#6637);
#5206=LINE('',#28227,#6638);
#5207=LINE('',#28230,#6639);
#5208=LINE('',#28232,#6640);
#5209=LINE('',#28233,#6641);
#5210=LINE('',#28235,#6642);
#5211=LINE('',#28236,#6643);
#5212=LINE('',#28242,#6644);
#5213=LINE('',#28248,#6645);
#5214=LINE('',#28253,#6646);
#5215=LINE('',#28255,#6647);
#5216=LINE('',#28257,#6648);
#5217=LINE('',#28258,#6649);
#5218=LINE('',#28261,#6650);
#5219=LINE('',#28263,#6651);
#5220=LINE('',#28264,#6652);
#5221=LINE('',#28267,#6653);
#5222=LINE('',#28269,#6654);
#5223=LINE('',#28270,#6655);
#5224=LINE('',#28272,#6656);
#5225=LINE('',#28273,#6657);
#5226=LINE('',#28281,#6658);
#5227=LINE('',#28286,#6659);
#5228=LINE('',#28291,#6660);
#5229=LINE('',#28297,#6661);
#5230=LINE('',#28301,#6662);
#5231=LINE('',#28304,#6663);
#5232=LINE('',#28308,#6664);
#5233=LINE('',#28312,#6665);
#5234=LINE('',#28315,#6666);
#5235=LINE('',#28318,#6667);
#5236=LINE('',#28320,#6668);
#5237=LINE('',#28322,#6669);
#5238=LINE('',#28324,#6670);
#5239=LINE('',#28325,#6671);
#5240=LINE('',#28330,#6672);
#5241=LINE('',#28332,#6673);
#5242=LINE('',#28333,#6674);
#5243=LINE('',#28339,#6675);
#5244=LINE('',#28341,#6676);
#5245=LINE('',#28342,#6677);
#5246=LINE('',#28344,#6678);
#5247=LINE('',#28345,#6679);
#5248=LINE('',#28352,#6680);
#5249=LINE('',#28356,#6681);
#5250=LINE('',#28361,#6682);
#5251=LINE('',#28365,#6683);
#5252=LINE('',#28370,#6684);
#5253=LINE('',#28374,#6685);
#5254=LINE('',#28376,#6686);
#5255=LINE('',#28377,#6687);
#5256=LINE('',#28379,#6688);
#5257=LINE('',#28381,#6689);
#5258=LINE('',#28383,#6690);
#5259=LINE('',#28385,#6691);
#5260=LINE('',#28387,#6692);
#5261=LINE('',#28388,#6693);
#5262=LINE('',#28391,#6694);
#5263=LINE('',#28392,#6695);
#5264=LINE('',#28395,#6696);
#5265=LINE('',#28396,#6697);
#5266=LINE('',#28398,#6698);
#5267=LINE('',#28401,#6699);
#5268=LINE('',#28402,#6700);
#5269=LINE('',#28405,#6701);
#5270=LINE('',#28406,#6702);
#5271=LINE('',#28409,#6703);
#5272=LINE('',#28410,#6704);
#5273=LINE('',#28413,#6705);
#5274=LINE('',#28414,#6706);
#5275=LINE('',#28417,#6707);
#5276=LINE('',#28418,#6708);
#5277=LINE('',#28420,#6709);
#5278=LINE('',#28426,#6710);
#5279=LINE('',#28428,#6711);
#5280=LINE('',#28430,#6712);
#5281=LINE('',#28431,#6713);
#5282=LINE('',#28434,#6714);
#5283=LINE('',#28436,#6715);
#5284=LINE('',#28437,#6716);
#5285=LINE('',#28440,#6717);
#5286=LINE('',#28442,#6718);
#5287=LINE('',#28443,#6719);
#5288=LINE('',#28446,#6720);
#5289=LINE('',#28448,#6721);
#5290=LINE('',#28449,#6722);
#5291=LINE('',#28452,#6723);
#5292=LINE('',#28454,#6724);
#5293=LINE('',#28455,#6725);
#5294=LINE('',#28457,#6726);
#5295=LINE('',#28458,#6727);
#5296=LINE('',#28470,#6728);
#5297=LINE('',#28474,#6729);
#5298=LINE('',#28478,#6730);
#5299=LINE('',#28485,#6731);
#5300=LINE('',#28487,#6732);
#5301=LINE('',#28502,#6733);
#5302=LINE('',#28508,#6734);
#5303=LINE('',#28512,#6735);
#5304=LINE('',#28518,#6736);
#5305=LINE('',#28523,#6737);
#5306=LINE('',#28538,#6738);
#5307=LINE('',#28547,#6739);
#5308=LINE('',#28551,#6740);
#5309=LINE('',#28555,#6741);
#5310=LINE('',#28558,#6742);
#5311=LINE('',#28694,#6743);
#5312=LINE('',#28947,#6744);
#5313=LINE('',#28989,#6745);
#5314=LINE('',#28994,#6746);
#5315=LINE('',#29003,#6747);
#5316=LINE('',#29008,#6748);
#5317=LINE('',#29028,#6749);
#5318=LINE('',#29034,#6750);
#5319=LINE('',#29038,#6751);
#5320=LINE('',#29044,#6752);
#5321=LINE('',#29049,#6753);
#5322=LINE('',#29064,#6754);
#5323=LINE('',#29073,#6755);
#5324=LINE('',#29077,#6756);
#5325=LINE('',#29081,#6757);
#5326=LINE('',#29084,#6758);
#5327=LINE('',#29237,#6759);
#5328=LINE('',#29533,#6760);
#5329=LINE('',#29575,#6761);
#5330=LINE('',#29580,#6762);
#5331=LINE('',#29589,#6763);
#5332=LINE('',#29594,#6764);
#5333=LINE('',#29610,#6765);
#5334=LINE('',#29617,#6766);
#5335=LINE('',#29621,#6767);
#5336=LINE('',#29625,#6768);
#5337=LINE('',#29632,#6769);
#5338=LINE('',#29634,#6770);
#5339=LINE('',#29638,#6771);
#5340=LINE('',#29640,#6772);
#5341=LINE('',#29642,#6773);
#5342=LINE('',#29643,#6774);
#5343=LINE('',#29646,#6775);
#5344=LINE('',#29648,#6776);
#5345=LINE('',#29649,#6777);
#5346=LINE('',#29652,#6778);
#5347=LINE('',#29654,#6779);
#5348=LINE('',#29655,#6780);
#5349=LINE('',#29658,#6781);
#5350=LINE('',#29660,#6782);
#5351=LINE('',#29661,#6783);
#5352=LINE('',#29664,#6784);
#5353=LINE('',#29666,#6785);
#5354=LINE('',#29667,#6786);
#5355=LINE('',#29669,#6787);
#5356=LINE('',#29670,#6788);
#5357=LINE('',#29677,#6789);
#5358=LINE('',#29679,#6790);
#5359=LINE('',#29681,#6791);
#5360=LINE('',#29682,#6792);
#5361=LINE('',#29685,#6793);
#5362=LINE('',#29687,#6794);
#5363=LINE('',#29688,#6795);
#5364=LINE('',#29691,#6796);
#5365=LINE('',#29693,#6797);
#5366=LINE('',#29694,#6798);
#5367=LINE('',#29697,#6799);
#5368=LINE('',#29699,#6800);
#5369=LINE('',#29700,#6801);
#5370=LINE('',#29703,#6802);
#5371=LINE('',#29705,#6803);
#5372=LINE('',#29706,#6804);
#5373=LINE('',#29708,#6805);
#5374=LINE('',#29709,#6806);
#5375=LINE('',#29721,#6807);
#5376=LINE('',#29725,#6808);
#5377=LINE('',#29729,#6809);
#5378=LINE('',#29736,#6810);
#5379=LINE('',#29738,#6811);
#5380=LINE('',#29743,#6812);
#5381=LINE('',#29745,#6813);
#5382=LINE('',#29747,#6814);
#5383=LINE('',#29748,#6815);
#5384=LINE('',#29751,#6816);
#5385=LINE('',#29753,#6817);
#5386=LINE('',#29754,#6818);
#5387=LINE('',#29757,#6819);
#5388=LINE('',#29759,#6820);
#5389=LINE('',#29760,#6821);
#5390=LINE('',#29763,#6822);
#5391=LINE('',#29765,#6823);
#5392=LINE('',#29766,#6824);
#5393=LINE('',#29769,#6825);
#5394=LINE('',#29771,#6826);
#5395=LINE('',#29772,#6827);
#5396=LINE('',#29775,#6828);
#5397=LINE('',#29777,#6829);
#5398=LINE('',#29778,#6830);
#5399=LINE('',#29781,#6831);
#5400=LINE('',#29783,#6832);
#5401=LINE('',#29784,#6833);
#5402=LINE('',#29787,#6834);
#5403=LINE('',#29789,#6835);
#5404=LINE('',#29790,#6836);
#5405=LINE('',#29793,#6837);
#5406=LINE('',#29795,#6838);
#5407=LINE('',#29796,#6839);
#5408=LINE('',#29800,#6840);
#5409=LINE('',#29802,#6841);
#5410=LINE('',#29804,#6842);
#5411=LINE('',#29805,#6843);
#5412=LINE('',#29808,#6844);
#5413=LINE('',#29810,#6845);
#5414=LINE('',#29811,#6846);
#5415=LINE('',#29814,#6847);
#5416=LINE('',#29816,#6848);
#5417=LINE('',#29817,#6849);
#5418=LINE('',#29820,#6850);
#5419=LINE('',#29822,#6851);
#5420=LINE('',#29823,#6852);
#5421=LINE('',#29826,#6853);
#5422=LINE('',#29828,#6854);
#5423=LINE('',#29829,#6855);
#5424=LINE('',#29832,#6856);
#5425=LINE('',#29834,#6857);
#5426=LINE('',#29835,#6858);
#5427=LINE('',#29838,#6859);
#5428=LINE('',#29840,#6860);
#5429=LINE('',#29841,#6861);
#5430=LINE('',#29844,#6862);
#5431=LINE('',#29846,#6863);
#5432=LINE('',#29847,#6864);
#5433=LINE('',#29850,#6865);
#5434=LINE('',#29852,#6866);
#5435=LINE('',#29853,#6867);
#5436=LINE('',#29857,#6868);
#5437=LINE('',#29859,#6869);
#5438=LINE('',#29861,#6870);
#5439=LINE('',#29862,#6871);
#5440=LINE('',#29865,#6872);
#5441=LINE('',#29867,#6873);
#5442=LINE('',#29868,#6874);
#5443=LINE('',#29871,#6875);
#5444=LINE('',#29873,#6876);
#5445=LINE('',#29874,#6877);
#5446=LINE('',#29877,#6878);
#5447=LINE('',#29879,#6879);
#5448=LINE('',#29880,#6880);
#5449=LINE('',#29883,#6881);
#5450=LINE('',#29885,#6882);
#5451=LINE('',#29886,#6883);
#5452=LINE('',#29889,#6884);
#5453=LINE('',#29891,#6885);
#5454=LINE('',#29892,#6886);
#5455=LINE('',#29895,#6887);
#5456=LINE('',#29897,#6888);
#5457=LINE('',#29898,#6889);
#5458=LINE('',#29901,#6890);
#5459=LINE('',#29903,#6891);
#5460=LINE('',#29904,#6892);
#5461=LINE('',#29907,#6893);
#5462=LINE('',#29909,#6894);
#5463=LINE('',#29910,#6895);
#5464=LINE('',#29914,#6896);
#5465=LINE('',#29916,#6897);
#5466=LINE('',#29918,#6898);
#5467=LINE('',#29919,#6899);
#5468=LINE('',#29922,#6900);
#5469=LINE('',#29924,#6901);
#5470=LINE('',#29925,#6902);
#5471=LINE('',#29928,#6903);
#5472=LINE('',#29930,#6904);
#5473=LINE('',#29931,#6905);
#5474=LINE('',#29934,#6906);
#5475=LINE('',#29936,#6907);
#5476=LINE('',#29937,#6908);
#5477=LINE('',#29940,#6909);
#5478=LINE('',#29942,#6910);
#5479=LINE('',#29943,#6911);
#5480=LINE('',#29946,#6912);
#5481=LINE('',#29948,#6913);
#5482=LINE('',#29949,#6914);
#5483=LINE('',#29952,#6915);
#5484=LINE('',#29954,#6916);
#5485=LINE('',#29955,#6917);
#5486=LINE('',#29958,#6918);
#5487=LINE('',#29960,#6919);
#5488=LINE('',#29961,#6920);
#5489=LINE('',#29964,#6921);
#5490=LINE('',#29966,#6922);
#5491=LINE('',#29967,#6923);
#5492=LINE('',#29972,#6924);
#5493=LINE('',#29976,#6925);
#5494=LINE('',#29978,#6926);
#5495=LINE('',#29979,#6927);
#5496=LINE('',#29982,#6928);
#5497=LINE('',#29984,#6929);
#5498=LINE('',#29985,#6930);
#5499=LINE('',#29987,#6931);
#5500=LINE('',#29988,#6932);
#5501=LINE('',#29991,#6933);
#5502=LINE('',#29993,#6934);
#5503=LINE('',#29994,#6935);
#5504=LINE('',#29996,#6936);
#5505=LINE('',#29997,#6937);
#5506=LINE('',#30000,#6938);
#5507=LINE('',#30002,#6939);
#5508=LINE('',#30003,#6940);
#5509=LINE('',#30005,#6941);
#5510=LINE('',#30006,#6942);
#5511=LINE('',#30008,#6943);
#5512=LINE('',#30009,#6944);
#5513=LINE('',#30019,#6945);
#5514=LINE('',#30023,#6946);
#5515=LINE('',#30027,#6947);
#5516=LINE('',#30034,#6948);
#5517=LINE('',#30038,#6949);
#5518=LINE('',#30042,#6950);
#5519=LINE('',#30047,#6951);
#5520=LINE('',#30049,#6952);
#5521=LINE('',#30051,#6953);
#5522=LINE('',#30052,#6954);
#5523=LINE('',#30055,#6955);
#5524=LINE('',#30057,#6956);
#5525=LINE('',#30058,#6957);
#5526=LINE('',#30061,#6958);
#5527=LINE('',#30063,#6959);
#5528=LINE('',#30064,#6960);
#5529=LINE('',#30067,#6961);
#5530=LINE('',#30069,#6962);
#5531=LINE('',#30070,#6963);
#5532=LINE('',#30073,#6964);
#5533=LINE('',#30075,#6965);
#5534=LINE('',#30076,#6966);
#5535=LINE('',#30078,#6967);
#5536=LINE('',#30079,#6968);
#5537=LINE('',#30086,#6969);
#5538=LINE('',#30088,#6970);
#5539=LINE('',#30090,#6971);
#5540=LINE('',#30091,#6972);
#5541=LINE('',#30094,#6973);
#5542=LINE('',#30096,#6974);
#5543=LINE('',#30097,#6975);
#5544=LINE('',#30100,#6976);
#5545=LINE('',#30102,#6977);
#5546=LINE('',#30103,#6978);
#5547=LINE('',#30108,#6979);
#5548=LINE('',#30110,#6980);
#5549=LINE('',#30112,#6981);
#5550=LINE('',#30114,#6982);
#5551=LINE('',#30116,#6983);
#5552=LINE('',#30118,#6984);
#5553=LINE('',#30119,#6985);
#5554=LINE('',#30122,#6986);
#5555=LINE('',#30123,#6987);
#5556=LINE('',#30126,#6988);
#5557=LINE('',#30127,#6989);
#5558=LINE('',#30130,#6990);
#5559=LINE('',#30132,#6991);
#5560=LINE('',#30134,#6992);
#5561=LINE('',#30136,#6993);
#5562=LINE('',#30137,#6994);
#5563=LINE('',#30139,#6995);
#5564=LINE('',#30142,#6996);
#5565=LINE('',#30145,#6997);
#5566=LINE('',#30149,#6998);
#5567=LINE('',#30156,#6999);
#5568=LINE('',#30158,#7000);
#5569=LINE('',#30160,#7001);
#5570=LINE('',#30168,#7002);
#5571=LINE('',#30170,#7003);
#5572=LINE('',#30172,#7004);
#5573=LINE('',#30174,#7005);
#5574=LINE('',#30176,#7006);
#5575=LINE('',#30177,#7007);
#5576=LINE('',#30184,#7008);
#5577=LINE('',#30188,#7009);
#5578=LINE('',#30192,#7010);
#5579=LINE('',#30199,#7011);
#5580=LINE('',#30201,#7012);
#5581=LINE('',#30205,#7013);
#5582=LINE('',#30206,#7014);
#5583=LINE('',#30207,#7015);
#5584=LINE('',#30210,#7016);
#5585=LINE('',#30211,#7017);
#5586=LINE('',#30214,#7018);
#5587=LINE('',#30215,#7019);
#5588=LINE('',#30218,#7020);
#5589=LINE('',#30219,#7021);
#5590=LINE('',#30222,#7022);
#5591=LINE('',#30223,#7023);
#5592=LINE('',#30225,#7024);
#5593=LINE('',#30233,#7025);
#5594=LINE('',#30239,#7026);
#5595=LINE('',#30245,#7027);
#5596=LINE('',#30251,#7028);
#5597=LINE('',#30257,#7029);
#5598=LINE('',#30263,#7030);
#5599=LINE('',#30269,#7031);
#5600=LINE('',#30275,#7032);
#5601=LINE('',#30281,#7033);
#5602=LINE('',#30287,#7034);
#5603=LINE('',#30293,#7035);
#5604=LINE('',#30299,#7036);
#5605=LINE('',#30305,#7037);
#5606=LINE('',#30311,#7038);
#5607=LINE('',#30317,#7039);
#5608=LINE('',#30323,#7040);
#5609=LINE('',#30329,#7041);
#5610=LINE('',#30335,#7042);
#5611=LINE('',#30340,#7043);
#5612=LINE('',#30342,#7044);
#5613=LINE('',#30344,#7045);
#5614=LINE('',#30345,#7046);
#5615=LINE('',#30348,#7047);
#5616=LINE('',#30350,#7048);
#5617=LINE('',#30351,#7049);
#5618=LINE('',#30354,#7050);
#5619=LINE('',#30356,#7051);
#5620=LINE('',#30357,#7052);
#5621=LINE('',#30359,#7053);
#5622=LINE('',#30360,#7054);
#5623=LINE('',#30371,#7055);
#5624=LINE('',#30375,#7056);
#5625=LINE('',#30379,#7057);
#5626=LINE('',#30387,#7058);
#5627=LINE('',#30391,#7059);
#5628=LINE('',#30395,#7060);
#5629=LINE('',#30405,#7061);
#5630=LINE('',#30408,#7062);
#5631=LINE('',#30410,#7063);
#5632=LINE('',#30421,#7064);
#5633=LINE('',#30424,#7065);
#5634=LINE('',#30426,#7066);
#5635=LINE('',#30432,#7067);
#5636=LINE('',#30442,#7068);
#5637=LINE('',#30453,#7069);
#5638=LINE('',#30456,#7070);
#5639=LINE('',#30468,#7071);
#5640=LINE('',#30472,#7072);
#5641=LINE('',#30476,#7073);
#5642=LINE('',#30484,#7074);
#5643=LINE('',#30488,#7075);
#5644=LINE('',#30492,#7076);
#5645=LINE('',#30502,#7077);
#5646=LINE('',#30505,#7078);
#5647=LINE('',#30507,#7079);
#5648=LINE('',#30518,#7080);
#5649=LINE('',#30521,#7081);
#5650=LINE('',#30523,#7082);
#5651=LINE('',#30529,#7083);
#5652=LINE('',#30539,#7084);
#5653=LINE('',#30550,#7085);
#5654=LINE('',#30553,#7086);
#5655=LINE('',#30562,#7087);
#5656=LINE('',#30569,#7088);
#5657=LINE('',#30576,#7089);
#5658=LINE('',#30583,#7090);
#5659=LINE('',#30589,#7091);
#5660=LINE('',#30598,#7092);
#5661=LINE('',#30604,#7093);
#5662=LINE('',#30610,#7094);
#5663=LINE('',#30619,#7095);
#5664=LINE('',#30625,#7096);
#5665=LINE('',#30630,#7097);
#5666=LINE('',#30632,#7098);
#5667=LINE('',#30634,#7099);
#5668=LINE('',#30635,#7100);
#5669=LINE('',#30638,#7101);
#5670=LINE('',#30640,#7102);
#5671=LINE('',#30641,#7103);
#5672=LINE('',#30643,#7104);
#5673=LINE('',#30647,#7105);
#5674=LINE('',#30649,#7106);
#5675=LINE('',#30651,#7107);
#5676=LINE('',#30652,#7108);
#5677=LINE('',#30655,#7109);
#5678=LINE('',#30657,#7110);
#5679=LINE('',#30658,#7111);
#5680=LINE('',#30661,#7112);
#5681=LINE('',#30663,#7113);
#5682=LINE('',#30664,#7114);
#5683=LINE('',#30666,#7115);
#5684=LINE('',#30669,#7116);
#5685=LINE('',#30671,#7117);
#5686=LINE('',#30673,#7118);
#5687=LINE('',#30675,#7119);
#5688=LINE('',#30676,#7120);
#5689=LINE('',#30679,#7121);
#5690=LINE('',#30681,#7122);
#5691=LINE('',#30682,#7123);
#5692=LINE('',#30685,#7124);
#5693=LINE('',#30687,#7125);
#5694=LINE('',#30688,#7126);
#5695=LINE('',#30690,#7127);
#5696=LINE('',#30691,#7128);
#5697=LINE('',#30692,#7129);
#5698=LINE('',#30702,#7130);
#5699=LINE('',#30704,#7131);
#5700=LINE('',#30705,#7132);
#5701=LINE('',#30708,#7133);
#5702=LINE('',#30710,#7134);
#5703=LINE('',#30711,#7135);
#5704=LINE('',#30716,#7136);
#5705=LINE('',#30717,#7137);
#5706=LINE('',#30719,#7138);
#5707=LINE('',#30720,#7139);
#5708=LINE('',#30730,#7140);
#5709=LINE('',#30737,#7141);
#5710=LINE('',#30744,#7142);
#5711=LINE('',#30751,#7143);
#5712=LINE('',#30758,#7144);
#5713=LINE('',#30763,#7145);
#5714=LINE('',#30770,#7146);
#5715=LINE('',#30773,#7147);
#5716=LINE('',#30776,#7148);
#5717=LINE('',#30778,#7149);
#5718=LINE('',#30779,#7150);
#5719=LINE('',#30785,#7151);
#5720=LINE('',#30787,#7152);
#5721=LINE('',#30788,#7153);
#5722=LINE('',#30797,#7154);
#5723=LINE('',#30802,#7155);
#5724=LINE('',#30809,#7156);
#5725=LINE('',#30881,#7157);
#5726=LINE('',#30968,#7158);
#5727=LINE('',#31058,#7159);
#5728=LINE('',#31145,#7160);
#5729=LINE('',#31235,#7161);
#5730=LINE('',#31322,#7162);
#5731=LINE('',#31409,#7163);
#5732=LINE('',#31499,#7164);
#5733=LINE('',#31515,#7165);
#5734=LINE('',#31541,#7166);
#5735=LINE('',#31578,#7167);
#5736=LINE('',#31615,#7168);
#5737=LINE('',#31653,#7169);
#5738=LINE('',#31690,#7170);
#5739=LINE('',#31727,#7171);
#5740=LINE('',#31765,#7172);
#5741=LINE('',#31803,#7173);
#5742=LINE('',#32968,#7174);
#5743=LINE('',#32980,#7175);
#5744=LINE('',#32984,#7176);
#5745=LINE('',#32988,#7177);
#5746=LINE('',#32992,#7178);
#5747=LINE('',#32993,#7179);
#5748=LINE('',#32994,#7180);
#5749=LINE('',#33003,#7181);
#5750=LINE('',#33010,#7182);
#5751=LINE('',#33012,#7183);
#5752=LINE('',#33014,#7184);
#5753=LINE('',#33015,#7185);
#5754=LINE('',#33018,#7186);
#5755=LINE('',#33020,#7187);
#5756=LINE('',#33021,#7188);
#5757=LINE('',#33024,#7189);
#5758=LINE('',#33026,#7190);
#5759=LINE('',#33027,#7191);
#5760=LINE('',#33030,#7192);
#5761=LINE('',#33032,#7193);
#5762=LINE('',#33033,#7194);
#5763=LINE('',#33036,#7195);
#5764=LINE('',#33038,#7196);
#5765=LINE('',#33039,#7197);
#5766=LINE('',#33041,#7198);
#5767=LINE('',#33042,#7199);
#5768=LINE('',#33052,#7200);
#5769=LINE('',#33061,#7201);
#5770=LINE('',#33065,#7202);
#5771=LINE('',#33069,#7203);
#5772=LINE('',#33076,#7204);
#5773=LINE('',#33078,#7205);
#5774=LINE('',#33086,#7206);
#5775=LINE('',#33090,#7207);
#5776=LINE('',#33094,#7208);
#5777=LINE('',#33101,#7209);
#5778=LINE('',#33105,#7210);
#5779=LINE('',#33109,#7211);
#5780=LINE('',#33114,#7212);
#5781=LINE('',#33116,#7213);
#5782=LINE('',#33118,#7214);
#5783=LINE('',#33119,#7215);
#5784=LINE('',#33122,#7216);
#5785=LINE('',#33124,#7217);
#5786=LINE('',#33125,#7218);
#5787=LINE('',#33128,#7219);
#5788=LINE('',#33130,#7220);
#5789=LINE('',#33131,#7221);
#5790=LINE('',#33134,#7222);
#5791=LINE('',#33136,#7223);
#5792=LINE('',#33137,#7224);
#5793=LINE('',#33140,#7225);
#5794=LINE('',#33142,#7226);
#5795=LINE('',#33143,#7227);
#5796=LINE('',#33145,#7228);
#5797=LINE('',#33146,#7229);
#5798=LINE('',#33262,#7230);
#5799=LINE('',#33292,#7231);
#5800=LINE('',#33379,#7232);
#5801=LINE('',#33469,#7233);
#5802=LINE('',#33556,#7234);
#5803=LINE('',#33643,#7235);
#5804=LINE('',#33730,#7236);
#5805=LINE('',#33817,#7237);
#5806=LINE('',#33904,#7238);
#5807=LINE('',#33976,#7239);
#5808=LINE('',#34027,#7240);
#5809=LINE('',#34075,#7241);
#5810=LINE('',#34123,#7242);
#5811=LINE('',#34174,#7243);
#5812=LINE('',#34225,#7244);
#5813=LINE('',#34273,#7245);
#5814=LINE('',#34324,#7246);
#5815=LINE('',#34375,#7247);
#5816=LINE('',#34423,#7248);
#5817=LINE('',#34471,#7249);
#5818=LINE('',#34522,#7250);
#5819=LINE('',#34573,#7251);
#5820=LINE('',#34621,#7252);
#5821=LINE('',#34672,#7253);
#5822=LINE('',#34723,#7254);
#5823=LINE('',#34771,#7255);
#5824=LINE('',#34819,#7256);
#5825=LINE('',#34870,#7257);
#5826=LINE('',#34921,#7258);
#5827=LINE('',#34969,#7259);
#5828=LINE('',#35020,#7260);
#5829=LINE('',#35071,#7261);
#5830=LINE('',#35119,#7262);
#5831=LINE('',#35167,#7263);
#5832=LINE('',#35218,#7264);
#5833=LINE('',#35269,#7265);
#5834=LINE('',#35317,#7266);
#5835=LINE('',#35368,#7267);
#5836=LINE('',#35419,#7268);
#5837=LINE('',#35467,#7269);
#5838=LINE('',#35515,#7270);
#5839=LINE('',#35566,#7271);
#5840=LINE('',#35617,#7272);
#5841=LINE('',#35665,#7273);
#5842=LINE('',#35716,#7274);
#5843=LINE('',#35767,#7275);
#5844=LINE('',#35815,#7276);
#5845=LINE('',#35863,#7277);
#5846=LINE('',#35914,#7278);
#5847=LINE('',#35965,#7279);
#5848=LINE('',#36013,#7280);
#5849=LINE('',#36064,#7281);
#5850=LINE('',#36115,#7282);
#5851=LINE('',#36163,#7283);
#5852=LINE('',#36211,#7284);
#5853=LINE('',#36262,#7285);
#5854=LINE('',#36328,#7286);
#5855=LINE('',#36418,#7287);
#5856=LINE('',#36505,#7288);
#5857=LINE('',#36592,#7289);
#5858=LINE('',#36679,#7290);
#5859=LINE('',#36766,#7291);
#5860=LINE('',#36853,#7292);
#5861=LINE('',#36943,#7293);
#5862=LINE('',#36953,#7294);
#5863=LINE('',#36989,#7295);
#5864=LINE('',#37027,#7296);
#5865=LINE('',#37063,#7297);
#5866=LINE('',#37101,#7298);
#5867=LINE('',#37137,#7299);
#5868=LINE('',#37175,#7300);
#5869=LINE('',#37212,#7301);
#5870=LINE('',#37247,#7302);
#5871=LINE('',#37274,#7303);
#5872=LINE('',#37298,#7304);
#5873=LINE('',#37322,#7305);
#5874=LINE('',#37346,#7306);
#5875=LINE('',#37372,#7307);
#5876=LINE('',#37396,#7308);
#5877=LINE('',#37420,#7309);
#5878=LINE('',#37446,#7310);
#5879=LINE('',#37470,#7311);
#5880=LINE('',#37494,#7312);
#5881=LINE('',#37518,#7313);
#5882=LINE('',#37544,#7314);
#5883=LINE('',#37568,#7315);
#5884=LINE('',#37592,#7316);
#5885=LINE('',#37618,#7317);
#5886=LINE('',#37642,#7318);
#5887=LINE('',#37666,#7319);
#5888=LINE('',#37690,#7320);
#5889=LINE('',#37716,#7321);
#5890=LINE('',#37740,#7322);
#5891=LINE('',#37764,#7323);
#5892=LINE('',#37790,#7324);
#5893=LINE('',#37814,#7325);
#5894=LINE('',#37838,#7326);
#5895=LINE('',#37862,#7327);
#5896=LINE('',#37888,#7328);
#5897=LINE('',#37912,#7329);
#5898=LINE('',#37936,#7330);
#5899=LINE('',#37962,#7331);
#5900=LINE('',#37986,#7332);
#5901=LINE('',#38010,#7333);
#5902=LINE('',#38034,#7334);
#5903=LINE('',#38060,#7335);
#5904=LINE('',#38084,#7336);
#5905=LINE('',#38108,#7337);
#5906=LINE('',#38134,#7338);
#5907=LINE('',#38158,#7339);
#5908=LINE('',#38182,#7340);
#5909=LINE('',#38206,#7341);
#5910=LINE('',#38232,#7342);
#5911=LINE('',#38256,#7343);
#5912=LINE('',#38280,#7344);
#5913=LINE('',#38306,#7345);
#5914=LINE('',#38330,#7346);
#5915=LINE('',#38354,#7347);
#5916=LINE('',#38379,#7348);
#5917=LINE('',#38406,#7349);
#5918=LINE('',#38443,#7350);
#5919=LINE('',#38479,#7351);
#5920=LINE('',#38517,#7352);
#5921=LINE('',#38553,#7353);
#5922=LINE('',#38591,#7354);
#5923=LINE('',#38628,#7355);
#5924=LINE('',#38744,#7356);
#5925=LINE('',#42878,#7357);
#5926=LINE('',#42880,#7358);
#5927=LINE('',#42882,#7359);
#5928=LINE('',#42883,#7360);
#5929=LINE('',#42888,#7361);
#5930=LINE('',#42889,#7362);
#5931=LINE('',#42892,#7363);
#5932=LINE('',#42893,#7364);
#5933=LINE('',#42896,#7365);
#5934=LINE('',#42897,#7366);
#5935=LINE('',#42904,#7367);
#5936=LINE('',#42914,#7368);
#5937=LINE('',#42922,#7369);
#5938=LINE('',#42928,#7370);
#5939=LINE('',#42936,#7371);
#5940=LINE('',#42974,#7372);
#5941=LINE('',#43013,#7373);
#5942=LINE('',#43018,#7374);
#5943=LINE('',#43024,#7375);
#5944=LINE('',#43033,#7376);
#5945=LINE('',#43038,#7377);
#5946=LINE('',#43068,#7378);
#5947=LINE('',#43107,#7379);
#5948=LINE('',#43111,#7380);
#5949=LINE('',#43113,#7381);
#5950=LINE('',#43115,#7382);
#5951=LINE('',#43117,#7383);
#5952=LINE('',#43119,#7384);
#5953=LINE('',#43120,#7385);
#5954=LINE('',#43123,#7386);
#5955=LINE('',#43125,#7387);
#5956=LINE('',#43126,#7388);
#5957=LINE('',#43129,#7389);
#5958=LINE('',#43131,#7390);
#5959=LINE('',#43133,#7391);
#5960=LINE('',#43135,#7392);
#5961=LINE('',#43136,#7393);
#5962=LINE('',#43146,#7394);
#5963=LINE('',#43157,#7395);
#5964=LINE('',#43163,#7396);
#5965=LINE('',#43172,#7397);
#5966=LINE('',#43178,#7398);
#5967=LINE('',#43186,#7399);
#5968=LINE('',#43188,#7400);
#5969=LINE('',#43190,#7401);
#5970=LINE('',#43192,#7402);
#5971=LINE('',#43194,#7403);
#5972=LINE('',#43196,#7404);
#5973=LINE('',#43198,#7405);
#5974=LINE('',#43199,#7406);
#5975=LINE('',#43202,#7407);
#5976=LINE('',#43204,#7408);
#5977=LINE('',#43205,#7409);
#5978=LINE('',#43208,#7410);
#5979=LINE('',#43209,#7411);
#5980=LINE('',#43212,#7412);
#5981=LINE('',#43213,#7413);
#5982=LINE('',#43216,#7414);
#5983=LINE('',#43217,#7415);
#5984=LINE('',#43221,#7416);
#5985=LINE('',#43222,#7417);
#5986=LINE('',#43224,#7418);
#5987=LINE('',#43225,#7419);
#5988=LINE('',#43227,#7420);
#5989=LINE('',#43229,#7421);
#5990=LINE('',#43231,#7422);
#5991=LINE('',#43237,#7423);
#5992=LINE('',#43239,#7424);
#5993=LINE('',#43241,#7425);
#5994=LINE('',#43242,#7426);
#5995=LINE('',#43245,#7427);
#5996=LINE('',#43247,#7428);
#5997=LINE('',#43248,#7429);
#5998=LINE('',#43251,#7430);
#5999=LINE('',#43253,#7431);
#6000=LINE('',#43254,#7432);
#6001=LINE('',#43257,#7433);
#6002=LINE('',#43259,#7434);
#6003=LINE('',#43260,#7435);
#6004=LINE('',#43263,#7436);
#6005=LINE('',#43265,#7437);
#6006=LINE('',#43266,#7438);
#6007=LINE('',#43268,#7439);
#6008=LINE('',#43269,#7440);
#6009=LINE('',#43277,#7441);
#6010=LINE('',#43281,#7442);
#6011=LINE('',#43285,#7443);
#6012=LINE('',#43292,#7444);
#6013=LINE('',#43298,#7445);
#6014=LINE('',#43309,#7446);
#6015=LINE('',#43313,#7447);
#6016=LINE('',#43317,#7448);
#6017=LINE('',#43324,#7449);
#6018=LINE('',#43328,#7450);
#6019=LINE('',#43332,#7451);
#6020=LINE('',#43337,#7452);
#6021=LINE('',#43339,#7453);
#6022=LINE('',#43341,#7454);
#6023=LINE('',#43342,#7455);
#6024=LINE('',#43345,#7456);
#6025=LINE('',#43347,#7457);
#6026=LINE('',#43348,#7458);
#6027=LINE('',#43351,#7459);
#6028=LINE('',#43353,#7460);
#6029=LINE('',#43354,#7461);
#6030=LINE('',#43357,#7462);
#6031=LINE('',#43359,#7463);
#6032=LINE('',#43360,#7464);
#6033=LINE('',#43363,#7465);
#6034=LINE('',#43365,#7466);
#6035=LINE('',#43366,#7467);
#6036=LINE('',#43368,#7468);
#6037=LINE('',#43369,#7469);
#6038=VECTOR('',#21206,0.275);
#6039=VECTOR('',#21211,1.);
#6040=VECTOR('',#21212,1.);
#6041=VECTOR('',#21213,1.);
#6042=VECTOR('',#21214,1.);
#6043=VECTOR('',#21217,1.);
#6044=VECTOR('',#21218,1.);
#6045=VECTOR('',#21219,1.);
#6046=VECTOR('',#21222,1.);
#6047=VECTOR('',#21223,1.);
#6048=VECTOR('',#21224,1.);
#6049=VECTOR('',#21227,1.);
#6050=VECTOR('',#21228,1.);
#6051=VECTOR('',#21229,1.);
#6052=VECTOR('',#21232,1.);
#6053=VECTOR('',#21233,1.);
#6054=VECTOR('',#21234,1.);
#6055=VECTOR('',#21239,0.165);
#6056=VECTOR('',#21248,0.165);
#6057=VECTOR('',#21257,0.165);
#6058=VECTOR('',#21266,0.165);
#6059=VECTOR('',#21275,0.275);
#6060=VECTOR('',#21282,0.275);
#6061=VECTOR('',#21289,0.275);
#6062=VECTOR('',#21296,0.275);
#6063=VECTOR('',#21303,0.275);
#6064=VECTOR('',#21310,0.275);
#6065=VECTOR('',#21317,2.5);
#6066=VECTOR('',#21324,0.275);
#6067=VECTOR('',#21331,0.275);
#6068=VECTOR('',#21338,0.275);
#6069=VECTOR('',#21345,0.275);
#6070=VECTOR('',#21352,0.275);
#6071=VECTOR('',#21359,0.275);
#6072=VECTOR('',#21366,0.275);
#6073=VECTOR('',#21373,0.275);
#6074=VECTOR('',#21378,1.);
#6075=VECTOR('',#21379,1.);
#6076=VECTOR('',#21380,1.);
#6077=VECTOR('',#21383,1.);
#6078=VECTOR('',#21384,1.);
#6079=VECTOR('',#21385,1.);
#6080=VECTOR('',#21388,1.);
#6081=VECTOR('',#21389,1.);
#6082=VECTOR('',#21398,1.);
#6083=VECTOR('',#21399,1.);
#6084=VECTOR('',#21400,1.);
#6085=VECTOR('',#21401,1.);
#6086=VECTOR('',#21404,1.);
#6087=VECTOR('',#21405,1.);
#6088=VECTOR('',#21406,1.);
#6089=VECTOR('',#21409,1.);
#6090=VECTOR('',#21410,1.);
#6091=VECTOR('',#21411,1.);
#6092=VECTOR('',#21414,1.);
#6093=VECTOR('',#21415,1.);
#6094=VECTOR('',#21424,1.);
#6095=VECTOR('',#21425,1.);
#6096=VECTOR('',#21426,1.);
#6097=VECTOR('',#21427,1.);
#6098=VECTOR('',#21430,1.);
#6099=VECTOR('',#21431,1.);
#6100=VECTOR('',#21432,1.);
#6101=VECTOR('',#21435,1.);
#6102=VECTOR('',#21436,1.);
#6103=VECTOR('',#21437,1.);
#6104=VECTOR('',#21440,1.);
#6105=VECTOR('',#21441,1.);
#6106=VECTOR('',#21452,0.275);
#6107=VECTOR('',#21459,0.275);
#6108=VECTOR('',#21466,0.275);
#6109=VECTOR('',#21473,0.275);
#6110=VECTOR('',#21480,0.275);
#6111=VECTOR('',#21487,0.275);
#6112=VECTOR('',#21494,0.275);
#6113=VECTOR('',#21501,0.275);
#6114=VECTOR('',#21506,1.);
#6115=VECTOR('',#21507,1.);
#6116=VECTOR('',#21508,1.);
#6117=VECTOR('',#21509,1.);
#6118=VECTOR('',#21512,1.);
#6119=VECTOR('',#21513,1.);
#6120=VECTOR('',#21514,1.);
#6121=VECTOR('',#21517,1.);
#6122=VECTOR('',#21518,1.);
#6123=VECTOR('',#21519,1.);
#6124=VECTOR('',#21522,1.);
#6125=VECTOR('',#21523,1.);
#6126=VECTOR('',#21528,0.61);
#6127=VECTOR('',#21535,0.61);
#6128=VECTOR('',#21540,1.);
#6129=VECTOR('',#21541,1.);
#6130=VECTOR('',#21542,1.);
#6131=VECTOR('',#21543,1.);
#6132=VECTOR('',#21546,1.);
#6133=VECTOR('',#21547,1.);
#6134=VECTOR('',#21548,1.);
#6135=VECTOR('',#21551,1.);
#6136=VECTOR('',#21552,1.);
#6137=VECTOR('',#21553,1.);
#6138=VECTOR('',#21556,1.);
#6139=VECTOR('',#21557,1.);
#6140=VECTOR('',#21568,0.274999999999999);
#6141=VECTOR('',#21575,0.274999999999999);
#6142=VECTOR('',#21582,0.21);
#6143=VECTOR('',#21591,0.21);
#6144=VECTOR('',#21600,0.21);
#6145=VECTOR('',#21609,0.21);
#6146=VECTOR('',#21616,1.);
#6147=VECTOR('',#21617,1.);
#6148=VECTOR('',#21618,1.);
#6149=VECTOR('',#21619,1.);
#6150=VECTOR('',#21622,1.);
#6151=VECTOR('',#21623,1.);
#6152=VECTOR('',#21624,1.);
#6153=VECTOR('',#21627,1.);
#6154=VECTOR('',#21628,1.);
#6155=VECTOR('',#21629,1.);
#6156=VECTOR('',#21632,1.);
#6157=VECTOR('',#21633,1.);
#6158=VECTOR('',#21644,0.274999999999999);
#6159=VECTOR('',#21651,0.274999999999999);
#6160=VECTOR('',#21658,0.21);
#6161=VECTOR('',#21667,0.21);
#6162=VECTOR('',#21676,0.21);
#6163=VECTOR('',#21685,0.21);
#6164=VECTOR('',#21692,1.);
#6165=VECTOR('',#21693,1.);
#6166=VECTOR('',#21694,1.);
#6167=VECTOR('',#21695,1.);
#6168=VECTOR('',#21698,1.);
#6169=VECTOR('',#21699,1.);
#6170=VECTOR('',#21700,1.);
#6171=VECTOR('',#21703,1.);
#6172=VECTOR('',#21704,1.);
#6173=VECTOR('',#21705,1.);
#6174=VECTOR('',#21708,1.);
#6175=VECTOR('',#21709,1.);
#6176=VECTOR('',#21720,0.21);
#6177=VECTOR('',#21729,0.21);
#6178=VECTOR('',#21738,0.21);
#6179=VECTOR('',#21745,0.21);
#6180=VECTOR('',#21750,1.);
#6181=VECTOR('',#21751,1.);
#6182=VECTOR('',#21752,1.);
#6183=VECTOR('',#21753,1.);
#6184=VECTOR('',#21756,1.);
#6185=VECTOR('',#21757,1.);
#6186=VECTOR('',#21758,1.);
#6187=VECTOR('',#21761,1.);
#6188=VECTOR('',#21762,1.);
#6189=VECTOR('',#21763,1.);
#6190=VECTOR('',#21766,1.);
#6191=VECTOR('',#21767,1.);
#6192=VECTOR('',#21778,0.21);
#6193=VECTOR('',#21785,0.21);
#6194=VECTOR('',#21792,0.21);
#6195=VECTOR('',#21795,1.);
#6196=VECTOR('',#21798,1.);
#6197=VECTOR('',#21803,1.);
#6198=VECTOR('',#21808,0.21);
#6199=VECTOR('',#21811,1.);
#6200=VECTOR('',#21814,1.);
#6201=VECTOR('',#21819,1.);
#6202=VECTOR('',#21822,1.);
#6203=VECTOR('',#21823,1.);
#6204=VECTOR('',#21824,1.);
#6205=VECTOR('',#21825,1.);
#6206=VECTOR('',#21826,1.);
#6207=VECTOR('',#21827,1.);
#6208=VECTOR('',#21830,1.);
#6209=VECTOR('',#21831,1.);
#6210=VECTOR('',#21832,1.);
#6211=VECTOR('',#21835,1.);
#6212=VECTOR('',#21836,1.);
#6213=VECTOR('',#21837,1.);
#6214=VECTOR('',#21840,1.);
#6215=VECTOR('',#21841,1.);
#6216=VECTOR('',#21842,1.);
#6217=VECTOR('',#21845,1.);
#6218=VECTOR('',#21846,1.);
#6219=VECTOR('',#21847,1.);
#6220=VECTOR('',#21850,1.);
#6221=VECTOR('',#21851,1.);
#6222=VECTOR('',#21862,0.21);
#6223=VECTOR('',#21871,0.21);
#6224=VECTOR('',#21880,0.21);
#6225=VECTOR('',#21887,0.21);
#6226=VECTOR('',#21892,1.);
#6227=VECTOR('',#21893,1.);
#6228=VECTOR('',#21894,1.);
#6229=VECTOR('',#21895,1.);
#6230=VECTOR('',#21898,1.);
#6231=VECTOR('',#21899,1.);
#6232=VECTOR('',#21900,1.);
#6233=VECTOR('',#21903,1.);
#6234=VECTOR('',#21904,1.);
#6235=VECTOR('',#21905,1.);
#6236=VECTOR('',#21908,1.);
#6237=VECTOR('',#21909,1.);
#6238=VECTOR('',#21920,0.21);
#6239=VECTOR('',#21927,0.21);
#6240=VECTOR('',#21934,0.21);
#6241=VECTOR('',#21937,1.);
#6242=VECTOR('',#21940,1.);
#6243=VECTOR('',#21945,1.);
#6244=VECTOR('',#21950,0.21);
#6245=VECTOR('',#21953,1.);
#6246=VECTOR('',#21956,1.);
#6247=VECTOR('',#21961,1.);
#6248=VECTOR('',#21964,1.);
#6249=VECTOR('',#21965,1.);
#6250=VECTOR('',#21966,1.);
#6251=VECTOR('',#21967,1.);
#6252=VECTOR('',#21968,1.);
#6253=VECTOR('',#21969,1.);
#6254=VECTOR('',#21972,1.);
#6255=VECTOR('',#21973,1.);
#6256=VECTOR('',#21974,1.);
#6257=VECTOR('',#21977,1.);
#6258=VECTOR('',#21978,1.);
#6259=VECTOR('',#21979,1.);
#6260=VECTOR('',#21982,1.);
#6261=VECTOR('',#21983,1.);
#6262=VECTOR('',#21984,1.);
#6263=VECTOR('',#21987,1.);
#6264=VECTOR('',#21988,1.);
#6265=VECTOR('',#21989,1.);
#6266=VECTOR('',#21992,1.);
#6267=VECTOR('',#21993,1.);
#6268=VECTOR('',#22004,0.165);
#6269=VECTOR('',#22011,0.165);
#6270=VECTOR('',#22018,0.165);
#6271=VECTOR('',#22025,0.21);
#6272=VECTOR('',#22034,0.21);
#6273=VECTOR('',#22043,0.21);
#6274=VECTOR('',#22052,0.21);
#6275=VECTOR('',#22061,1.6);
#6276=VECTOR('',#22070,1.4);
#6277=VECTOR('',#22077,2.5);
#6278=VECTOR('',#22084,1.);
#6279=VECTOR('',#22085,1.);
#6280=VECTOR('',#22086,1.);
#6281=VECTOR('',#22087,1.);
#6282=VECTOR('',#22090,1.);
#6283=VECTOR('',#22091,1.);
#6284=VECTOR('',#22092,1.);
#6285=VECTOR('',#22095,1.);
#6286=VECTOR('',#22096,1.);
#6287=VECTOR('',#22097,1.);
#6288=VECTOR('',#22100,1.);
#6289=VECTOR('',#22101,1.);
#6290=VECTOR('',#22112,0.275);
#6291=VECTOR('',#22119,0.275);
#6292=VECTOR('',#22126,0.165);
#6293=VECTOR('',#22133,0.165);
#6294=VECTOR('',#22140,0.165);
#6295=VECTOR('',#22147,0.210000000000001);
#6296=VECTOR('',#22156,0.210000000000001);
#6297=VECTOR('',#22165,0.210000000000001);
#6298=VECTOR('',#22174,0.210000000000001);
#6299=VECTOR('',#22183,2.35);
#6300=VECTOR('',#22194,2.15);
#6301=VECTOR('',#22197,1.);
#6302=VECTOR('',#22200,1.);
#6303=VECTOR('',#22205,1.);
#6304=VECTOR('',#22208,1.);
#6305=VECTOR('',#22213,1.);
#6306=VECTOR('',#22214,1.);
#6307=VECTOR('',#22215,1.);
#6308=VECTOR('',#22218,1.);
#6309=VECTOR('',#22219,1.);
#6310=VECTOR('',#22220,1.);
#6311=VECTOR('',#22223,1.);
#6312=VECTOR('',#22226,1.);
#6313=VECTOR('',#22227,1.);
#6314=VECTOR('',#22230,1.);
#6315=VECTOR('',#22239,0.225);
#6316=VECTOR('',#22246,0.225);
#6317=VECTOR('',#22253,0.225);
#6318=VECTOR('',#22260,1.59);
#6319=VECTOR('',#22269,1.2);
#6320=VECTOR('',#22276,2.4);
#6321=VECTOR('',#22289,0.225);
#6322=VECTOR('',#22296,0.225);
#6323=VECTOR('',#22303,0.225);
#6324=VECTOR('',#22310,2.34);
#6325=VECTOR('',#22321,1.8);
#6326=VECTOR('',#22326,3.);
#6327=VECTOR('',#22339,0.21);
#6328=VECTOR('',#22348,0.5);
#6329=VECTOR('',#22361,0.21);
#6330=VECTOR('',#22370,0.5);
#6331=VECTOR('',#22383,0.21);
#6332=VECTOR('',#22392,0.5);
#6333=VECTOR('',#22405,0.21);
#6334=VECTOR('',#22414,0.5);
#6335=VECTOR('',#22427,0.375);
#6336=VECTOR('',#22438,0.375);
#6337=VECTOR('',#22449,0.375);
#6338=VECTOR('',#22460,0.375);
#6339=VECTOR('',#22471,0.225);
#6340=VECTOR('',#22476,0.225);
#6341=VECTOR('',#22481,0.225);
#6342=VECTOR('',#22486,0.225);
#6343=VECTOR('',#22491,3.);
#6344=VECTOR('',#22502,1.);
#6345=VECTOR('',#22503,1.);
#6346=VECTOR('',#22504,1.);
#6347=VECTOR('',#22505,1.);
#6348=VECTOR('',#22508,1.);
#6349=VECTOR('',#22509,1.);
#6350=VECTOR('',#22510,1.);
#6351=VECTOR('',#22513,1.);
#6352=VECTOR('',#22514,1.);
#6353=VECTOR('',#22515,1.);
#6354=VECTOR('',#22518,1.);
#6355=VECTOR('',#22519,1.);
#6356=VECTOR('',#22524,1.);
#6357=VECTOR('',#22525,1.);
#6358=VECTOR('',#22526,1.);
#6359=VECTOR('',#22527,1.);
#6360=VECTOR('',#22530,1.);
#6361=VECTOR('',#22531,1.);
#6362=VECTOR('',#22532,1.);
#6363=VECTOR('',#22535,1.);
#6364=VECTOR('',#22536,1.);
#6365=VECTOR('',#22537,1.);
#6366=VECTOR('',#22540,1.);
#6367=VECTOR('',#22541,1.);
#6368=VECTOR('',#22546,1.);
#6369=VECTOR('',#22547,1.);
#6370=VECTOR('',#22548,1.);
#6371=VECTOR('',#22549,1.);
#6372=VECTOR('',#22552,1.);
#6373=VECTOR('',#22553,1.);
#6374=VECTOR('',#22554,1.);
#6375=VECTOR('',#22557,1.);
#6376=VECTOR('',#22558,1.);
#6377=VECTOR('',#22559,1.);
#6378=VECTOR('',#22562,1.);
#6379=VECTOR('',#22563,1.);
#6380=VECTOR('',#22568,1.);
#6381=VECTOR('',#22569,1.);
#6382=VECTOR('',#22570,1.);
#6383=VECTOR('',#22571,1.);
#6384=VECTOR('',#22574,1.);
#6385=VECTOR('',#22575,1.);
#6386=VECTOR('',#22576,1.);
#6387=VECTOR('',#22579,1.);
#6388=VECTOR('',#22580,1.);
#6389=VECTOR('',#22581,1.);
#6390=VECTOR('',#22584,1.);
#6391=VECTOR('',#22585,1.);
#6392=VECTOR('',#22590,1.);
#6393=VECTOR('',#22591,1.);
#6394=VECTOR('',#22592,1.);
#6395=VECTOR('',#22593,1.);
#6396=VECTOR('',#22596,1.);
#6397=VECTOR('',#22597,1.);
#6398=VECTOR('',#22598,1.);
#6399=VECTOR('',#22601,1.);
#6400=VECTOR('',#22602,1.);
#6401=VECTOR('',#22603,1.);
#6402=VECTOR('',#22606,1.);
#6403=VECTOR('',#22607,1.);
#6404=VECTOR('',#22612,1.);
#6405=VECTOR('',#22613,1.);
#6406=VECTOR('',#22614,1.);
#6407=VECTOR('',#22615,1.);
#6408=VECTOR('',#22618,1.);
#6409=VECTOR('',#22619,1.);
#6410=VECTOR('',#22620,1.);
#6411=VECTOR('',#22623,1.);
#6412=VECTOR('',#22624,1.);
#6413=VECTOR('',#22625,1.);
#6414=VECTOR('',#22628,1.);
#6415=VECTOR('',#22629,1.);
#6416=VECTOR('',#22634,1.);
#6417=VECTOR('',#22635,1.);
#6418=VECTOR('',#22636,1.);
#6419=VECTOR('',#22637,1.);
#6420=VECTOR('',#22640,1.);
#6421=VECTOR('',#22641,1.);
#6422=VECTOR('',#22642,1.);
#6423=VECTOR('',#22645,1.);
#6424=VECTOR('',#22646,1.);
#6425=VECTOR('',#22647,1.);
#6426=VECTOR('',#22650,1.);
#6427=VECTOR('',#22651,1.);
#6428=VECTOR('',#22656,1.);
#6429=VECTOR('',#22657,1.);
#6430=VECTOR('',#22658,1.);
#6431=VECTOR('',#22659,1.);
#6432=VECTOR('',#22662,1.);
#6433=VECTOR('',#22663,1.);
#6434=VECTOR('',#22664,1.);
#6435=VECTOR('',#22667,1.);
#6436=VECTOR('',#22668,1.);
#6437=VECTOR('',#22669,1.);
#6438=VECTOR('',#22672,1.);
#6439=VECTOR('',#22673,1.);
#6440=VECTOR('',#22678,1.);
#6441=VECTOR('',#22679,1.);
#6442=VECTOR('',#22680,1.);
#6443=VECTOR('',#22681,1.);
#6444=VECTOR('',#22684,1.);
#6445=VECTOR('',#22685,1.);
#6446=VECTOR('',#22686,1.);
#6447=VECTOR('',#22689,1.);
#6448=VECTOR('',#22690,1.);
#6449=VECTOR('',#22691,1.);
#6450=VECTOR('',#22694,1.);
#6451=VECTOR('',#22695,1.);
#6452=VECTOR('',#22700,1.);
#6453=VECTOR('',#22701,1.);
#6454=VECTOR('',#22702,1.);
#6455=VECTOR('',#22703,1.);
#6456=VECTOR('',#22706,1.);
#6457=VECTOR('',#22707,1.);
#6458=VECTOR('',#22708,1.);
#6459=VECTOR('',#22711,1.);
#6460=VECTOR('',#22712,1.);
#6461=VECTOR('',#22713,1.);
#6462=VECTOR('',#22716,1.);
#6463=VECTOR('',#22717,1.);
#6464=VECTOR('',#22722,1.);
#6465=VECTOR('',#22723,1.);
#6466=VECTOR('',#22724,1.);
#6467=VECTOR('',#22725,1.);
#6468=VECTOR('',#22728,1.);
#6469=VECTOR('',#22729,1.);
#6470=VECTOR('',#22730,1.);
#6471=VECTOR('',#22733,1.);
#6472=VECTOR('',#22734,1.);
#6473=VECTOR('',#22735,1.);
#6474=VECTOR('',#22738,1.);
#6475=VECTOR('',#22739,1.);
#6476=VECTOR('',#22744,1.);
#6477=VECTOR('',#22745,1.);
#6478=VECTOR('',#22746,1.);
#6479=VECTOR('',#22747,1.);
#6480=VECTOR('',#22750,1.);
#6481=VECTOR('',#22751,1.);
#6482=VECTOR('',#22752,1.);
#6483=VECTOR('',#22755,1.);
#6484=VECTOR('',#22756,1.);
#6485=VECTOR('',#22757,1.);
#6486=VECTOR('',#22760,1.);
#6487=VECTOR('',#22761,1.);
#6488=VECTOR('',#22766,1.);
#6489=VECTOR('',#22767,1.);
#6490=VECTOR('',#22768,1.);
#6491=VECTOR('',#22769,1.);
#6492=VECTOR('',#22772,1.);
#6493=VECTOR('',#22773,1.);
#6494=VECTOR('',#22774,1.);
#6495=VECTOR('',#22777,1.);
#6496=VECTOR('',#22778,1.);
#6497=VECTOR('',#22779,1.);
#6498=VECTOR('',#22782,1.);
#6499=VECTOR('',#22783,1.);
#6500=VECTOR('',#22788,1.);
#6501=VECTOR('',#22789,1.);
#6502=VECTOR('',#22790,1.);
#6503=VECTOR('',#22791,1.);
#6504=VECTOR('',#22794,1.);
#6505=VECTOR('',#22795,1.);
#6506=VECTOR('',#22796,1.);
#6507=VECTOR('',#22799,1.);
#6508=VECTOR('',#22800,1.);
#6509=VECTOR('',#22801,1.);
#6510=VECTOR('',#22804,1.);
#6511=VECTOR('',#22805,1.);
#6512=VECTOR('',#22810,1.);
#6513=VECTOR('',#22811,1.);
#6514=VECTOR('',#22812,1.);
#6515=VECTOR('',#22813,1.);
#6516=VECTOR('',#22816,1.);
#6517=VECTOR('',#22817,1.);
#6518=VECTOR('',#22818,1.);
#6519=VECTOR('',#22821,1.);
#6520=VECTOR('',#22822,1.);
#6521=VECTOR('',#22823,1.);
#6522=VECTOR('',#22826,1.);
#6523=VECTOR('',#22827,1.);
#6524=VECTOR('',#22832,1.);
#6525=VECTOR('',#22833,1.);
#6526=VECTOR('',#22834,1.);
#6527=VECTOR('',#22835,1.);
#6528=VECTOR('',#22838,1.);
#6529=VECTOR('',#22839,1.);
#6530=VECTOR('',#22840,1.);
#6531=VECTOR('',#22843,1.);
#6532=VECTOR('',#22844,1.);
#6533=VECTOR('',#22845,1.);
#6534=VECTOR('',#22848,1.);
#6535=VECTOR('',#22849,1.);
#6536=VECTOR('',#22854,1.);
#6537=VECTOR('',#22855,1.);
#6538=VECTOR('',#22856,1.);
#6539=VECTOR('',#22857,1.);
#6540=VECTOR('',#22860,1.);
#6541=VECTOR('',#22861,1.);
#6542=VECTOR('',#22862,1.);
#6543=VECTOR('',#22865,1.);
#6544=VECTOR('',#22866,1.);
#6545=VECTOR('',#22867,1.);
#6546=VECTOR('',#22870,1.);
#6547=VECTOR('',#22871,1.);
#6548=VECTOR('',#22876,1.);
#6549=VECTOR('',#22877,1.);
#6550=VECTOR('',#22878,1.);
#6551=VECTOR('',#22879,1.);
#6552=VECTOR('',#22882,1.);
#6553=VECTOR('',#22883,1.);
#6554=VECTOR('',#22884,1.);
#6555=VECTOR('',#22887,1.);
#6556=VECTOR('',#22888,1.);
#6557=VECTOR('',#22889,1.);
#6558=VECTOR('',#22892,1.);
#6559=VECTOR('',#22893,1.);
#6560=VECTOR('',#22898,1.);
#6561=VECTOR('',#22899,1.);
#6562=VECTOR('',#22900,1.);
#6563=VECTOR('',#22901,1.);
#6564=VECTOR('',#22904,1.);
#6565=VECTOR('',#22905,1.);
#6566=VECTOR('',#22906,1.);
#6567=VECTOR('',#22909,1.);
#6568=VECTOR('',#22910,1.);
#6569=VECTOR('',#22911,1.);
#6570=VECTOR('',#22914,1.);
#6571=VECTOR('',#22915,1.);
#6572=VECTOR('',#22920,1.);
#6573=VECTOR('',#22921,1.);
#6574=VECTOR('',#22922,1.);
#6575=VECTOR('',#22923,1.);
#6576=VECTOR('',#22926,1.);
#6577=VECTOR('',#22927,1.);
#6578=VECTOR('',#22928,1.);
#6579=VECTOR('',#22931,1.);
#6580=VECTOR('',#22932,1.);
#6581=VECTOR('',#22933,1.);
#6582=VECTOR('',#22936,1.);
#6583=VECTOR('',#22937,1.);
#6584=VECTOR('',#22942,1.);
#6585=VECTOR('',#22943,1.);
#6586=VECTOR('',#22944,1.);
#6587=VECTOR('',#22945,1.);
#6588=VECTOR('',#22948,1.);
#6589=VECTOR('',#22949,1.);
#6590=VECTOR('',#22950,1.);
#6591=VECTOR('',#22953,1.);
#6592=VECTOR('',#22954,1.);
#6593=VECTOR('',#22955,1.);
#6594=VECTOR('',#22958,1.);
#6595=VECTOR('',#22959,1.);
#6596=VECTOR('',#22964,1.);
#6597=VECTOR('',#22965,1.);
#6598=VECTOR('',#22966,1.);
#6599=VECTOR('',#22967,1.);
#6600=VECTOR('',#22970,1.);
#6601=VECTOR('',#22971,1.);
#6602=VECTOR('',#22972,1.);
#6603=VECTOR('',#22975,1.);
#6604=VECTOR('',#22976,1.);
#6605=VECTOR('',#22977,1.);
#6606=VECTOR('',#22980,1.);
#6607=VECTOR('',#22981,1.);
#6608=VECTOR('',#22986,1.);
#6609=VECTOR('',#22987,1.);
#6610=VECTOR('',#22988,1.);
#6611=VECTOR('',#22989,1.);
#6612=VECTOR('',#22992,1.);
#6613=VECTOR('',#22993,1.);
#6614=VECTOR('',#22994,1.);
#6615=VECTOR('',#22997,1.);
#6616=VECTOR('',#22998,1.);
#6617=VECTOR('',#22999,1.);
#6618=VECTOR('',#23002,1.);
#6619=VECTOR('',#23003,1.);
#6620=VECTOR('',#23008,1.);
#6621=VECTOR('',#23009,1.);
#6622=VECTOR('',#23010,1.);
#6623=VECTOR('',#23011,1.);
#6624=VECTOR('',#23014,1.);
#6625=VECTOR('',#23015,1.);
#6626=VECTOR('',#23016,1.);
#6627=VECTOR('',#23019,1.);
#6628=VECTOR('',#23020,1.);
#6629=VECTOR('',#23021,1.);
#6630=VECTOR('',#23024,1.);
#6631=VECTOR('',#23025,1.);
#6632=VECTOR('',#23030,1.);
#6633=VECTOR('',#23031,1.);
#6634=VECTOR('',#23032,1.);
#6635=VECTOR('',#23033,1.);
#6636=VECTOR('',#23036,1.);
#6637=VECTOR('',#23037,1.);
#6638=VECTOR('',#23038,1.);
#6639=VECTOR('',#23041,1.);
#6640=VECTOR('',#23042,1.);
#6641=VECTOR('',#23043,1.);
#6642=VECTOR('',#23046,1.);
#6643=VECTOR('',#23047,1.);
#6644=VECTOR('',#23054,0.274999999999999);
#6645=VECTOR('',#23061,0.275);
#6646=VECTOR('',#23066,1.);
#6647=VECTOR('',#23067,1.);
#6648=VECTOR('',#23068,1.);
#6649=VECTOR('',#23069,1.);
#6650=VECTOR('',#23072,1.);
#6651=VECTOR('',#23073,1.);
#6652=VECTOR('',#23074,1.);
#6653=VECTOR('',#23077,1.);
#6654=VECTOR('',#23078,1.);
#6655=VECTOR('',#23079,1.);
#6656=VECTOR('',#23082,1.);
#6657=VECTOR('',#23083,1.);
#6658=VECTOR('',#23094,0.55);
#6659=VECTOR('',#23101,0.6);
#6660=VECTOR('',#23108,0.55);
#6661=VECTOR('',#23115,1.);
#6662=VECTOR('',#23120,1.);
#6663=VECTOR('',#23123,1.);
#6664=VECTOR('',#23126,1.);
#6665=VECTOR('',#23129,1.);
#6666=VECTOR('',#23134,1.);
#6667=VECTOR('',#23137,1.);
#6668=VECTOR('',#23138,1.);
#6669=VECTOR('',#23139,1.);
#6670=VECTOR('',#23140,1.);
#6671=VECTOR('',#23141,1.);
#6672=VECTOR('',#23146,1.);
#6673=VECTOR('',#23147,1.);
#6674=VECTOR('',#23148,1.);
#6675=VECTOR('',#23153,1.);
#6676=VECTOR('',#23154,1.);
#6677=VECTOR('',#23155,1.);
#6678=VECTOR('',#23156,1.);
#6679=VECTOR('',#23157,1.);
#6680=VECTOR('',#23164,0.225);
#6681=VECTOR('',#23169,0.165);
#6682=VECTOR('',#23176,0.275);
#6683=VECTOR('',#23181,0.275);
#6684=VECTOR('',#23186,0.6);
#6685=VECTOR('',#23191,1.);
#6686=VECTOR('',#23192,1.);
#6687=VECTOR('',#23193,1.);
#6688=VECTOR('',#23194,1.);
#6689=VECTOR('',#23195,1.);
#6690=VECTOR('',#23196,1.);
#6691=VECTOR('',#23197,1.);
#6692=VECTOR('',#23198,1.);
#6693=VECTOR('',#23199,1.);
#6694=VECTOR('',#23202,1.);
#6695=VECTOR('',#23203,1.);
#6696=VECTOR('',#23206,1.);
#6697=VECTOR('',#23207,1.);
#6698=VECTOR('',#23210,1.);
#6699=VECTOR('',#23213,1.);
#6700=VECTOR('',#23214,1.);
#6701=VECTOR('',#23217,1.);
#6702=VECTOR('',#23218,1.);
#6703=VECTOR('',#23221,1.);
#6704=VECTOR('',#23222,1.);
#6705=VECTOR('',#23225,1.);
#6706=VECTOR('',#23226,1.);
#6707=VECTOR('',#23229,1.);
#6708=VECTOR('',#23230,1.);
#6709=VECTOR('',#23233,1.);
#6710=VECTOR('',#23240,1.);
#6711=VECTOR('',#23241,1.);
#6712=VECTOR('',#23242,1.);
#6713=VECTOR('',#23243,1.);
#6714=VECTOR('',#23246,1.);
#6715=VECTOR('',#23247,1.);
#6716=VECTOR('',#23248,1.);
#6717=VECTOR('',#23251,1.);
#6718=VECTOR('',#23252,1.);
#6719=VECTOR('',#23253,1.);
#6720=VECTOR('',#23256,1.);
#6721=VECTOR('',#23257,1.);
#6722=VECTOR('',#23258,1.);
#6723=VECTOR('',#23261,1.);
#6724=VECTOR('',#23262,1.);
#6725=VECTOR('',#23263,1.);
#6726=VECTOR('',#23266,1.);
#6727=VECTOR('',#23267,1.);
#6728=VECTOR('',#23284,0.4);
#6729=VECTOR('',#23289,0.425);
#6730=VECTOR('',#23294,0.41);
#6731=VECTOR('',#23303,0.26);
#6732=VECTOR('',#23306,0.25);
#6733=VECTOR('',#23325,1.070235);
#6734=VECTOR('',#23332,0.6);
#6735=VECTOR('',#23337,0.63);
#6736=VECTOR('',#23346,1.070235);
#6737=VECTOR('',#23353,0.63);
#6738=VECTOR('',#23372,1.129765);
#6739=VECTOR('',#23383,1.57);
#6740=VECTOR('',#23388,1.6);
#6741=VECTOR('',#23393,1.57);
#6742=VECTOR('',#23398,1.129765);
#6743=VECTOR('',#23445,1.123812);
#6744=VECTOR('',#23514,1.076188);
#6745=VECTOR('',#23543,1.119765);
#6746=VECTOR('',#23550,1.085235);
#6747=VECTOR('',#23561,1.119765);
#6748=VECTOR('',#23568,1.085235);
#6749=VECTOR('',#23597,1.63531);
#6750=VECTOR('',#23604,1.);
#6751=VECTOR('',#23609,1.05);
#6752=VECTOR('',#23618,1.63531);
#6753=VECTOR('',#23625,1.05);
#6754=VECTOR('',#23644,1.71469);
#6755=VECTOR('',#23655,2.3);
#6756=VECTOR('',#23660,2.35);
#6757=VECTOR('',#23665,2.3);
#6758=VECTOR('',#23670,1.71469);
#6759=VECTOR('',#23721,1.706752);
#6760=VECTOR('',#23798,1.643248);
#6761=VECTOR('',#23827,1.70469);
#6762=VECTOR('',#23834,1.65031);
#6763=VECTOR('',#23845,1.70469);
#6764=VECTOR('',#23852,1.65031);
#6765=VECTOR('',#23877,0.25);
#6766=VECTOR('',#23886,0.4);
#6767=VECTOR('',#23891,0.425);
#6768=VECTOR('',#23896,0.41);
#6769=VECTOR('',#23905,0.26);
#6770=VECTOR('',#23908,0.25);
#6771=VECTOR('',#23911,1.);
#6772=VECTOR('',#23912,1.);
#6773=VECTOR('',#23913,1.);
#6774=VECTOR('',#23914,1.);
#6775=VECTOR('',#23917,1.);
#6776=VECTOR('',#23918,1.);
#6777=VECTOR('',#23919,1.);
#6778=VECTOR('',#23922,1.);
#6779=VECTOR('',#23923,1.);
#6780=VECTOR('',#23924,1.);
#6781=VECTOR('',#23927,1.);
#6782=VECTOR('',#23928,1.);
#6783=VECTOR('',#23929,1.);
#6784=VECTOR('',#23932,1.);
#6785=VECTOR('',#23933,1.);
#6786=VECTOR('',#23934,1.);
#6787=VECTOR('',#23937,1.);
#6788=VECTOR('',#23938,1.);
#6789=VECTOR('',#23947,1.);
#6790=VECTOR('',#23948,1.);
#6791=VECTOR('',#23949,1.);
#6792=VECTOR('',#23950,1.);
#6793=VECTOR('',#23953,1.);
#6794=VECTOR('',#23954,1.);
#6795=VECTOR('',#23955,1.);
#6796=VECTOR('',#23958,1.);
#6797=VECTOR('',#23959,1.);
#6798=VECTOR('',#23960,1.);
#6799=VECTOR('',#23963,1.);
#6800=VECTOR('',#23964,1.);
#6801=VECTOR('',#23965,1.);
#6802=VECTOR('',#23968,1.);
#6803=VECTOR('',#23969,1.);
#6804=VECTOR('',#23970,1.);
#6805=VECTOR('',#23973,1.);
#6806=VECTOR('',#23974,1.);
#6807=VECTOR('',#23991,0.325);
#6808=VECTOR('',#23996,0.35);
#6809=VECTOR('',#24001,0.335);
#6810=VECTOR('',#24010,0.21);
#6811=VECTOR('',#24013,0.2);
#6812=VECTOR('',#24018,1.);
#6813=VECTOR('',#24019,1.);
#6814=VECTOR('',#24020,1.);
#6815=VECTOR('',#24021,1.);
#6816=VECTOR('',#24024,1.);
#6817=VECTOR('',#24025,1.);
#6818=VECTOR('',#24026,1.);
#6819=VECTOR('',#24029,1.);
#6820=VECTOR('',#24030,1.);
#6821=VECTOR('',#24031,1.);
#6822=VECTOR('',#24034,1.);
#6823=VECTOR('',#24035,1.);
#6824=VECTOR('',#24036,1.);
#6825=VECTOR('',#24039,1.);
#6826=VECTOR('',#24040,1.);
#6827=VECTOR('',#24041,1.);
#6828=VECTOR('',#24044,1.);
#6829=VECTOR('',#24045,1.);
#6830=VECTOR('',#24046,1.);
#6831=VECTOR('',#24049,1.);
#6832=VECTOR('',#24050,1.);
#6833=VECTOR('',#24051,1.);
#6834=VECTOR('',#24054,1.);
#6835=VECTOR('',#24055,1.);
#6836=VECTOR('',#24056,1.);
#6837=VECTOR('',#24059,1.);
#6838=VECTOR('',#24060,1.);
#6839=VECTOR('',#24061,1.);
#6840=VECTOR('',#24064,1.);
#6841=VECTOR('',#24065,1.);
#6842=VECTOR('',#24066,1.);
#6843=VECTOR('',#24067,1.);
#6844=VECTOR('',#24070,1.);
#6845=VECTOR('',#24071,1.);
#6846=VECTOR('',#24072,1.);
#6847=VECTOR('',#24075,1.);
#6848=VECTOR('',#24076,1.);
#6849=VECTOR('',#24077,1.);
#6850=VECTOR('',#24080,1.);
#6851=VECTOR('',#24081,1.);
#6852=VECTOR('',#24082,1.);
#6853=VECTOR('',#24085,1.);
#6854=VECTOR('',#24086,1.);
#6855=VECTOR('',#24087,1.);
#6856=VECTOR('',#24090,1.);
#6857=VECTOR('',#24091,1.);
#6858=VECTOR('',#24092,1.);
#6859=VECTOR('',#24095,1.);
#6860=VECTOR('',#24096,1.);
#6861=VECTOR('',#24097,1.);
#6862=VECTOR('',#24100,1.);
#6863=VECTOR('',#24101,1.);
#6864=VECTOR('',#24102,1.);
#6865=VECTOR('',#24105,1.);
#6866=VECTOR('',#24106,1.);
#6867=VECTOR('',#24107,1.);
#6868=VECTOR('',#24110,1.);
#6869=VECTOR('',#24111,1.);
#6870=VECTOR('',#24112,1.);
#6871=VECTOR('',#24113,1.);
#6872=VECTOR('',#24116,1.);
#6873=VECTOR('',#24117,1.);
#6874=VECTOR('',#24118,1.);
#6875=VECTOR('',#24121,1.);
#6876=VECTOR('',#24122,1.);
#6877=VECTOR('',#24123,1.);
#6878=VECTOR('',#24126,1.);
#6879=VECTOR('',#24127,1.);
#6880=VECTOR('',#24128,1.);
#6881=VECTOR('',#24131,1.);
#6882=VECTOR('',#24132,1.);
#6883=VECTOR('',#24133,1.);
#6884=VECTOR('',#24136,1.);
#6885=VECTOR('',#24137,1.);
#6886=VECTOR('',#24138,1.);
#6887=VECTOR('',#24141,1.);
#6888=VECTOR('',#24142,1.);
#6889=VECTOR('',#24143,1.);
#6890=VECTOR('',#24146,1.);
#6891=VECTOR('',#24147,1.);
#6892=VECTOR('',#24148,1.);
#6893=VECTOR('',#24151,1.);
#6894=VECTOR('',#24152,1.);
#6895=VECTOR('',#24153,1.);
#6896=VECTOR('',#24156,1.);
#6897=VECTOR('',#24157,1.);
#6898=VECTOR('',#24158,1.);
#6899=VECTOR('',#24159,1.);
#6900=VECTOR('',#24162,1.);
#6901=VECTOR('',#24163,1.);
#6902=VECTOR('',#24164,1.);
#6903=VECTOR('',#24167,1.);
#6904=VECTOR('',#24168,1.);
#6905=VECTOR('',#24169,1.);
#6906=VECTOR('',#24172,1.);
#6907=VECTOR('',#24173,1.);
#6908=VECTOR('',#24174,1.);
#6909=VECTOR('',#24177,1.);
#6910=VECTOR('',#24178,1.);
#6911=VECTOR('',#24179,1.);
#6912=VECTOR('',#24182,1.);
#6913=VECTOR('',#24183,1.);
#6914=VECTOR('',#24184,1.);
#6915=VECTOR('',#24187,1.);
#6916=VECTOR('',#24188,1.);
#6917=VECTOR('',#24189,1.);
#6918=VECTOR('',#24192,1.);
#6919=VECTOR('',#24193,1.);
#6920=VECTOR('',#24194,1.);
#6921=VECTOR('',#24197,1.);
#6922=VECTOR('',#24198,1.);
#6923=VECTOR('',#24199,1.);
#6924=VECTOR('',#24204,0.21);
#6925=VECTOR('',#24209,1.);
#6926=VECTOR('',#24210,1.);
#6927=VECTOR('',#24211,1.);
#6928=VECTOR('',#24214,1.);
#6929=VECTOR('',#24215,1.);
#6930=VECTOR('',#24216,1.);
#6931=VECTOR('',#24219,1.);
#6932=VECTOR('',#24220,1.);
#6933=VECTOR('',#24223,1.);
#6934=VECTOR('',#24224,1.);
#6935=VECTOR('',#24225,1.);
#6936=VECTOR('',#24228,1.);
#6937=VECTOR('',#24229,1.);
#6938=VECTOR('',#24232,1.);
#6939=VECTOR('',#24233,1.);
#6940=VECTOR('',#24234,1.);
#6941=VECTOR('',#24237,1.);
#6942=VECTOR('',#24238,1.);
#6943=VECTOR('',#24241,1.);
#6944=VECTOR('',#24242,1.);
#6945=VECTOR('',#24257,0.4);
#6946=VECTOR('',#24262,0.425);
#6947=VECTOR('',#24267,0.41);
#6948=VECTOR('',#24276,0.26);
#6949=VECTOR('',#24281,0.25);
#6950=VECTOR('',#24286,0.225);
#6951=VECTOR('',#24291,1.);
#6952=VECTOR('',#24292,1.);
#6953=VECTOR('',#24293,1.);
#6954=VECTOR('',#24294,1.);
#6955=VECTOR('',#24297,1.);
#6956=VECTOR('',#24298,1.);
#6957=VECTOR('',#24299,1.);
#6958=VECTOR('',#24302,1.);
#6959=VECTOR('',#24303,1.);
#6960=VECTOR('',#24304,1.);
#6961=VECTOR('',#24307,1.);
#6962=VECTOR('',#24308,1.);
#6963=VECTOR('',#24309,1.);
#6964=VECTOR('',#24312,1.);
#6965=VECTOR('',#24313,1.);
#6966=VECTOR('',#24314,1.);
#6967=VECTOR('',#24317,1.);
#6968=VECTOR('',#24318,1.);
#6969=VECTOR('',#24327,1.);
#6970=VECTOR('',#24328,1.);
#6971=VECTOR('',#24329,1.);
#6972=VECTOR('',#24330,1.);
#6973=VECTOR('',#24333,1.);
#6974=VECTOR('',#24334,1.);
#6975=VECTOR('',#24335,1.);
#6976=VECTOR('',#24338,1.);
#6977=VECTOR('',#24339,1.);
#6978=VECTOR('',#24340,1.);
#6979=VECTOR('',#24345,1.);
#6980=VECTOR('',#24346,1.);
#6981=VECTOR('',#24347,1.);
#6982=VECTOR('',#24348,1.);
#6983=VECTOR('',#24349,1.);
#6984=VECTOR('',#24350,1.);
#6985=VECTOR('',#24351,1.);
#6986=VECTOR('',#24354,1.);
#6987=VECTOR('',#24355,1.);
#6988=VECTOR('',#24358,1.);
#6989=VECTOR('',#24359,1.);
#6990=VECTOR('',#24362,1.);
#6991=VECTOR('',#24363,1.);
#6992=VECTOR('',#24364,1.);
#6993=VECTOR('',#24365,1.);
#6994=VECTOR('',#24366,1.);
#6995=VECTOR('',#24369,1.);
#6996=VECTOR('',#24372,1.);
#6997=VECTOR('',#24375,1.);
#6998=VECTOR('',#24380,0.21);
#6999=VECTOR('',#24389,1.);
#7000=VECTOR('',#24392,1.);
#7001=VECTOR('',#24395,1.);
#7002=VECTOR('',#24404,1.);
#7003=VECTOR('',#24405,1.);
#7004=VECTOR('',#24406,1.);
#7005=VECTOR('',#24407,1.);
#7006=VECTOR('',#24408,1.);
#7007=VECTOR('',#24409,1.);
#7008=VECTOR('',#24418,0.4);
#7009=VECTOR('',#24423,0.425);
#7010=VECTOR('',#24428,0.41);
#7011=VECTOR('',#24437,0.26);
#7012=VECTOR('',#24440,0.25);
#7013=VECTOR('',#24443,1.);
#7014=VECTOR('',#24444,1.);
#7015=VECTOR('',#24445,1.);
#7016=VECTOR('',#24448,1.);
#7017=VECTOR('',#24449,1.);
#7018=VECTOR('',#24452,1.);
#7019=VECTOR('',#24453,1.);
#7020=VECTOR('',#24456,1.);
#7021=VECTOR('',#24457,1.);
#7022=VECTOR('',#24460,1.);
#7023=VECTOR('',#24461,1.);
#7024=VECTOR('',#24464,1.);
#7025=VECTOR('',#24475,0.165);
#7026=VECTOR('',#24482,0.165);
#7027=VECTOR('',#24489,0.225);
#7028=VECTOR('',#24496,0.225);
#7029=VECTOR('',#24503,0.225);
#7030=VECTOR('',#24510,0.225);
#7031=VECTOR('',#24517,0.225);
#7032=VECTOR('',#24524,0.225);
#7033=VECTOR('',#24531,0.225);
#7034=VECTOR('',#24538,0.225);
#7035=VECTOR('',#24545,0.225);
#7036=VECTOR('',#24552,0.225);
#7037=VECTOR('',#24559,0.225);
#7038=VECTOR('',#24566,0.225);
#7039=VECTOR('',#24573,0.225);
#7040=VECTOR('',#24580,0.625);
#7041=VECTOR('',#24587,0.625);
#7042=VECTOR('',#24594,0.625);
#7043=VECTOR('',#24599,1.);
#7044=VECTOR('',#24600,1.);
#7045=VECTOR('',#24601,1.);
#7046=VECTOR('',#24602,1.);
#7047=VECTOR('',#24605,1.);
#7048=VECTOR('',#24606,1.);
#7049=VECTOR('',#24607,1.);
#7050=VECTOR('',#24610,1.);
#7051=VECTOR('',#24611,1.);
#7052=VECTOR('',#24612,1.);
#7053=VECTOR('',#24615,1.);
#7054=VECTOR('',#24616,1.);
#7055=VECTOR('',#24631,1.);
#7056=VECTOR('',#24634,0.165);
#7057=VECTOR('',#24639,1.);
#7058=VECTOR('',#24648,1.);
#7059=VECTOR('',#24651,0.165);
#7060=VECTOR('',#24656,1.);
#7061=VECTOR('',#24667,1.);
#7062=VECTOR('',#24670,1.);
#7063=VECTOR('',#24671,0.165);
#7064=VECTOR('',#24684,1.);
#7065=VECTOR('',#24687,1.);
#7066=VECTOR('',#24688,0.165);
#7067=VECTOR('',#24695,1.5);
#7068=VECTOR('',#24710,1.05);
#7069=VECTOR('',#24725,2.);
#7070=VECTOR('',#24728,0.625);
#7071=VECTOR('',#24745,1.);
#7072=VECTOR('',#24748,0.165);
#7073=VECTOR('',#24753,1.);
#7074=VECTOR('',#24762,1.);
#7075=VECTOR('',#24765,0.165);
#7076=VECTOR('',#24770,1.);
#7077=VECTOR('',#24781,1.);
#7078=VECTOR('',#24784,1.);
#7079=VECTOR('',#24785,0.165);
#7080=VECTOR('',#24798,1.);
#7081=VECTOR('',#24801,1.);
#7082=VECTOR('',#24802,0.165);
#7083=VECTOR('',#24809,1.5);
#7084=VECTOR('',#24824,1.05);
#7085=VECTOR('',#24839,2.);
#7086=VECTOR('',#24842,0.625);
#7087=VECTOR('',#24855,0.165);
#7088=VECTOR('',#24864,0.165);
#7089=VECTOR('',#24873,0.165);
#7090=VECTOR('',#24882,1.11);
#7091=VECTOR('',#24889,2.2);
#7092=VECTOR('',#24902,0.165);
#7093=VECTOR('',#24909,0.165);
#7094=VECTOR('',#24916,3.);
#7095=VECTOR('',#24929,0.225);
#7096=VECTOR('',#24936,0.225);
#7097=VECTOR('',#24941,1.);
#7098=VECTOR('',#24942,1.);
#7099=VECTOR('',#24943,1.);
#7100=VECTOR('',#24944,1.);
#7101=VECTOR('',#24947,1.);
#7102=VECTOR('',#24948,1.);
#7103=VECTOR('',#24949,1.);
#7104=VECTOR('',#24952,1.);
#7105=VECTOR('',#24955,1.);
#7106=VECTOR('',#24956,1.);
#7107=VECTOR('',#24957,1.);
#7108=VECTOR('',#24958,1.);
#7109=VECTOR('',#24961,1.);
#7110=VECTOR('',#24962,1.);
#7111=VECTOR('',#24963,1.);
#7112=VECTOR('',#24966,1.);
#7113=VECTOR('',#24967,1.);
#7114=VECTOR('',#24968,1.);
#7115=VECTOR('',#24971,1.);
#7116=VECTOR('',#24974,1.);
#7117=VECTOR('',#24975,1.);
#7118=VECTOR('',#24976,1.);
#7119=VECTOR('',#24977,1.);
#7120=VECTOR('',#24978,1.);
#7121=VECTOR('',#24981,1.);
#7122=VECTOR('',#24982,1.);
#7123=VECTOR('',#24983,1.);
#7124=VECTOR('',#24986,1.);
#7125=VECTOR('',#24987,1.);
#7126=VECTOR('',#24988,1.);
#7127=VECTOR('',#24991,1.);
#7128=VECTOR('',#24992,1.);
#7129=VECTOR('',#24993,1.);
#7130=VECTOR('',#25006,1.);
#7131=VECTOR('',#25007,1.);
#7132=VECTOR('',#25008,1.);
#7133=VECTOR('',#25011,1.);
#7134=VECTOR('',#25012,1.);
#7135=VECTOR('',#25013,1.);
#7136=VECTOR('',#25018,1.);
#7137=VECTOR('',#25019,1.);
#7138=VECTOR('',#25022,1.);
#7139=VECTOR('',#25023,1.);
#7140=VECTOR('',#25036,1.05);
#7141=VECTOR('',#25045,1.);
#7142=VECTOR('',#25054,1.05);
#7143=VECTOR('',#25063,1.);
#7144=VECTOR('',#25072,1.05);
#7145=VECTOR('',#25079,0.9);
#7146=VECTOR('',#25086,1.);
#7147=VECTOR('',#25089,1.);
#7148=VECTOR('',#25092,1.);
#7149=VECTOR('',#25093,1.);
#7150=VECTOR('',#25094,1.);
#7151=VECTOR('',#25101,1.);
#7152=VECTOR('',#25104,1.);
#7153=VECTOR('',#25105,1.);
#7154=VECTOR('',#25116,0.895);
#7155=VECTOR('',#25123,0.605);
#7156=VECTOR('',#25132,0.45);
#7157=VECTOR('',#25137,0.45);
#7158=VECTOR('',#25140,0.45);
#7159=VECTOR('',#25143,0.45);
#7160=VECTOR('',#25146,0.45);
#7161=VECTOR('',#25149,0.45);
#7162=VECTOR('',#25152,0.45);
#7163=VECTOR('',#25155,0.45);
#7164=VECTOR('',#25158,0.45);
#7165=VECTOR('',#25163,0.625);
#7166=VECTOR('',#25168,0.625);
#7167=VECTOR('',#25171,0.625);
#7168=VECTOR('',#25174,0.625);
#7169=VECTOR('',#25177,0.625);
#7170=VECTOR('',#25180,0.625);
#7171=VECTOR('',#25183,0.625);
#7172=VECTOR('',#25186,0.625);
#7173=VECTOR('',#25189,0.625);
#7174=VECTOR('',#25196,1.);
#7175=VECTOR('',#25211,0.225);
#7176=VECTOR('',#25216,0.225);
#7177=VECTOR('',#25221,0.225);
#7178=VECTOR('',#25224,1.);
#7179=VECTOR('',#25225,1.);
#7180=VECTOR('',#25226,1.);
#7181=VECTOR('',#25239,1.1);
#7182=VECTOR('',#25248,1.);
#7183=VECTOR('',#25249,1.);
#7184=VECTOR('',#25250,1.);
#7185=VECTOR('',#25251,1.);
#7186=VECTOR('',#25254,1.);
#7187=VECTOR('',#25255,1.);
#7188=VECTOR('',#25256,1.);
#7189=VECTOR('',#25259,1.);
#7190=VECTOR('',#25260,1.);
#7191=VECTOR('',#25261,1.);
#7192=VECTOR('',#25264,1.);
#7193=VECTOR('',#25265,1.);
#7194=VECTOR('',#25266,1.);
#7195=VECTOR('',#25269,1.);
#7196=VECTOR('',#25270,1.);
#7197=VECTOR('',#25271,1.);
#7198=VECTOR('',#25274,1.);
#7199=VECTOR('',#25275,1.);
#7200=VECTOR('',#25288,0.2);
#7201=VECTOR('',#25301,0.325);
#7202=VECTOR('',#25306,0.35);
#7203=VECTOR('',#25311,0.335);
#7204=VECTOR('',#25320,0.21);
#7205=VECTOR('',#25323,0.2);
#7206=VECTOR('',#25334,0.325);
#7207=VECTOR('',#25339,0.35);
#7208=VECTOR('',#25344,0.335);
#7209=VECTOR('',#25353,0.21);
#7210=VECTOR('',#25358,0.2);
#7211=VECTOR('',#25363,0.18);
#7212=VECTOR('',#25368,1.);
#7213=VECTOR('',#25369,1.);
#7214=VECTOR('',#25370,1.);
#7215=VECTOR('',#25371,1.);
#7216=VECTOR('',#25374,1.);
#7217=VECTOR('',#25375,1.);
#7218=VECTOR('',#25376,1.);
#7219=VECTOR('',#25379,1.);
#7220=VECTOR('',#25380,1.);
#7221=VECTOR('',#25381,1.);
#7222=VECTOR('',#25384,1.);
#7223=VECTOR('',#25385,1.);
#7224=VECTOR('',#25386,1.);
#7225=VECTOR('',#25389,1.);
#7226=VECTOR('',#25390,1.);
#7227=VECTOR('',#25391,1.);
#7228=VECTOR('',#25394,1.);
#7229=VECTOR('',#25395,1.);
#7230=VECTOR('',#25622,0.6);
#7231=VECTOR('',#25627,0.6);
#7232=VECTOR('',#25630,0.6);
#7233=VECTOR('',#25633,0.6);
#7234=VECTOR('',#25636,0.6);
#7235=VECTOR('',#25639,0.6);
#7236=VECTOR('',#25642,0.6);
#7237=VECTOR('',#25645,0.6);
#7238=VECTOR('',#25648,0.6);
#7239=VECTOR('',#25651,0.6);
#7240=VECTOR('',#25654,0.6);
#7241=VECTOR('',#25657,0.6);
#7242=VECTOR('',#25660,0.6);
#7243=VECTOR('',#25663,0.6);
#7244=VECTOR('',#25666,0.6);
#7245=VECTOR('',#25669,0.6);
#7246=VECTOR('',#25672,0.6);
#7247=VECTOR('',#25675,0.6);
#7248=VECTOR('',#25678,0.6);
#7249=VECTOR('',#25681,0.6);
#7250=VECTOR('',#25684,0.6);
#7251=VECTOR('',#25687,0.6);
#7252=VECTOR('',#25690,0.6);
#7253=VECTOR('',#25693,0.6);
#7254=VECTOR('',#25696,0.6);
#7255=VECTOR('',#25699,0.6);
#7256=VECTOR('',#25702,0.6);
#7257=VECTOR('',#25705,0.6);
#7258=VECTOR('',#25708,0.6);
#7259=VECTOR('',#25711,0.6);
#7260=VECTOR('',#25714,0.6);
#7261=VECTOR('',#25717,0.6);
#7262=VECTOR('',#25720,0.6);
#7263=VECTOR('',#25723,0.6);
#7264=VECTOR('',#25726,0.6);
#7265=VECTOR('',#25729,0.6);
#7266=VECTOR('',#25732,0.6);
#7267=VECTOR('',#25735,0.6);
#7268=VECTOR('',#25738,0.6);
#7269=VECTOR('',#25741,0.6);
#7270=VECTOR('',#25744,0.6);
#7271=VECTOR('',#25747,0.6);
#7272=VECTOR('',#25750,0.6);
#7273=VECTOR('',#25753,0.6);
#7274=VECTOR('',#25756,0.6);
#7275=VECTOR('',#25759,0.6);
#7276=VECTOR('',#25762,0.6);
#7277=VECTOR('',#25765,0.6);
#7278=VECTOR('',#25768,0.6);
#7279=VECTOR('',#25771,0.6);
#7280=VECTOR('',#25774,0.6);
#7281=VECTOR('',#25777,0.6);
#7282=VECTOR('',#25780,0.6);
#7283=VECTOR('',#25783,0.6);
#7284=VECTOR('',#25786,0.6);
#7285=VECTOR('',#25789,0.6);
#7286=VECTOR('',#25792,0.6);
#7287=VECTOR('',#25795,0.6);
#7288=VECTOR('',#25798,0.6);
#7289=VECTOR('',#25801,0.6);
#7290=VECTOR('',#25804,0.6);
#7291=VECTOR('',#25807,0.6);
#7292=VECTOR('',#25810,0.6);
#7293=VECTOR('',#25813,0.415875);
#7294=VECTOR('',#25818,0.415875);
#7295=VECTOR('',#25823,0.415875);
#7296=VECTOR('',#25826,0.415875);
#7297=VECTOR('',#25829,0.415875);
#7298=VECTOR('',#25832,0.415875);
#7299=VECTOR('',#25835,0.415875);
#7300=VECTOR('',#25838,0.415875);
#7301=VECTOR('',#25841,0.415875);
#7302=VECTOR('',#25844,0.415875);
#7303=VECTOR('',#25847,0.415875);
#7304=VECTOR('',#25850,0.415875);
#7305=VECTOR('',#25853,0.415875);
#7306=VECTOR('',#25856,0.415875);
#7307=VECTOR('',#25859,0.415875);
#7308=VECTOR('',#25862,0.415875);
#7309=VECTOR('',#25865,0.415875);
#7310=VECTOR('',#25868,0.415875);
#7311=VECTOR('',#25871,0.415875);
#7312=VECTOR('',#25874,0.415875);
#7313=VECTOR('',#25877,0.415875);
#7314=VECTOR('',#25880,0.415875);
#7315=VECTOR('',#25883,0.415875);
#7316=VECTOR('',#25886,0.415875);
#7317=VECTOR('',#25889,0.415875);
#7318=VECTOR('',#25892,0.415875);
#7319=VECTOR('',#25895,0.415875);
#7320=VECTOR('',#25898,0.415875);
#7321=VECTOR('',#25901,0.415875);
#7322=VECTOR('',#25904,0.415875);
#7323=VECTOR('',#25907,0.415875);
#7324=VECTOR('',#25910,0.415875);
#7325=VECTOR('',#25913,0.415875);
#7326=VECTOR('',#25916,0.415875);
#7327=VECTOR('',#25919,0.415875);
#7328=VECTOR('',#25922,0.415875);
#7329=VECTOR('',#25925,0.415875);
#7330=VECTOR('',#25928,0.415875);
#7331=VECTOR('',#25931,0.415875);
#7332=VECTOR('',#25934,0.415875);
#7333=VECTOR('',#25937,0.415875);
#7334=VECTOR('',#25940,0.415875);
#7335=VECTOR('',#25943,0.415875);
#7336=VECTOR('',#25946,0.415875);
#7337=VECTOR('',#25949,0.415875);
#7338=VECTOR('',#25952,0.415875);
#7339=VECTOR('',#25955,0.415875);
#7340=VECTOR('',#25958,0.415875);
#7341=VECTOR('',#25961,0.415875);
#7342=VECTOR('',#25964,0.415875);
#7343=VECTOR('',#25967,0.415875);
#7344=VECTOR('',#25970,0.415875);
#7345=VECTOR('',#25973,0.415875);
#7346=VECTOR('',#25976,0.415875);
#7347=VECTOR('',#25979,0.415875);
#7348=VECTOR('',#25982,0.415875);
#7349=VECTOR('',#25985,0.415875);
#7350=VECTOR('',#25988,0.415875);
#7351=VECTOR('',#25991,0.415875);
#7352=VECTOR('',#25994,0.415875);
#7353=VECTOR('',#25997,0.415875);
#7354=VECTOR('',#26000,0.415875);
#7355=VECTOR('',#26003,0.415875);
#7356=VECTOR('',#26012,0.6);
#7357=VECTOR('',#26021,1.);
#7358=VECTOR('',#26022,1.);
#7359=VECTOR('',#26023,1.);
#7360=VECTOR('',#26024,1.);
#7361=VECTOR('',#26029,1.);
#7362=VECTOR('',#26030,1.);
#7363=VECTOR('',#26033,1.);
#7364=VECTOR('',#26034,1.);
#7365=VECTOR('',#26037,1.);
#7366=VECTOR('',#26038,1.);
#7367=VECTOR('',#26047,1.);
#7368=VECTOR('',#26062,1.35);
#7369=VECTOR('',#26073,1.01);
#7370=VECTOR('',#26080,1.35);
#7371=VECTOR('',#26091,1.);
#7372=VECTOR('',#26098,0.210000000000001);
#7373=VECTOR('',#26101,1.);
#7374=VECTOR('',#26106,1.005);
#7375=VECTOR('',#26113,1.5);
#7376=VECTOR('',#26126,0.25);
#7377=VECTOR('',#26131,1.);
#7378=VECTOR('',#26138,0.210000000000001);
#7379=VECTOR('',#26141,1.);
#7380=VECTOR('',#26144,1.);
#7381=VECTOR('',#26145,1.);
#7382=VECTOR('',#26146,1.);
#7383=VECTOR('',#26147,1.);
#7384=VECTOR('',#26148,1.);
#7385=VECTOR('',#26149,1.);
#7386=VECTOR('',#26152,1.);
#7387=VECTOR('',#26153,1.);
#7388=VECTOR('',#26154,1.);
#7389=VECTOR('',#26157,1.);
#7390=VECTOR('',#26158,1.);
#7391=VECTOR('',#26159,1.);
#7392=VECTOR('',#26160,1.);
#7393=VECTOR('',#26161,1.);
#7394=VECTOR('',#26176,3.5);
#7395=VECTOR('',#26193,0.33);
#7396=VECTOR('',#26200,0.4);
#7397=VECTOR('',#26213,0.405);
#7398=VECTOR('',#26220,0.9);
#7399=VECTOR('',#26231,1.);
#7400=VECTOR('',#26232,1.);
#7401=VECTOR('',#26233,1.);
#7402=VECTOR('',#26234,1.);
#7403=VECTOR('',#26235,1.);
#7404=VECTOR('',#26236,1.);
#7405=VECTOR('',#26237,1.);
#7406=VECTOR('',#26238,1.);
#7407=VECTOR('',#26241,1.);
#7408=VECTOR('',#26242,1.);
#7409=VECTOR('',#26243,1.);
#7410=VECTOR('',#26246,1.);
#7411=VECTOR('',#26247,1.);
#7412=VECTOR('',#26250,1.);
#7413=VECTOR('',#26251,1.);
#7414=VECTOR('',#26254,1.);
#7415=VECTOR('',#26255,1.);
#7416=VECTOR('',#26258,1.);
#7417=VECTOR('',#26259,1.);
#7418=VECTOR('',#26260,1.);
#7419=VECTOR('',#26261,1.);
#7420=VECTOR('',#26264,1.);
#7421=VECTOR('',#26267,1.);
#7422=VECTOR('',#26270,1.);
#7423=VECTOR('',#26277,1.);
#7424=VECTOR('',#26278,1.);
#7425=VECTOR('',#26279,1.);
#7426=VECTOR('',#26280,1.);
#7427=VECTOR('',#26283,1.);
#7428=VECTOR('',#26284,1.);
#7429=VECTOR('',#26285,1.);
#7430=VECTOR('',#26288,1.);
#7431=VECTOR('',#26289,1.);
#7432=VECTOR('',#26290,1.);
#7433=VECTOR('',#26293,1.);
#7434=VECTOR('',#26294,1.);
#7435=VECTOR('',#26295,1.);
#7436=VECTOR('',#26298,1.);
#7437=VECTOR('',#26299,1.);
#7438=VECTOR('',#26300,1.);
#7439=VECTOR('',#26303,1.);
#7440=VECTOR('',#26304,1.);
#7441=VECTOR('',#26315,0.235);
#7442=VECTOR('',#26320,0.25);
#7443=VECTOR('',#26325,0.2125);
#7444=VECTOR('',#26334,0.32);
#7445=VECTOR('',#26341,0.6);
#7446=VECTOR('',#26358,0.475);
#7447=VECTOR('',#26363,0.5);
#7448=VECTOR('',#26368,0.485);
#7449=VECTOR('',#26377,0.31);
#7450=VECTOR('',#26382,0.3);
#7451=VECTOR('',#26387,0.27);
#7452=VECTOR('',#26392,1.);
#7453=VECTOR('',#26393,1.);
#7454=VECTOR('',#26394,1.);
#7455=VECTOR('',#26395,1.);
#7456=VECTOR('',#26398,1.);
#7457=VECTOR('',#26399,1.);
#7458=VECTOR('',#26400,1.);
#7459=VECTOR('',#26403,1.);
#7460=VECTOR('',#26404,1.);
#7461=VECTOR('',#26405,1.);
#7462=VECTOR('',#26408,1.);
#7463=VECTOR('',#26409,1.);
#7464=VECTOR('',#26410,1.);
#7465=VECTOR('',#26413,1.);
#7466=VECTOR('',#26414,1.);
#7467=VECTOR('',#26415,1.);
#7468=VECTOR('',#26418,1.);
#7469=VECTOR('',#26419,1.);
#7470=CIRCLE('',#19288,0.275);
#7471=CIRCLE('',#19289,0.275);
#7472=CIRCLE('',#19296,0.165);
#7473=CIRCLE('',#19297,0.165);
#7474=CIRCLE('',#19300,0.165);
#7475=CIRCLE('',#19301,0.165);
#7476=CIRCLE('',#19304,0.165);
#7477=CIRCLE('',#19305,0.165);
#7478=CIRCLE('',#19308,0.165);
#7479=CIRCLE('',#19309,0.165);
#7480=CIRCLE('',#19312,0.275);
#7481=CIRCLE('',#19313,0.275);
#7482=CIRCLE('',#19315,0.275);
#7483=CIRCLE('',#19316,0.275);
#7484=CIRCLE('',#19318,0.275);
#7485=CIRCLE('',#19319,0.275);
#7486=CIRCLE('',#19321,0.275);
#7487=CIRCLE('',#19322,0.275);
#7488=CIRCLE('',#19324,0.275);
#7489=CIRCLE('',#19325,0.275);
#7490=CIRCLE('',#19327,0.275);
#7491=CIRCLE('',#19328,0.275);
#7492=CIRCLE('',#19330,2.5);
#7493=CIRCLE('',#19331,2.5);
#7494=CIRCLE('',#19333,0.275);
#7495=CIRCLE('',#19334,0.275);
#7496=CIRCLE('',#19336,0.275);
#7497=CIRCLE('',#19337,0.275);
#7498=CIRCLE('',#19339,0.275);
#7499=CIRCLE('',#19340,0.275);
#7500=CIRCLE('',#19342,0.275);
#7501=CIRCLE('',#19343,0.275);
#7502=CIRCLE('',#19345,0.275);
#7503=CIRCLE('',#19346,0.275);
#7504=CIRCLE('',#19348,0.275);
#7505=CIRCLE('',#19349,0.275);
#7506=CIRCLE('',#19351,0.275);
#7507=CIRCLE('',#19352,0.275);
#7508=CIRCLE('',#19354,0.275);
#7509=CIRCLE('',#19355,0.275);
#7510=CIRCLE('',#19377,0.275);
#7511=CIRCLE('',#19378,0.275);
#7512=CIRCLE('',#19380,0.275);
#7513=CIRCLE('',#19381,0.275);
#7514=CIRCLE('',#19383,0.275);
#7515=CIRCLE('',#19384,0.275);
#7516=CIRCLE('',#19386,0.275);
#7517=CIRCLE('',#19387,0.275);
#7518=CIRCLE('',#19389,0.275);
#7519=CIRCLE('',#19390,0.275);
#7520=CIRCLE('',#19392,0.275);
#7521=CIRCLE('',#19393,0.275);
#7522=CIRCLE('',#19395,0.275);
#7523=CIRCLE('',#19396,0.275);
#7524=CIRCLE('',#19398,0.275);
#7525=CIRCLE('',#19399,0.275);
#7526=CIRCLE('',#19405,0.61);
#7527=CIRCLE('',#19406,0.61);
#7528=CIRCLE('',#19408,0.61);
#7529=CIRCLE('',#19409,0.61);
#7530=CIRCLE('',#19418,0.274999999999999);
#7531=CIRCLE('',#19419,0.274999999999999);
#7532=CIRCLE('',#19421,0.274999999999999);
#7533=CIRCLE('',#19422,0.274999999999999);
#7534=CIRCLE('',#19424,0.21);
#7535=CIRCLE('',#19425,0.21);
#7536=CIRCLE('',#19428,0.21);
#7537=CIRCLE('',#19429,0.21);
#7538=CIRCLE('',#19432,0.21);
#7539=CIRCLE('',#19433,0.21);
#7540=CIRCLE('',#19436,0.21);
#7541=CIRCLE('',#19437,0.21);
#7542=CIRCLE('',#19447,0.274999999999999);
#7543=CIRCLE('',#19448,0.274999999999999);
#7544=CIRCLE('',#19450,0.274999999999999);
#7545=CIRCLE('',#19451,0.274999999999999);
#7546=CIRCLE('',#19453,0.21);
#7547=CIRCLE('',#19454,0.21);
#7548=CIRCLE('',#19457,0.21);
#7549=CIRCLE('',#19458,0.21);
#7550=CIRCLE('',#19461,0.21);
#7551=CIRCLE('',#19462,0.21);
#7552=CIRCLE('',#19465,0.21);
#7553=CIRCLE('',#19466,0.21);
#7554=CIRCLE('',#19476,0.21);
#7555=CIRCLE('',#19477,0.21);
#7556=CIRCLE('',#19480,0.21);
#7557=CIRCLE('',#19481,0.21);
#7558=CIRCLE('',#19484,0.21);
#7559=CIRCLE('',#19485,0.21);
#7560=CIRCLE('',#19487,0.21);
#7561=CIRCLE('',#19488,0.21);
#7562=CIRCLE('',#19497,0.21);
#7563=CIRCLE('',#19498,0.21);
#7564=CIRCLE('',#19500,0.21);
#7565=CIRCLE('',#19501,0.21);
#7566=CIRCLE('',#19503,0.21);
#7567=CIRCLE('',#19504,0.21);
#7568=CIRCLE('',#19505,0.21);
#7569=CIRCLE('',#19506,0.21);
#7570=CIRCLE('',#19509,0.21);
#7571=CIRCLE('',#19510,0.21);
#7572=CIRCLE('',#19511,0.21);
#7573=CIRCLE('',#19512,0.21);
#7574=CIRCLE('',#19524,0.21);
#7575=CIRCLE('',#19525,0.21);
#7576=CIRCLE('',#19528,0.21);
#7577=CIRCLE('',#19529,0.21);
#7578=CIRCLE('',#19532,0.21);
#7579=CIRCLE('',#19533,0.21);
#7580=CIRCLE('',#19535,0.21);
#7581=CIRCLE('',#19536,0.21);
#7582=CIRCLE('',#19545,0.21);
#7583=CIRCLE('',#19546,0.21);
#7584=CIRCLE('',#19548,0.21);
#7585=CIRCLE('',#19549,0.21);
#7586=CIRCLE('',#19551,0.21);
#7587=CIRCLE('',#19552,0.21);
#7588=CIRCLE('',#19553,0.21);
#7589=CIRCLE('',#19554,0.21);
#7590=CIRCLE('',#19557,0.21);
#7591=CIRCLE('',#19558,0.21);
#7592=CIRCLE('',#19559,0.21);
#7593=CIRCLE('',#19560,0.21);
#7594=CIRCLE('',#19572,0.165);
#7595=CIRCLE('',#19573,0.165);
#7596=CIRCLE('',#19575,0.165);
#7597=CIRCLE('',#19576,0.165);
#7598=CIRCLE('',#19578,0.165);
#7599=CIRCLE('',#19579,0.165);
#7600=CIRCLE('',#19581,0.21);
#7601=CIRCLE('',#19582,0.21);
#7602=CIRCLE('',#19585,0.21);
#7603=CIRCLE('',#19586,0.21);
#7604=CIRCLE('',#19589,0.21);
#7605=CIRCLE('',#19590,0.21);
#7606=CIRCLE('',#19593,0.21);
#7607=CIRCLE('',#19594,0.21);
#7608=CIRCLE('',#19597,1.6);
#7609=CIRCLE('',#19598,1.6);
#7610=CIRCLE('',#19600,1.4);
#7611=CIRCLE('',#19602,1.4);
#7612=CIRCLE('',#19604,2.5);
#7613=CIRCLE('',#19605,2.5);
#7614=CIRCLE('',#19615,0.275);
#7615=CIRCLE('',#19616,0.275);
#7616=CIRCLE('',#19618,0.275);
#7617=CIRCLE('',#19619,0.275);
#7618=CIRCLE('',#19621,0.165);
#7619=CIRCLE('',#19622,0.165);
#7620=CIRCLE('',#19624,0.165);
#7621=CIRCLE('',#19625,0.165);
#7622=CIRCLE('',#19627,0.165);
#7623=CIRCLE('',#19628,0.165);
#7624=CIRCLE('',#19630,0.210000000000001);
#7625=CIRCLE('',#19631,0.210000000000001);
#7626=CIRCLE('',#19634,0.210000000000001);
#7627=CIRCLE('',#19635,0.210000000000001);
#7628=CIRCLE('',#19638,0.210000000000001);
#7629=CIRCLE('',#19639,0.210000000000001);
#7630=CIRCLE('',#19642,0.210000000000001);
#7631=CIRCLE('',#19643,0.210000000000001);
#7632=CIRCLE('',#19646,2.35);
#7633=CIRCLE('',#19647,2.35);
#7634=CIRCLE('',#19649,2.15);
#7635=CIRCLE('',#19651,2.15);
#7636=CIRCLE('',#19653,0.625);
#7637=CIRCLE('',#19654,0.625);
#7638=CIRCLE('',#19656,0.625);
#7639=CIRCLE('',#19657,0.625);
#7640=CIRCLE('',#19666,0.225);
#7641=CIRCLE('',#19667,0.225);
#7642=CIRCLE('',#19669,0.225);
#7643=CIRCLE('',#19670,0.225);
#7644=CIRCLE('',#19672,0.225);
#7645=CIRCLE('',#19673,0.225);
#7646=CIRCLE('',#19675,1.59);
#7647=CIRCLE('',#19676,1.59);
#7648=CIRCLE('',#19678,1.2);
#7649=CIRCLE('',#19680,1.2);
#7650=CIRCLE('',#19682,2.4);
#7651=CIRCLE('',#19683,2.4);
#7652=CIRCLE('',#19688,0.225);
#7653=CIRCLE('',#19689,0.225);
#7654=CIRCLE('',#19691,0.225);
#7655=CIRCLE('',#19692,0.225);
#7656=CIRCLE('',#19694,0.225);
#7657=CIRCLE('',#19695,0.225);
#7658=CIRCLE('',#19697,2.34);
#7659=CIRCLE('',#19698,2.34);
#7660=CIRCLE('',#19700,1.8);
#7661=CIRCLE('',#19702,1.8);
#7662=CIRCLE('',#19704,3.);
#7663=CIRCLE('',#19705,3.);
#7664=CIRCLE('',#19710,0.21);
#7665=CIRCLE('',#19711,0.21);
#7666=CIRCLE('',#19714,0.5);
#7667=CIRCLE('',#19715,0.5);
#7668=CIRCLE('',#19720,0.21);
#7669=CIRCLE('',#19721,0.21);
#7670=CIRCLE('',#19724,0.5);
#7671=CIRCLE('',#19725,0.5);
#7672=CIRCLE('',#19730,0.21);
#7673=CIRCLE('',#19731,0.21);
#7674=CIRCLE('',#19734,0.5);
#7675=CIRCLE('',#19735,0.5);
#7676=CIRCLE('',#19740,0.21);
#7677=CIRCLE('',#19741,0.21);
#7678=CIRCLE('',#19744,0.5);
#7679=CIRCLE('',#19745,0.5);
#7680=CIRCLE('',#19750,0.375);
#7681=CIRCLE('',#19751,0.375);
#7682=CIRCLE('',#19753,0.225);
#7683=CIRCLE('',#19755,0.375);
#7684=CIRCLE('',#19756,0.375);
#7685=CIRCLE('',#19758,0.225);
#7686=CIRCLE('',#19760,0.375);
#7687=CIRCLE('',#19761,0.375);
#7688=CIRCLE('',#19763,0.225);
#7689=CIRCLE('',#19765,0.375);
#7690=CIRCLE('',#19766,0.375);
#7691=CIRCLE('',#19768,0.225);
#7692=CIRCLE('',#19770,0.225);
#7693=CIRCLE('',#19772,0.225);
#7694=CIRCLE('',#19774,0.225);
#7695=CIRCLE('',#19776,0.225);
#7696=CIRCLE('',#19778,3.);
#7697=CIRCLE('',#19779,3.);
#7698=CIRCLE('',#19909,0.274999999999999);
#7699=CIRCLE('',#19910,0.274999999999999);
#7700=CIRCLE('',#19912,0.275);
#7701=CIRCLE('',#19913,0.275);
#7702=CIRCLE('',#19922,0.6);
#7703=CIRCLE('',#19923,0.5);
#7704=CIRCLE('',#19925,0.6);
#7705=CIRCLE('',#19928,0.5);
#7706=CIRCLE('',#19932,0.525);
#7707=CIRCLE('',#19934,0.525);
#7708=CIRCLE('',#19936,0.525);
#7709=CIRCLE('',#19937,0.525);
#7710=CIRCLE('',#19940,0.275);
#7711=CIRCLE('',#19942,0.165);
#7712=CIRCLE('',#19944,0.275);
#7713=CIRCLE('',#19946,0.225);
#7714=CIRCLE('',#19947,0.225);
#7715=CIRCLE('',#19949,0.165);
#7716=CIRCLE('',#19951,0.275);
#7717=CIRCLE('',#19953,0.275);
#7718=CIRCLE('',#19955,0.6);
#7719=CIRCLE('',#19956,0.6);
#7720=CIRCLE('',#19978,0.24505);
#7721=CIRCLE('',#19980,0.375);
#7722=CIRCLE('',#19982,0.425);
#7723=CIRCLE('',#19984,0.425);
#7724=CIRCLE('',#19986,0.395);
#7725=CIRCLE('',#19988,0.27);
#7726=CIRCLE('',#19990,0.24505);
#7727=CIRCLE('',#19995,1.070235);
#7728=CIRCLE('',#19996,1.070235);
#7729=CIRCLE('',#19997,0.309556);
#7730=CIRCLE('',#19998,1.070235);
#7731=CIRCLE('',#19999,1.070235);
#7732=CIRCLE('',#20001,1.070235);
#7733=CIRCLE('',#20003,0.6);
#7734=CIRCLE('',#20004,0.6);
#7735=CIRCLE('',#20006,0.66);
#7736=CIRCLE('',#20009,1.070235);
#7737=CIRCLE('',#20011,0.66);
#7738=CIRCLE('',#20015,1.129765);
#7739=CIRCLE('',#20016,1.129765);
#7740=CIRCLE('',#20017,0.309556);
#7741=CIRCLE('',#20018,1.129765);
#7742=CIRCLE('',#20019,1.129765);
#7743=CIRCLE('',#20021,1.129765);
#7744=CIRCLE('',#20023,1.54);
#7745=CIRCLE('',#20024,1.129765);
#7746=CIRCLE('',#20026,1.6);
#7747=CIRCLE('',#20028,1.6);
#7748=CIRCLE('',#20030,1.54);
#7749=CIRCLE('',#20035,0.29765);
#7750=CIRCLE('',#20037,0.29765);
#7751=CIRCLE('',#20039,0.29765);
#7752=CIRCLE('',#20041,0.29765);
#7753=CIRCLE('',#20043,0.29765);
#7754=CIRCLE('',#20045,0.29765);
#7755=CIRCLE('',#20047,0.29765);
#7756=CIRCLE('',#20050,0.303778037777585);
#7757=CIRCLE('',#20051,0.303778037777585);
#7758=CIRCLE('',#20053,1.123812);
#7759=CIRCLE('',#20054,1.123812);
#7760=CIRCLE('',#20055,1.123812);
#7761=CIRCLE('',#20056,1.123812);
#7762=CIRCLE('',#20057,1.123812);
#7763=CIRCLE('',#20058,1.123812);
#7764=CIRCLE('',#20059,1.123812);
#7765=CIRCLE('',#20060,1.123812);
#7766=CIRCLE('',#20061,1.123812);
#7767=CIRCLE('',#20063,1.076188);
#7768=CIRCLE('',#20064,0.303778037777585);
#7769=CIRCLE('',#20066,0.303778037777585);
#7770=CIRCLE('',#20068,1.076188);
#7771=CIRCLE('',#20069,0.303778037777585);
#7772=CIRCLE('',#20071,0.303778037777585);
#7773=CIRCLE('',#20073,1.076188);
#7774=CIRCLE('',#20074,1.076188);
#7775=CIRCLE('',#20075,0.303778037777585);
#7776=CIRCLE('',#20077,0.303778037777585);
#7777=CIRCLE('',#20079,1.076188);
#7778=CIRCLE('',#20080,0.303778037777585);
#7779=CIRCLE('',#20082,0.303778037777585);
#7780=CIRCLE('',#20084,1.076188);
#7781=CIRCLE('',#20085,0.303778037777585);
#7782=CIRCLE('',#20087,0.303778037777585);
#7783=CIRCLE('',#20089,1.076188);
#7784=CIRCLE('',#20090,1.076188);
#7785=CIRCLE('',#20091,1.076188);
#7786=CIRCLE('',#20093,0.303778037777585);
#7787=CIRCLE('',#20095,0.303778037777585);
#7788=CIRCLE('',#20100,1.119765);
#7789=CIRCLE('',#20101,1.085235);
#7790=CIRCLE('',#20103,1.119765);
#7791=CIRCLE('',#20105,1.085235);
#7792=CIRCLE('',#20108,1.119765);
#7793=CIRCLE('',#20109,1.085235);
#7794=CIRCLE('',#20111,1.119765);
#7795=CIRCLE('',#20113,1.085235);
#7796=CIRCLE('',#20123,1.63531);
#7797=CIRCLE('',#20124,1.63531);
#7798=CIRCLE('',#20125,0.412776);
#7799=CIRCLE('',#20126,1.63531);
#7800=CIRCLE('',#20127,1.63531);
#7801=CIRCLE('',#20129,1.63531);
#7802=CIRCLE('',#20131,1.);
#7803=CIRCLE('',#20132,1.);
#7804=CIRCLE('',#20134,1.1);
#7805=CIRCLE('',#20137,1.63531);
#7806=CIRCLE('',#20139,1.1);
#7807=CIRCLE('',#20143,1.71469);
#7808=CIRCLE('',#20144,1.71469);
#7809=CIRCLE('',#20145,0.412776);
#7810=CIRCLE('',#20146,1.71469);
#7811=CIRCLE('',#20147,1.71469);
#7812=CIRCLE('',#20149,1.71469);
#7813=CIRCLE('',#20151,2.25);
#7814=CIRCLE('',#20152,1.71469);
#7815=CIRCLE('',#20154,2.35);
#7816=CIRCLE('',#20156,2.35);
#7817=CIRCLE('',#20158,2.25);
#7818=CIRCLE('',#20163,0.3969);
#7819=CIRCLE('',#20165,0.3969);
#7820=CIRCLE('',#20167,0.3969);
#7821=CIRCLE('',#20169,0.3969);
#7822=CIRCLE('',#20171,0.3969);
#7823=CIRCLE('',#20173,0.3969);
#7824=CIRCLE('',#20175,0.3969);
#7825=CIRCLE('',#20177,0.3969);
#7826=CIRCLE('',#20180,0.405071403305639);
#7827=CIRCLE('',#20181,0.405071403305639);
#7828=CIRCLE('',#20183,1.706752);
#7829=CIRCLE('',#20184,1.706752);
#7830=CIRCLE('',#20185,1.706752);
#7831=CIRCLE('',#20186,1.706752);
#7832=CIRCLE('',#20187,1.706752);
#7833=CIRCLE('',#20188,1.706752);
#7834=CIRCLE('',#20189,1.706752);
#7835=CIRCLE('',#20190,1.706752);
#7836=CIRCLE('',#20191,1.706752);
#7837=CIRCLE('',#20193,1.643248);
#7838=CIRCLE('',#20194,0.405071403305639);
#7839=CIRCLE('',#20196,0.405071403305639);
#7840=CIRCLE('',#20198,1.643248);
#7841=CIRCLE('',#20199,0.405071403305639);
#7842=CIRCLE('',#20201,0.405071403305639);
#7843=CIRCLE('',#20203,1.643248);
#7844=CIRCLE('',#20204,0.405071403305639);
#7845=CIRCLE('',#20206,0.405071403305639);
#7846=CIRCLE('',#20208,1.643248);
#7847=CIRCLE('',#20209,0.405071403305639);
#7848=CIRCLE('',#20211,0.405071403305639);
#7849=CIRCLE('',#20213,1.643248);
#7850=CIRCLE('',#20214,0.405071403305639);
#7851=CIRCLE('',#20216,0.405071403305639);
#7852=CIRCLE('',#20218,1.643248);
#7853=CIRCLE('',#20219,0.405071403305639);
#7854=CIRCLE('',#20221,0.405071403305639);
#7855=CIRCLE('',#20223,1.643248);
#7856=CIRCLE('',#20224,1.643248);
#7857=CIRCLE('',#20225,1.643248);
#7858=CIRCLE('',#20227,0.405071403305639);
#7859=CIRCLE('',#20229,0.405071403305639);
#7860=CIRCLE('',#20234,1.70469);
#7861=CIRCLE('',#20235,1.65031);
#7862=CIRCLE('',#20237,1.70469);
#7863=CIRCLE('',#20239,1.65031);
#7864=CIRCLE('',#20242,1.70469);
#7865=CIRCLE('',#20243,1.65031);
#7866=CIRCLE('',#20245,1.70469);
#7867=CIRCLE('',#20247,1.65031);
#7868=CIRCLE('',#20256,0.25);
#7869=CIRCLE('',#20258,0.25);
#7870=CIRCLE('',#20259,0.24505);
#7871=CIRCLE('',#20262,0.375);
#7872=CIRCLE('',#20264,0.425);
#7873=CIRCLE('',#20266,0.425);
#7874=CIRCLE('',#20268,0.395);
#7875=CIRCLE('',#20270,0.27);
#7876=CIRCLE('',#20272,0.24505);
#7877=CIRCLE('',#20292,0.1954);
#7878=CIRCLE('',#20294,0.3);
#7879=CIRCLE('',#20296,0.35);
#7880=CIRCLE('',#20298,0.35);
#7881=CIRCLE('',#20300,0.32);
#7882=CIRCLE('',#20302,0.22);
#7883=CIRCLE('',#20304,0.1954);
#7884=CIRCLE('',#20344,0.21);
#7885=CIRCLE('',#20345,0.21);
#7886=CIRCLE('',#20358,0.375);
#7887=CIRCLE('',#20360,0.425);
#7888=CIRCLE('',#20362,0.425);
#7889=CIRCLE('',#20364,0.395);
#7890=CIRCLE('',#20366,0.27);
#7891=CIRCLE('',#20368,0.24505);
#7892=CIRCLE('',#20370,0.24505);
#7893=CIRCLE('',#20372,0.2);
#7894=CIRCLE('',#20386,0.2117);
#7895=CIRCLE('',#20395,0.2117);
#7896=CIRCLE('',#20396,0.2117);
#7897=CIRCLE('',#20398,0.2117);
#7898=CIRCLE('',#20405,0.24505);
#7899=CIRCLE('',#20407,0.375);
#7900=CIRCLE('',#20409,0.425);
#7901=CIRCLE('',#20411,0.425);
#7902=CIRCLE('',#20413,0.395);
#7903=CIRCLE('',#20415,0.27);
#7904=CIRCLE('',#20417,0.24505);
#7905=CIRCLE('',#20429,0.165);
#7906=CIRCLE('',#20430,0.165);
#7907=CIRCLE('',#20432,0.165);
#7908=CIRCLE('',#20433,0.165);
#7909=CIRCLE('',#20435,0.225);
#7910=CIRCLE('',#20436,0.225);
#7911=CIRCLE('',#20438,0.225);
#7912=CIRCLE('',#20439,0.225);
#7913=CIRCLE('',#20441,0.225);
#7914=CIRCLE('',#20442,0.225);
#7915=CIRCLE('',#20444,0.225);
#7916=CIRCLE('',#20445,0.225);
#7917=CIRCLE('',#20447,0.225);
#7918=CIRCLE('',#20448,0.225);
#7919=CIRCLE('',#20450,0.225);
#7920=CIRCLE('',#20451,0.225);
#7921=CIRCLE('',#20453,0.225);
#7922=CIRCLE('',#20454,0.225);
#7923=CIRCLE('',#20456,0.225);
#7924=CIRCLE('',#20457,0.225);
#7925=CIRCLE('',#20459,0.225);
#7926=CIRCLE('',#20460,0.225);
#7927=CIRCLE('',#20462,0.225);
#7928=CIRCLE('',#20463,0.225);
#7929=CIRCLE('',#20465,0.225);
#7930=CIRCLE('',#20466,0.225);
#7931=CIRCLE('',#20468,0.225);
#7932=CIRCLE('',#20469,0.225);
#7933=CIRCLE('',#20471,0.225);
#7934=CIRCLE('',#20472,0.225);
#7935=CIRCLE('',#20474,0.625);
#7936=CIRCLE('',#20475,0.625);
#7937=CIRCLE('',#20477,0.625);
#7938=CIRCLE('',#20478,0.625);
#7939=CIRCLE('',#20480,0.625);
#7940=CIRCLE('',#20481,0.625);
#7941=CIRCLE('',#20490,1.5);
#7942=CIRCLE('',#20491,0.165);
#7943=CIRCLE('',#20493,0.165);
#7944=CIRCLE('',#20494,0.165);
#7945=CIRCLE('',#20495,0.165);
#7946=CIRCLE('',#20497,1.5);
#7947=CIRCLE('',#20498,0.165);
#7948=CIRCLE('',#20500,0.165);
#7949=CIRCLE('',#20501,0.165);
#7950=CIRCLE('',#20502,0.165);
#7951=CIRCLE('',#20504,1.5);
#7952=CIRCLE('',#20505,0.165);
#7953=CIRCLE('',#20506,0.165);
#7954=CIRCLE('',#20508,0.165);
#7955=CIRCLE('',#20509,0.165);
#7956=CIRCLE('',#20511,1.5);
#7957=CIRCLE('',#20512,0.165);
#7958=CIRCLE('',#20513,0.165);
#7959=CIRCLE('',#20515,0.165);
#7960=CIRCLE('',#20516,0.165);
#7961=CIRCLE('',#20518,1.5);
#7962=CIRCLE('',#20519,1.5);
#7963=CIRCLE('',#20520,1.5);
#7964=CIRCLE('',#20521,1.5);
#7965=CIRCLE('',#20522,1.5);
#7966=CIRCLE('',#20523,1.5);
#7967=CIRCLE('',#20525,1.05);
#7968=CIRCLE('',#20526,1.05);
#7969=CIRCLE('',#20528,0.625);
#7970=CIRCLE('',#20530,2.);
#7971=CIRCLE('',#20532,2.);
#7972=CIRCLE('',#20534,0.625);
#7973=CIRCLE('',#20539,1.5);
#7974=CIRCLE('',#20540,0.165);
#7975=CIRCLE('',#20542,0.165);
#7976=CIRCLE('',#20543,0.165);
#7977=CIRCLE('',#20544,0.165);
#7978=CIRCLE('',#20546,1.5);
#7979=CIRCLE('',#20547,0.165);
#7980=CIRCLE('',#20549,0.165);
#7981=CIRCLE('',#20550,0.165);
#7982=CIRCLE('',#20551,0.165);
#7983=CIRCLE('',#20553,1.5);
#7984=CIRCLE('',#20554,0.165);
#7985=CIRCLE('',#20555,0.165);
#7986=CIRCLE('',#20557,0.165);
#7987=CIRCLE('',#20558,0.165);
#7988=CIRCLE('',#20560,1.5);
#7989=CIRCLE('',#20561,0.165);
#7990=CIRCLE('',#20562,0.165);
#7991=CIRCLE('',#20564,0.165);
#7992=CIRCLE('',#20565,0.165);
#7993=CIRCLE('',#20567,1.5);
#7994=CIRCLE('',#20568,1.5);
#7995=CIRCLE('',#20569,1.5);
#7996=CIRCLE('',#20570,1.5);
#7997=CIRCLE('',#20571,1.5);
#7998=CIRCLE('',#20572,1.5);
#7999=CIRCLE('',#20574,1.05);
#8000=CIRCLE('',#20575,1.05);
#8001=CIRCLE('',#20577,0.625);
#8002=CIRCLE('',#20579,2.);
#8003=CIRCLE('',#20581,2.);
#8004=CIRCLE('',#20583,0.625);
#8005=CIRCLE('',#20588,0.165);
#8006=CIRCLE('',#20589,0.165);
#8007=CIRCLE('',#20592,0.165);
#8008=CIRCLE('',#20593,0.165);
#8009=CIRCLE('',#20596,0.165);
#8010=CIRCLE('',#20597,0.165);
#8011=CIRCLE('',#20600,1.11);
#8012=CIRCLE('',#20601,1.11);
#8013=CIRCLE('',#20603,2.2);
#8014=CIRCLE('',#20604,2.2);
#8015=CIRCLE('',#20609,0.165);
#8016=CIRCLE('',#20610,0.165);
#8017=CIRCLE('',#20612,0.165);
#8018=CIRCLE('',#20613,0.165);
#8019=CIRCLE('',#20615,3.);
#8020=CIRCLE('',#20616,3.);
#8021=CIRCLE('',#20621,0.225);
#8022=CIRCLE('',#20622,0.225);
#8023=CIRCLE('',#20624,0.225);
#8024=CIRCLE('',#20625,0.225);
#8025=CIRCLE('',#20642,0.9);
#8026=CIRCLE('',#20645,0.9);
#8027=CIRCLE('',#20649,1.05);
#8028=CIRCLE('',#20650,0.9);
#8029=CIRCLE('',#20652,1.05);
#8030=CIRCLE('',#20654,1.);
#8031=CIRCLE('',#20656,1.);
#8032=CIRCLE('',#20658,1.05);
#8033=CIRCLE('',#20660,1.05);
#8034=CIRCLE('',#20662,1.);
#8035=CIRCLE('',#20664,1.);
#8036=CIRCLE('',#20666,1.05);
#8037=CIRCLE('',#20668,1.05);
#8038=CIRCLE('',#20670,0.9);
#8039=CIRCLE('',#20674,0.895);
#8040=CIRCLE('',#20675,0.605);
#8041=CIRCLE('',#20678,0.895);
#8042=CIRCLE('',#20679,0.605);
#8043=CIRCLE('',#20682,0.895);
#8044=CIRCLE('',#20683,0.605);
#8045=CIRCLE('',#20685,0.895);
#8046=CIRCLE('',#20687,0.605);
#8047=CIRCLE('',#20693,0.457875);
#8048=CIRCLE('',#20702,0.457875);
#8049=CIRCLE('',#20704,0.625);
#8050=CIRCLE('',#20713,0.625);
#8051=CIRCLE('',#20716,1.9);
#8052=CIRCLE('',#20717,0.457875);
#8053=CIRCLE('',#20718,0.225);
#8054=CIRCLE('',#20719,0.225);
#8055=CIRCLE('',#20720,0.225);
#8056=CIRCLE('',#20722,0.225);
#8057=CIRCLE('',#20724,0.225);
#8058=CIRCLE('',#20726,0.225);
#8059=CIRCLE('',#20729,1.9);
#8060=CIRCLE('',#20730,1.1);
#8061=CIRCLE('',#20734,1.1);
#8062=CIRCLE('',#20746,0.2);
#8063=CIRCLE('',#20747,0.1954);
#8064=CIRCLE('',#20749,0.2);
#8065=CIRCLE('',#20752,0.3);
#8066=CIRCLE('',#20754,0.35);
#8067=CIRCLE('',#20756,0.35);
#8068=CIRCLE('',#20758,0.32);
#8069=CIRCLE('',#20760,0.22);
#8070=CIRCLE('',#20762,0.1954);
#8071=CIRCLE('',#20766,0.3);
#8072=CIRCLE('',#20768,0.35);
#8073=CIRCLE('',#20770,0.35);
#8074=CIRCLE('',#20772,0.32);
#8075=CIRCLE('',#20774,0.22);
#8076=CIRCLE('',#20776,0.1954);
#8077=CIRCLE('',#20778,0.1954);
#8078=CIRCLE('',#20780,0.16);
#8079=CIRCLE('',#20901,0.5941);
#8080=CIRCLE('',#20965,0.415875);
#8081=CIRCLE('',#20967,0.415875);
#8082=CIRCLE('',#21030,0.6);
#8083=CIRCLE('',#21031,0.415875);
#8084=CIRCLE('',#21033,0.6);
#8085=CIRCLE('',#21038,1.);
#8086=CIRCLE('',#21042,1.);
#8087=CIRCLE('',#21044,1.);
#8088=CIRCLE('',#21045,1.);
#8089=CIRCLE('',#21048,1.35);
#8090=CIRCLE('',#21049,0.5941);
#8091=CIRCLE('',#21051,1.35);
#8092=CIRCLE('',#21056,1.01);
#8093=CIRCLE('',#21057,1.01);
#8094=CIRCLE('',#21059,1.35);
#8095=CIRCLE('',#21060,1.35);
#8096=CIRCLE('',#21065,0.210000000000001);
#8097=CIRCLE('',#21067,0.210000000000001);
#8098=CIRCLE('',#21070,1.005);
#8099=CIRCLE('',#21071,1.005);
#8100=CIRCLE('',#21073,1.5);
#8101=CIRCLE('',#21074,1.5);
#8102=CIRCLE('',#21079,0.25);
#8103=CIRCLE('',#21080,0.25);
#8104=CIRCLE('',#21082,0.210000000000001);
#8105=CIRCLE('',#21084,0.210000000000001);
#8106=CIRCLE('',#21090,3.5);
#8107=CIRCLE('',#21091,1.);
#8108=CIRCLE('',#21093,3.5);
#8109=CIRCLE('',#21094,1.5);
#8110=CIRCLE('',#21097,1.);
#8111=CIRCLE('',#21099,1.5);
#8112=CIRCLE('',#21103,0.33);
#8113=CIRCLE('',#21104,0.33);
#8114=CIRCLE('',#21106,0.4);
#8115=CIRCLE('',#21107,0.4);
#8116=CIRCLE('',#21112,0.405);
#8117=CIRCLE('',#21113,0.405);
#8118=CIRCLE('',#21115,0.9);
#8119=CIRCLE('',#21116,0.9);
#8120=CIRCLE('',#21139,0.22);
#8121=CIRCLE('',#21141,0.24505);
#8122=CIRCLE('',#21143,0.24505);
#8123=CIRCLE('',#21145,0.175);
#8124=CIRCLE('',#21149,0.32);
#8125=CIRCLE('',#21150,0.32);
#8126=CIRCLE('',#21152,0.6);
#8127=CIRCLE('',#21153,0.6);
#8128=CIRCLE('',#21158,0.45);
#8129=CIRCLE('',#21160,0.5);
#8130=CIRCLE('',#21162,0.5);
#8131=CIRCLE('',#21164,0.47);
#8132=CIRCLE('',#21166,0.32);
#8133=CIRCLE('',#21168,0.2942);
#8134=CIRCLE('',#21170,0.2942);
#8135=CIRCLE('',#21172,0.24);
#8136=VERTEX_POINT('',#26456);
#8137=VERTEX_POINT('',#26458);
#8138=VERTEX_POINT('',#26462);
#8139=VERTEX_POINT('',#26463);
#8140=VERTEX_POINT('',#26465);
#8141=VERTEX_POINT('',#26467);
#8142=VERTEX_POINT('',#26471);
#8143=VERTEX_POINT('',#26472);
#8144=VERTEX_POINT('',#26477);
#8145=VERTEX_POINT('',#26478);
#8146=VERTEX_POINT('',#26483);
#8147=VERTEX_POINT('',#26485);
#8148=VERTEX_POINT('',#26489);
#8149=VERTEX_POINT('',#26491);
#8150=VERTEX_POINT('',#26495);
#8151=VERTEX_POINT('',#26497);
#8152=VERTEX_POINT('',#26502);
#8153=VERTEX_POINT('',#26504);
#8154=VERTEX_POINT('',#26509);
#8155=VERTEX_POINT('',#26511);
#8156=VERTEX_POINT('',#26516);
#8157=VERTEX_POINT('',#26518);
#8158=VERTEX_POINT('',#26523);
#8159=VERTEX_POINT('',#26525);
#8160=VERTEX_POINT('',#26529);
#8161=VERTEX_POINT('',#26531);
#8162=VERTEX_POINT('',#26535);
#8163=VERTEX_POINT('',#26537);
#8164=VERTEX_POINT('',#26541);
#8165=VERTEX_POINT('',#26543);
#8166=VERTEX_POINT('',#26547);
#8167=VERTEX_POINT('',#26549);
#8168=VERTEX_POINT('',#26553);
#8169=VERTEX_POINT('',#26555);
#8170=VERTEX_POINT('',#26559);
#8171=VERTEX_POINT('',#26561);
#8172=VERTEX_POINT('',#26565);
#8173=VERTEX_POINT('',#26567);
#8174=VERTEX_POINT('',#26571);
#8175=VERTEX_POINT('',#26573);
#8176=VERTEX_POINT('',#26577);
#8177=VERTEX_POINT('',#26579);
#8178=VERTEX_POINT('',#26583);
#8179=VERTEX_POINT('',#26585);
#8180=VERTEX_POINT('',#26589);
#8181=VERTEX_POINT('',#26591);
#8182=VERTEX_POINT('',#26595);
#8183=VERTEX_POINT('',#26597);
#8184=VERTEX_POINT('',#26601);
#8185=VERTEX_POINT('',#26603);
#8186=VERTEX_POINT('',#26607);
#8187=VERTEX_POINT('',#26609);
#8188=VERTEX_POINT('',#26613);
#8189=VERTEX_POINT('',#26615);
#8190=VERTEX_POINT('',#26619);
#8191=VERTEX_POINT('',#26621);
#8192=VERTEX_POINT('',#26631);
#8193=VERTEX_POINT('',#26632);
#8194=VERTEX_POINT('',#26634);
#8195=VERTEX_POINT('',#26636);
#8196=VERTEX_POINT('',#26640);
#8197=VERTEX_POINT('',#26642);
#8198=VERTEX_POINT('',#26646);
#8199=VERTEX_POINT('',#26648);
#8200=VERTEX_POINT('',#26658);
#8201=VERTEX_POINT('',#26659);
#8202=VERTEX_POINT('',#26661);
#8203=VERTEX_POINT('',#26663);
#8204=VERTEX_POINT('',#26667);
#8205=VERTEX_POINT('',#26669);
#8206=VERTEX_POINT('',#26673);
#8207=VERTEX_POINT('',#26675);
#8208=VERTEX_POINT('',#26685);
#8209=VERTEX_POINT('',#26687);
#8210=VERTEX_POINT('',#26691);
#8211=VERTEX_POINT('',#26693);
#8212=VERTEX_POINT('',#26697);
#8213=VERTEX_POINT('',#26699);
#8214=VERTEX_POINT('',#26703);
#8215=VERTEX_POINT('',#26705);
#8216=VERTEX_POINT('',#26709);
#8217=VERTEX_POINT('',#26711);
#8218=VERTEX_POINT('',#26715);
#8219=VERTEX_POINT('',#26717);
#8220=VERTEX_POINT('',#26721);
#8221=VERTEX_POINT('',#26723);
#8222=VERTEX_POINT('',#26727);
#8223=VERTEX_POINT('',#26729);
#8224=VERTEX_POINT('',#26733);
#8225=VERTEX_POINT('',#26734);
#8226=VERTEX_POINT('',#26736);
#8227=VERTEX_POINT('',#26738);
#8228=VERTEX_POINT('',#26742);
#8229=VERTEX_POINT('',#26744);
#8230=VERTEX_POINT('',#26748);
#8231=VERTEX_POINT('',#26750);
#8232=VERTEX_POINT('',#26757);
#8233=VERTEX_POINT('',#26759);
#8234=VERTEX_POINT('',#26763);
#8235=VERTEX_POINT('',#26765);
#8236=VERTEX_POINT('',#26769);
#8237=VERTEX_POINT('',#26770);
#8238=VERTEX_POINT('',#26772);
#8239=VERTEX_POINT('',#26774);
#8240=VERTEX_POINT('',#26778);
#8241=VERTEX_POINT('',#26780);
#8242=VERTEX_POINT('',#26784);
#8243=VERTEX_POINT('',#26786);
#8244=VERTEX_POINT('',#26796);
#8245=VERTEX_POINT('',#26798);
#8246=VERTEX_POINT('',#26802);
#8247=VERTEX_POINT('',#26804);
#8248=VERTEX_POINT('',#26808);
#8249=VERTEX_POINT('',#26810);
#8250=VERTEX_POINT('',#26815);
#8251=VERTEX_POINT('',#26817);
#8252=VERTEX_POINT('',#26822);
#8253=VERTEX_POINT('',#26824);
#8254=VERTEX_POINT('',#26829);
#8255=VERTEX_POINT('',#26831);
#8256=VERTEX_POINT('',#26836);
#8257=VERTEX_POINT('',#26837);
#8258=VERTEX_POINT('',#26839);
#8259=VERTEX_POINT('',#26841);
#8260=VERTEX_POINT('',#26845);
#8261=VERTEX_POINT('',#26847);
#8262=VERTEX_POINT('',#26851);
#8263=VERTEX_POINT('',#26853);
#8264=VERTEX_POINT('',#26863);
#8265=VERTEX_POINT('',#26865);
#8266=VERTEX_POINT('',#26869);
#8267=VERTEX_POINT('',#26871);
#8268=VERTEX_POINT('',#26875);
#8269=VERTEX_POINT('',#26877);
#8270=VERTEX_POINT('',#26882);
#8271=VERTEX_POINT('',#26884);
#8272=VERTEX_POINT('',#26889);
#8273=VERTEX_POINT('',#26891);
#8274=VERTEX_POINT('',#26896);
#8275=VERTEX_POINT('',#26898);
#8276=VERTEX_POINT('',#26903);
#8277=VERTEX_POINT('',#26904);
#8278=VERTEX_POINT('',#26906);
#8279=VERTEX_POINT('',#26908);
#8280=VERTEX_POINT('',#26912);
#8281=VERTEX_POINT('',#26914);
#8282=VERTEX_POINT('',#26918);
#8283=VERTEX_POINT('',#26920);
#8284=VERTEX_POINT('',#26930);
#8285=VERTEX_POINT('',#26932);
#8286=VERTEX_POINT('',#26937);
#8287=VERTEX_POINT('',#26939);
#8288=VERTEX_POINT('',#26944);
#8289=VERTEX_POINT('',#26946);
#8290=VERTEX_POINT('',#26950);
#8291=VERTEX_POINT('',#26952);
#8292=VERTEX_POINT('',#26956);
#8293=VERTEX_POINT('',#26957);
#8294=VERTEX_POINT('',#26959);
#8295=VERTEX_POINT('',#26961);
#8296=VERTEX_POINT('',#26965);
#8297=VERTEX_POINT('',#26967);
#8298=VERTEX_POINT('',#26971);
#8299=VERTEX_POINT('',#26973);
#8300=VERTEX_POINT('',#26983);
#8301=VERTEX_POINT('',#26985);
#8302=VERTEX_POINT('',#26989);
#8303=VERTEX_POINT('',#26991);
#8304=VERTEX_POINT('',#26995);
#8305=VERTEX_POINT('',#26997);
#8306=VERTEX_POINT('',#26999);
#8307=VERTEX_POINT('',#27001);
#8308=VERTEX_POINT('',#27003);
#8309=VERTEX_POINT('',#27005);
#8310=VERTEX_POINT('',#27011);
#8311=VERTEX_POINT('',#27013);
#8312=VERTEX_POINT('',#27015);
#8313=VERTEX_POINT('',#27017);
#8314=VERTEX_POINT('',#27019);
#8315=VERTEX_POINT('',#27021);
#8316=VERTEX_POINT('',#27028);
#8317=VERTEX_POINT('',#27030);
#8318=VERTEX_POINT('',#27032);
#8319=VERTEX_POINT('',#27034);
#8320=VERTEX_POINT('',#27038);
#8321=VERTEX_POINT('',#27040);
#8322=VERTEX_POINT('',#27044);
#8323=VERTEX_POINT('',#27045);
#8324=VERTEX_POINT('',#27050);
#8325=VERTEX_POINT('',#27051);
#8326=VERTEX_POINT('',#27056);
#8327=VERTEX_POINT('',#27057);
#8328=VERTEX_POINT('',#27068);
#8329=VERTEX_POINT('',#27070);
#8330=VERTEX_POINT('',#27075);
#8331=VERTEX_POINT('',#27077);
#8332=VERTEX_POINT('',#27082);
#8333=VERTEX_POINT('',#27084);
#8334=VERTEX_POINT('',#27088);
#8335=VERTEX_POINT('',#27090);
#8336=VERTEX_POINT('',#27094);
#8337=VERTEX_POINT('',#27095);
#8338=VERTEX_POINT('',#27097);
#8339=VERTEX_POINT('',#27099);
#8340=VERTEX_POINT('',#27103);
#8341=VERTEX_POINT('',#27105);
#8342=VERTEX_POINT('',#27109);
#8343=VERTEX_POINT('',#27111);
#8344=VERTEX_POINT('',#27121);
#8345=VERTEX_POINT('',#27123);
#8346=VERTEX_POINT('',#27127);
#8347=VERTEX_POINT('',#27129);
#8348=VERTEX_POINT('',#27133);
#8349=VERTEX_POINT('',#27135);
#8350=VERTEX_POINT('',#27137);
#8351=VERTEX_POINT('',#27139);
#8352=VERTEX_POINT('',#27141);
#8353=VERTEX_POINT('',#27143);
#8354=VERTEX_POINT('',#27149);
#8355=VERTEX_POINT('',#27151);
#8356=VERTEX_POINT('',#27153);
#8357=VERTEX_POINT('',#27155);
#8358=VERTEX_POINT('',#27157);
#8359=VERTEX_POINT('',#27159);
#8360=VERTEX_POINT('',#27166);
#8361=VERTEX_POINT('',#27168);
#8362=VERTEX_POINT('',#27170);
#8363=VERTEX_POINT('',#27172);
#8364=VERTEX_POINT('',#27176);
#8365=VERTEX_POINT('',#27178);
#8366=VERTEX_POINT('',#27182);
#8367=VERTEX_POINT('',#27183);
#8368=VERTEX_POINT('',#27188);
#8369=VERTEX_POINT('',#27189);
#8370=VERTEX_POINT('',#27194);
#8371=VERTEX_POINT('',#27195);
#8372=VERTEX_POINT('',#27206);
#8373=VERTEX_POINT('',#27208);
#8374=VERTEX_POINT('',#27212);
#8375=VERTEX_POINT('',#27214);
#8376=VERTEX_POINT('',#27218);
#8377=VERTEX_POINT('',#27220);
#8378=VERTEX_POINT('',#27224);
#8379=VERTEX_POINT('',#27226);
#8380=VERTEX_POINT('',#27231);
#8381=VERTEX_POINT('',#27233);
#8382=VERTEX_POINT('',#27238);
#8383=VERTEX_POINT('',#27240);
#8384=VERTEX_POINT('',#27245);
#8385=VERTEX_POINT('',#27247);
#8386=VERTEX_POINT('',#27252);
#8387=VERTEX_POINT('',#27254);
#8388=VERTEX_POINT('',#27258);
#8389=VERTEX_POINT('',#27261);
#8390=VERTEX_POINT('',#27265);
#8391=VERTEX_POINT('',#27267);
#8392=VERTEX_POINT('',#27272);
#8393=VERTEX_POINT('',#27273);
#8394=VERTEX_POINT('',#27275);
#8395=VERTEX_POINT('',#27277);
#8396=VERTEX_POINT('',#27281);
#8397=VERTEX_POINT('',#27283);
#8398=VERTEX_POINT('',#27287);
#8399=VERTEX_POINT('',#27289);
#8400=VERTEX_POINT('',#27299);
#8401=VERTEX_POINT('',#27301);
#8402=VERTEX_POINT('',#27305);
#8403=VERTEX_POINT('',#27307);
#8404=VERTEX_POINT('',#27311);
#8405=VERTEX_POINT('',#27313);
#8406=VERTEX_POINT('',#27317);
#8407=VERTEX_POINT('',#27319);
#8408=VERTEX_POINT('',#27323);
#8409=VERTEX_POINT('',#27325);
#8410=VERTEX_POINT('',#27329);
#8411=VERTEX_POINT('',#27331);
#8412=VERTEX_POINT('',#27336);
#8413=VERTEX_POINT('',#27338);
#8414=VERTEX_POINT('',#27343);
#8415=VERTEX_POINT('',#27345);
#8416=VERTEX_POINT('',#27350);
#8417=VERTEX_POINT('',#27352);
#8418=VERTEX_POINT('',#27357);
#8419=VERTEX_POINT('',#27359);
#8420=VERTEX_POINT('',#27363);
#8421=VERTEX_POINT('',#27366);
#8422=VERTEX_POINT('',#27370);
#8423=VERTEX_POINT('',#27371);
#8424=VERTEX_POINT('',#27373);
#8425=VERTEX_POINT('',#27375);
#8426=VERTEX_POINT('',#27379);
#8427=VERTEX_POINT('',#27380);
#8428=VERTEX_POINT('',#27382);
#8429=VERTEX_POINT('',#27384);
#8430=VERTEX_POINT('',#27388);
#8431=VERTEX_POINT('',#27390);
#8432=VERTEX_POINT('',#27394);
#8433=VERTEX_POINT('',#27401);
#8434=VERTEX_POINT('',#27409);
#8435=VERTEX_POINT('',#27411);
#8436=VERTEX_POINT('',#27415);
#8437=VERTEX_POINT('',#27417);
#8438=VERTEX_POINT('',#27421);
#8439=VERTEX_POINT('',#27423);
#8440=VERTEX_POINT('',#27427);
#8441=VERTEX_POINT('',#27429);
#8442=VERTEX_POINT('',#27433);
#8443=VERTEX_POINT('',#27436);
#8444=VERTEX_POINT('',#27440);
#8445=VERTEX_POINT('',#27442);
#8446=VERTEX_POINT('',#27449);
#8447=VERTEX_POINT('',#27451);
#8448=VERTEX_POINT('',#27455);
#8449=VERTEX_POINT('',#27457);
#8450=VERTEX_POINT('',#27461);
#8451=VERTEX_POINT('',#27463);
#8452=VERTEX_POINT('',#27467);
#8453=VERTEX_POINT('',#27469);
#8454=VERTEX_POINT('',#27473);
#8455=VERTEX_POINT('',#27476);
#8456=VERTEX_POINT('',#27480);
#8457=VERTEX_POINT('',#27482);
#8458=VERTEX_POINT('',#27489);
#8459=VERTEX_POINT('',#27491);
#8460=VERTEX_POINT('',#27496);
#8461=VERTEX_POINT('',#27498);
#8462=VERTEX_POINT('',#27505);
#8463=VERTEX_POINT('',#27507);
#8464=VERTEX_POINT('',#27512);
#8465=VERTEX_POINT('',#27514);
#8466=VERTEX_POINT('',#27521);
#8467=VERTEX_POINT('',#27523);
#8468=VERTEX_POINT('',#27528);
#8469=VERTEX_POINT('',#27530);
#8470=VERTEX_POINT('',#27537);
#8471=VERTEX_POINT('',#27539);
#8472=VERTEX_POINT('',#27544);
#8473=VERTEX_POINT('',#27546);
#8474=VERTEX_POINT('',#27553);
#8475=VERTEX_POINT('',#27555);
#8476=VERTEX_POINT('',#27559);
#8477=VERTEX_POINT('',#27562);
#8478=VERTEX_POINT('',#27564);
#8479=VERTEX_POINT('',#27568);
#8480=VERTEX_POINT('',#27571);
#8481=VERTEX_POINT('',#27573);
#8482=VERTEX_POINT('',#27577);
#8483=VERTEX_POINT('',#27580);
#8484=VERTEX_POINT('',#27582);
#8485=VERTEX_POINT('',#27586);
#8486=VERTEX_POINT('',#27589);
#8487=VERTEX_POINT('',#27593);
#8488=VERTEX_POINT('',#27597);
#8489=VERTEX_POINT('',#27601);
#8490=VERTEX_POINT('',#27605);
#8491=VERTEX_POINT('',#27607);
#8492=VERTEX_POINT('',#27614);
#8493=VERTEX_POINT('',#27615);
#8494=VERTEX_POINT('',#27617);
#8495=VERTEX_POINT('',#27619);
#8496=VERTEX_POINT('',#27623);
#8497=VERTEX_POINT('',#27625);
#8498=VERTEX_POINT('',#27629);
#8499=VERTEX_POINT('',#27631);
#8500=VERTEX_POINT('',#27639);
#8501=VERTEX_POINT('',#27640);
#8502=VERTEX_POINT('',#27642);
#8503=VERTEX_POINT('',#27644);
#8504=VERTEX_POINT('',#27648);
#8505=VERTEX_POINT('',#27650);
#8506=VERTEX_POINT('',#27654);
#8507=VERTEX_POINT('',#27656);
#8508=VERTEX_POINT('',#27664);
#8509=VERTEX_POINT('',#27665);
#8510=VERTEX_POINT('',#27667);
#8511=VERTEX_POINT('',#27669);
#8512=VERTEX_POINT('',#27673);
#8513=VERTEX_POINT('',#27675);
#8514=VERTEX_POINT('',#27679);
#8515=VERTEX_POINT('',#27681);
#8516=VERTEX_POINT('',#27689);
#8517=VERTEX_POINT('',#27690);
#8518=VERTEX_POINT('',#27692);
#8519=VERTEX_POINT('',#27694);
#8520=VERTEX_POINT('',#27698);
#8521=VERTEX_POINT('',#27700);
#8522=VERTEX_POINT('',#27704);
#8523=VERTEX_POINT('',#27706);
#8524=VERTEX_POINT('',#27714);
#8525=VERTEX_POINT('',#27715);
#8526=VERTEX_POINT('',#27717);
#8527=VERTEX_POINT('',#27719);
#8528=VERTEX_POINT('',#27723);
#8529=VERTEX_POINT('',#27725);
#8530=VERTEX_POINT('',#27729);
#8531=VERTEX_POINT('',#27731);
#8532=VERTEX_POINT('',#27739);
#8533=VERTEX_POINT('',#27740);
#8534=VERTEX_POINT('',#27742);
#8535=VERTEX_POINT('',#27744);
#8536=VERTEX_POINT('',#27748);
#8537=VERTEX_POINT('',#27750);
#8538=VERTEX_POINT('',#27754);
#8539=VERTEX_POINT('',#27756);
#8540=VERTEX_POINT('',#27764);
#8541=VERTEX_POINT('',#27765);
#8542=VERTEX_POINT('',#27767);
#8543=VERTEX_POINT('',#27769);
#8544=VERTEX_POINT('',#27773);
#8545=VERTEX_POINT('',#27775);
#8546=VERTEX_POINT('',#27779);
#8547=VERTEX_POINT('',#27781);
#8548=VERTEX_POINT('',#27789);
#8549=VERTEX_POINT('',#27790);
#8550=VERTEX_POINT('',#27792);
#8551=VERTEX_POINT('',#27794);
#8552=VERTEX_POINT('',#27798);
#8553=VERTEX_POINT('',#27800);
#8554=VERTEX_POINT('',#27804);
#8555=VERTEX_POINT('',#27806);
#8556=VERTEX_POINT('',#27814);
#8557=VERTEX_POINT('',#27815);
#8558=VERTEX_POINT('',#27817);
#8559=VERTEX_POINT('',#27819);
#8560=VERTEX_POINT('',#27823);
#8561=VERTEX_POINT('',#27825);
#8562=VERTEX_POINT('',#27829);
#8563=VERTEX_POINT('',#27831);
#8564=VERTEX_POINT('',#27839);
#8565=VERTEX_POINT('',#27840);
#8566=VERTEX_POINT('',#27842);
#8567=VERTEX_POINT('',#27844);
#8568=VERTEX_POINT('',#27848);
#8569=VERTEX_POINT('',#27850);
#8570=VERTEX_POINT('',#27854);
#8571=VERTEX_POINT('',#27856);
#8572=VERTEX_POINT('',#27864);
#8573=VERTEX_POINT('',#27865);
#8574=VERTEX_POINT('',#27867);
#8575=VERTEX_POINT('',#27869);
#8576=VERTEX_POINT('',#27873);
#8577=VERTEX_POINT('',#27875);
#8578=VERTEX_POINT('',#27879);
#8579=VERTEX_POINT('',#27881);
#8580=VERTEX_POINT('',#27889);
#8581=VERTEX_POINT('',#27890);
#8582=VERTEX_POINT('',#27892);
#8583=VERTEX_POINT('',#27894);
#8584=VERTEX_POINT('',#27898);
#8585=VERTEX_POINT('',#27900);
#8586=VERTEX_POINT('',#27904);
#8587=VERTEX_POINT('',#27906);
#8588=VERTEX_POINT('',#27914);
#8589=VERTEX_POINT('',#27915);
#8590=VERTEX_POINT('',#27917);
#8591=VERTEX_POINT('',#27919);
#8592=VERTEX_POINT('',#27923);
#8593=VERTEX_POINT('',#27925);
#8594=VERTEX_POINT('',#27929);
#8595=VERTEX_POINT('',#27931);
#8596=VERTEX_POINT('',#27939);
#8597=VERTEX_POINT('',#27940);
#8598=VERTEX_POINT('',#27942);
#8599=VERTEX_POINT('',#27944);
#8600=VERTEX_POINT('',#27948);
#8601=VERTEX_POINT('',#27950);
#8602=VERTEX_POINT('',#27954);
#8603=VERTEX_POINT('',#27956);
#8604=VERTEX_POINT('',#27964);
#8605=VERTEX_POINT('',#27965);
#8606=VERTEX_POINT('',#27967);
#8607=VERTEX_POINT('',#27969);
#8608=VERTEX_POINT('',#27973);
#8609=VERTEX_POINT('',#27975);
#8610=VERTEX_POINT('',#27979);
#8611=VERTEX_POINT('',#27981);
#8612=VERTEX_POINT('',#27989);
#8613=VERTEX_POINT('',#27990);
#8614=VERTEX_POINT('',#27992);
#8615=VERTEX_POINT('',#27994);
#8616=VERTEX_POINT('',#27998);
#8617=VERTEX_POINT('',#28000);
#8618=VERTEX_POINT('',#28004);
#8619=VERTEX_POINT('',#28006);
#8620=VERTEX_POINT('',#28014);
#8621=VERTEX_POINT('',#28015);
#8622=VERTEX_POINT('',#28017);
#8623=VERTEX_POINT('',#28019);
#8624=VERTEX_POINT('',#28023);
#8625=VERTEX_POINT('',#28025);
#8626=VERTEX_POINT('',#28029);
#8627=VERTEX_POINT('',#28031);
#8628=VERTEX_POINT('',#28039);
#8629=VERTEX_POINT('',#28040);
#8630=VERTEX_POINT('',#28042);
#8631=VERTEX_POINT('',#28044);
#8632=VERTEX_POINT('',#28048);
#8633=VERTEX_POINT('',#28050);
#8634=VERTEX_POINT('',#28054);
#8635=VERTEX_POINT('',#28056);
#8636=VERTEX_POINT('',#28064);
#8637=VERTEX_POINT('',#28065);
#8638=VERTEX_POINT('',#28067);
#8639=VERTEX_POINT('',#28069);
#8640=VERTEX_POINT('',#28073);
#8641=VERTEX_POINT('',#28075);
#8642=VERTEX_POINT('',#28079);
#8643=VERTEX_POINT('',#28081);
#8644=VERTEX_POINT('',#28089);
#8645=VERTEX_POINT('',#28090);
#8646=VERTEX_POINT('',#28092);
#8647=VERTEX_POINT('',#28094);
#8648=VERTEX_POINT('',#28098);
#8649=VERTEX_POINT('',#28100);
#8650=VERTEX_POINT('',#28104);
#8651=VERTEX_POINT('',#28106);
#8652=VERTEX_POINT('',#28114);
#8653=VERTEX_POINT('',#28115);
#8654=VERTEX_POINT('',#28117);
#8655=VERTEX_POINT('',#28119);
#8656=VERTEX_POINT('',#28123);
#8657=VERTEX_POINT('',#28125);
#8658=VERTEX_POINT('',#28129);
#8659=VERTEX_POINT('',#28131);
#8660=VERTEX_POINT('',#28139);
#8661=VERTEX_POINT('',#28140);
#8662=VERTEX_POINT('',#28142);
#8663=VERTEX_POINT('',#28144);
#8664=VERTEX_POINT('',#28148);
#8665=VERTEX_POINT('',#28150);
#8666=VERTEX_POINT('',#28154);
#8667=VERTEX_POINT('',#28156);
#8668=VERTEX_POINT('',#28164);
#8669=VERTEX_POINT('',#28165);
#8670=VERTEX_POINT('',#28167);
#8671=VERTEX_POINT('',#28169);
#8672=VERTEX_POINT('',#28173);
#8673=VERTEX_POINT('',#28175);
#8674=VERTEX_POINT('',#28179);
#8675=VERTEX_POINT('',#28181);
#8676=VERTEX_POINT('',#28189);
#8677=VERTEX_POINT('',#28190);
#8678=VERTEX_POINT('',#28192);
#8679=VERTEX_POINT('',#28194);
#8680=VERTEX_POINT('',#28198);
#8681=VERTEX_POINT('',#28200);
#8682=VERTEX_POINT('',#28204);
#8683=VERTEX_POINT('',#28206);
#8684=VERTEX_POINT('',#28214);
#8685=VERTEX_POINT('',#28215);
#8686=VERTEX_POINT('',#28217);
#8687=VERTEX_POINT('',#28219);
#8688=VERTEX_POINT('',#28223);
#8689=VERTEX_POINT('',#28225);
#8690=VERTEX_POINT('',#28229);
#8691=VERTEX_POINT('',#28231);
#8692=VERTEX_POINT('',#28239);
#8693=VERTEX_POINT('',#28241);
#8694=VERTEX_POINT('',#28245);
#8695=VERTEX_POINT('',#28247);
#8696=VERTEX_POINT('',#28251);
#8697=VERTEX_POINT('',#28252);
#8698=VERTEX_POINT('',#28254);
#8699=VERTEX_POINT('',#28256);
#8700=VERTEX_POINT('',#28260);
#8701=VERTEX_POINT('',#28262);
#8702=VERTEX_POINT('',#28266);
#8703=VERTEX_POINT('',#28268);
#8704=VERTEX_POINT('',#28278);
#8705=VERTEX_POINT('',#28280);
#8706=VERTEX_POINT('',#28284);
#8707=VERTEX_POINT('',#28289);
#8708=VERTEX_POINT('',#28295);
#8709=VERTEX_POINT('',#28296);
#8710=VERTEX_POINT('',#28300);
#8711=VERTEX_POINT('',#28302);
#8712=VERTEX_POINT('',#28306);
#8713=VERTEX_POINT('',#28307);
#8714=VERTEX_POINT('',#28309);
#8715=VERTEX_POINT('',#28311);
#8716=VERTEX_POINT('',#28317);
#8717=VERTEX_POINT('',#28319);
#8718=VERTEX_POINT('',#28321);
#8719=VERTEX_POINT('',#28323);
#8720=VERTEX_POINT('',#28326);
#8721=VERTEX_POINT('',#28329);
#8722=VERTEX_POINT('',#28331);
#8723=VERTEX_POINT('',#28334);
#8724=VERTEX_POINT('',#28337);
#8725=VERTEX_POINT('',#28338);
#8726=VERTEX_POINT('',#28340);
#8727=VERTEX_POINT('',#28343);
#8728=VERTEX_POINT('',#28346);
#8729=VERTEX_POINT('',#28349);
#8730=VERTEX_POINT('',#28351);
#8731=VERTEX_POINT('',#28355);
#8732=VERTEX_POINT('',#28359);
#8733=VERTEX_POINT('',#28363);
#8734=VERTEX_POINT('',#28367);
#8735=VERTEX_POINT('',#28369);
#8736=VERTEX_POINT('',#28373);
#8737=VERTEX_POINT('',#28375);
#8738=VERTEX_POINT('',#28378);
#8739=VERTEX_POINT('',#28380);
#8740=VERTEX_POINT('',#28382);
#8741=VERTEX_POINT('',#28384);
#8742=VERTEX_POINT('',#28386);
#8743=VERTEX_POINT('',#28390);
#8744=VERTEX_POINT('',#28394);
#8745=VERTEX_POINT('',#28400);
#8746=VERTEX_POINT('',#28404);
#8747=VERTEX_POINT('',#28408);
#8748=VERTEX_POINT('',#28412);
#8749=VERTEX_POINT('',#28416);
#8750=VERTEX_POINT('',#28424);
#8751=VERTEX_POINT('',#28425);
#8752=VERTEX_POINT('',#28427);
#8753=VERTEX_POINT('',#28429);
#8754=VERTEX_POINT('',#28433);
#8755=VERTEX_POINT('',#28435);
#8756=VERTEX_POINT('',#28439);
#8757=VERTEX_POINT('',#28441);
#8758=VERTEX_POINT('',#28445);
#8759=VERTEX_POINT('',#28447);
#8760=VERTEX_POINT('',#28451);
#8761=VERTEX_POINT('',#28453);
#8762=VERTEX_POINT('',#28462);
#8763=VERTEX_POINT('',#28465);
#8764=VERTEX_POINT('',#28468);
#8765=VERTEX_POINT('',#28472);
#8766=VERTEX_POINT('',#28476);
#8767=VERTEX_POINT('',#28480);
#8768=VERTEX_POINT('',#28483);
#8769=VERTEX_POINT('',#28491);
#8770=VERTEX_POINT('',#28492);
#8771=VERTEX_POINT('',#28495);
#8772=VERTEX_POINT('',#28497);
#8773=VERTEX_POINT('',#28501);
#8774=VERTEX_POINT('',#28505);
#8775=VERTEX_POINT('',#28507);
#8776=VERTEX_POINT('',#28511);
#8777=VERTEX_POINT('',#28516);
#8778=VERTEX_POINT('',#28520);
#8779=VERTEX_POINT('',#28526);
#8780=VERTEX_POINT('',#28527);
#8781=VERTEX_POINT('',#28530);
#8782=VERTEX_POINT('',#28532);
#8783=VERTEX_POINT('',#28536);
#8784=VERTEX_POINT('',#28540);
#8785=VERTEX_POINT('',#28542);
#8786=VERTEX_POINT('',#28545);
#8787=VERTEX_POINT('',#28549);
#8788=VERTEX_POINT('',#28553);
#8789=VERTEX_POINT('',#28561);
#8790=VERTEX_POINT('',#28562);
#8791=VERTEX_POINT('',#28565);
#8792=VERTEX_POINT('',#28566);
#8793=VERTEX_POINT('',#28569);
#8794=VERTEX_POINT('',#28570);
#8795=VERTEX_POINT('',#28573);
#8796=VERTEX_POINT('',#28574);
#8797=VERTEX_POINT('',#28577);
#8798=VERTEX_POINT('',#28578);
#8799=VERTEX_POINT('',#28581);
#8800=VERTEX_POINT('',#28582);
#8801=VERTEX_POINT('',#28585);
#8802=VERTEX_POINT('',#28586);
#8803=VERTEX_POINT('',#28590);
#8804=VERTEX_POINT('',#28591);
#8805=VERTEX_POINT('',#28614);
#8806=VERTEX_POINT('',#28616);
#8807=VERTEX_POINT('',#28641);
#8808=VERTEX_POINT('',#28643);
#8809=VERTEX_POINT('',#28666);
#8810=VERTEX_POINT('',#28668);
#8811=VERTEX_POINT('',#28691);
#8812=VERTEX_POINT('',#28693);
#8813=VERTEX_POINT('',#28696);
#8814=VERTEX_POINT('',#28698);
#8815=VERTEX_POINT('',#28721);
#8816=VERTEX_POINT('',#28723);
#8817=VERTEX_POINT('',#28746);
#8818=VERTEX_POINT('',#28748);
#8819=VERTEX_POINT('',#28771);
#8820=VERTEX_POINT('',#28773);
#8821=VERTEX_POINT('',#28798);
#8822=VERTEX_POINT('',#28802);
#8823=VERTEX_POINT('',#28827);
#8824=VERTEX_POINT('',#28831);
#8825=VERTEX_POINT('',#28856);
#8826=VERTEX_POINT('',#28858);
#8827=VERTEX_POINT('',#28862);
#8828=VERTEX_POINT('',#28887);
#8829=VERTEX_POINT('',#28891);
#8830=VERTEX_POINT('',#28916);
#8831=VERTEX_POINT('',#28920);
#8832=VERTEX_POINT('',#28945);
#8833=VERTEX_POINT('',#28948);
#8834=VERTEX_POINT('',#28950);
#8835=VERTEX_POINT('',#28982);
#8836=VERTEX_POINT('',#28984);
#8837=VERTEX_POINT('',#28987);
#8838=VERTEX_POINT('',#28991);
#8839=VERTEX_POINT('',#28996);
#8840=VERTEX_POINT('',#28998);
#8841=VERTEX_POINT('',#29001);
#8842=VERTEX_POINT('',#29005);
#8843=VERTEX_POINT('',#29017);
#8844=VERTEX_POINT('',#29018);
#8845=VERTEX_POINT('',#29021);
#8846=VERTEX_POINT('',#29023);
#8847=VERTEX_POINT('',#29027);
#8848=VERTEX_POINT('',#29031);
#8849=VERTEX_POINT('',#29033);
#8850=VERTEX_POINT('',#29037);
#8851=VERTEX_POINT('',#29042);
#8852=VERTEX_POINT('',#29046);
#8853=VERTEX_POINT('',#29052);
#8854=VERTEX_POINT('',#29053);
#8855=VERTEX_POINT('',#29056);
#8856=VERTEX_POINT('',#29058);
#8857=VERTEX_POINT('',#29062);
#8858=VERTEX_POINT('',#29066);
#8859=VERTEX_POINT('',#29068);
#8860=VERTEX_POINT('',#29071);
#8861=VERTEX_POINT('',#29075);
#8862=VERTEX_POINT('',#29079);
#8863=VERTEX_POINT('',#29087);
#8864=VERTEX_POINT('',#29088);
#8865=VERTEX_POINT('',#29091);
#8866=VERTEX_POINT('',#29092);
#8867=VERTEX_POINT('',#29095);
#8868=VERTEX_POINT('',#29096);
#8869=VERTEX_POINT('',#29099);
#8870=VERTEX_POINT('',#29100);
#8871=VERTEX_POINT('',#29103);
#8872=VERTEX_POINT('',#29104);
#8873=VERTEX_POINT('',#29107);
#8874=VERTEX_POINT('',#29108);
#8875=VERTEX_POINT('',#29111);
#8876=VERTEX_POINT('',#29112);
#8877=VERTEX_POINT('',#29115);
#8878=VERTEX_POINT('',#29116);
#8879=VERTEX_POINT('',#29120);
#8880=VERTEX_POINT('',#29121);
#8881=VERTEX_POINT('',#29144);
#8882=VERTEX_POINT('',#29146);
#8883=VERTEX_POINT('',#29171);
#8884=VERTEX_POINT('',#29173);
#8885=VERTEX_POINT('',#29196);
#8886=VERTEX_POINT('',#29198);
#8887=VERTEX_POINT('',#29221);
#8888=VERTEX_POINT('',#29223);
#8889=VERTEX_POINT('',#29236);
#8890=VERTEX_POINT('',#29239);
#8891=VERTEX_POINT('',#29252);
#8892=VERTEX_POINT('',#29254);
#8893=VERTEX_POINT('',#29277);
#8894=VERTEX_POINT('',#29279);
#8895=VERTEX_POINT('',#29302);
#8896=VERTEX_POINT('',#29304);
#8897=VERTEX_POINT('',#29327);
#8898=VERTEX_POINT('',#29329);
#8899=VERTEX_POINT('',#29354);
#8900=VERTEX_POINT('',#29358);
#8901=VERTEX_POINT('',#29383);
#8902=VERTEX_POINT('',#29387);
#8903=VERTEX_POINT('',#29412);
#8904=VERTEX_POINT('',#29416);
#8905=VERTEX_POINT('',#29417);
#8906=VERTEX_POINT('',#29444);
#8907=VERTEX_POINT('',#29448);
#8908=VERTEX_POINT('',#29473);
#8909=VERTEX_POINT('',#29477);
#8910=VERTEX_POINT('',#29502);
#8911=VERTEX_POINT('',#29506);
#8912=VERTEX_POINT('',#29531);
#8913=VERTEX_POINT('',#29534);
#8914=VERTEX_POINT('',#29536);
#8915=VERTEX_POINT('',#29568);
#8916=VERTEX_POINT('',#29570);
#8917=VERTEX_POINT('',#29573);
#8918=VERTEX_POINT('',#29577);
#8919=VERTEX_POINT('',#29582);
#8920=VERTEX_POINT('',#29584);
#8921=VERTEX_POINT('',#29587);
#8922=VERTEX_POINT('',#29591);
#8923=VERTEX_POINT('',#29602);
#8924=VERTEX_POINT('',#29605);
#8925=VERTEX_POINT('',#29607);
#8926=VERTEX_POINT('',#29612);
#8927=VERTEX_POINT('',#29615);
#8928=VERTEX_POINT('',#29619);
#8929=VERTEX_POINT('',#29623);
#8930=VERTEX_POINT('',#29627);
#8931=VERTEX_POINT('',#29630);
#8932=VERTEX_POINT('',#29636);
#8933=VERTEX_POINT('',#29637);
#8934=VERTEX_POINT('',#29639);
#8935=VERTEX_POINT('',#29641);
#8936=VERTEX_POINT('',#29645);
#8937=VERTEX_POINT('',#29647);
#8938=VERTEX_POINT('',#29651);
#8939=VERTEX_POINT('',#29653);
#8940=VERTEX_POINT('',#29657);
#8941=VERTEX_POINT('',#29659);
#8942=VERTEX_POINT('',#29663);
#8943=VERTEX_POINT('',#29665);
#8944=VERTEX_POINT('',#29675);
#8945=VERTEX_POINT('',#29676);
#8946=VERTEX_POINT('',#29678);
#8947=VERTEX_POINT('',#29680);
#8948=VERTEX_POINT('',#29684);
#8949=VERTEX_POINT('',#29686);
#8950=VERTEX_POINT('',#29690);
#8951=VERTEX_POINT('',#29692);
#8952=VERTEX_POINT('',#29696);
#8953=VERTEX_POINT('',#29698);
#8954=VERTEX_POINT('',#29702);
#8955=VERTEX_POINT('',#29704);
#8956=VERTEX_POINT('',#29713);
#8957=VERTEX_POINT('',#29716);
#8958=VERTEX_POINT('',#29719);
#8959=VERTEX_POINT('',#29723);
#8960=VERTEX_POINT('',#29727);
#8961=VERTEX_POINT('',#29731);
#8962=VERTEX_POINT('',#29734);
#8963=VERTEX_POINT('',#29741);
#8964=VERTEX_POINT('',#29742);
#8965=VERTEX_POINT('',#29744);
#8966=VERTEX_POINT('',#29746);
#8967=VERTEX_POINT('',#29750);
#8968=VERTEX_POINT('',#29752);
#8969=VERTEX_POINT('',#29756);
#8970=VERTEX_POINT('',#29758);
#8971=VERTEX_POINT('',#29762);
#8972=VERTEX_POINT('',#29764);
#8973=VERTEX_POINT('',#29768);
#8974=VERTEX_POINT('',#29770);
#8975=VERTEX_POINT('',#29774);
#8976=VERTEX_POINT('',#29776);
#8977=VERTEX_POINT('',#29780);
#8978=VERTEX_POINT('',#29782);
#8979=VERTEX_POINT('',#29786);
#8980=VERTEX_POINT('',#29788);
#8981=VERTEX_POINT('',#29792);
#8982=VERTEX_POINT('',#29794);
#8983=VERTEX_POINT('',#29798);
#8984=VERTEX_POINT('',#29799);
#8985=VERTEX_POINT('',#29801);
#8986=VERTEX_POINT('',#29803);
#8987=VERTEX_POINT('',#29807);
#8988=VERTEX_POINT('',#29809);
#8989=VERTEX_POINT('',#29813);
#8990=VERTEX_POINT('',#29815);
#8991=VERTEX_POINT('',#29819);
#8992=VERTEX_POINT('',#29821);
#8993=VERTEX_POINT('',#29825);
#8994=VERTEX_POINT('',#29827);
#8995=VERTEX_POINT('',#29831);
#8996=VERTEX_POINT('',#29833);
#8997=VERTEX_POINT('',#29837);
#8998=VERTEX_POINT('',#29839);
#8999=VERTEX_POINT('',#29843);
#9000=VERTEX_POINT('',#29845);
#9001=VERTEX_POINT('',#29849);
#9002=VERTEX_POINT('',#29851);
#9003=VERTEX_POINT('',#29855);
#9004=VERTEX_POINT('',#29856);
#9005=VERTEX_POINT('',#29858);
#9006=VERTEX_POINT('',#29860);
#9007=VERTEX_POINT('',#29864);
#9008=VERTEX_POINT('',#29866);
#9009=VERTEX_POINT('',#29870);
#9010=VERTEX_POINT('',#29872);
#9011=VERTEX_POINT('',#29876);
#9012=VERTEX_POINT('',#29878);
#9013=VERTEX_POINT('',#29882);
#9014=VERTEX_POINT('',#29884);
#9015=VERTEX_POINT('',#29888);
#9016=VERTEX_POINT('',#29890);
#9017=VERTEX_POINT('',#29894);
#9018=VERTEX_POINT('',#29896);
#9019=VERTEX_POINT('',#29900);
#9020=VERTEX_POINT('',#29902);
#9021=VERTEX_POINT('',#29906);
#9022=VERTEX_POINT('',#29908);
#9023=VERTEX_POINT('',#29912);
#9024=VERTEX_POINT('',#29913);
#9025=VERTEX_POINT('',#29915);
#9026=VERTEX_POINT('',#29917);
#9027=VERTEX_POINT('',#29921);
#9028=VERTEX_POINT('',#29923);
#9029=VERTEX_POINT('',#29927);
#9030=VERTEX_POINT('',#29929);
#9031=VERTEX_POINT('',#29933);
#9032=VERTEX_POINT('',#29935);
#9033=VERTEX_POINT('',#29939);
#9034=VERTEX_POINT('',#29941);
#9035=VERTEX_POINT('',#29945);
#9036=VERTEX_POINT('',#29947);
#9037=VERTEX_POINT('',#29951);
#9038=VERTEX_POINT('',#29953);
#9039=VERTEX_POINT('',#29957);
#9040=VERTEX_POINT('',#29959);
#9041=VERTEX_POINT('',#29963);
#9042=VERTEX_POINT('',#29965);
#9043=VERTEX_POINT('',#29969);
#9044=VERTEX_POINT('',#29971);
#9045=VERTEX_POINT('',#29975);
#9046=VERTEX_POINT('',#29977);
#9047=VERTEX_POINT('',#29981);
#9048=VERTEX_POINT('',#29983);
#9049=VERTEX_POINT('',#29990);
#9050=VERTEX_POINT('',#29992);
#9051=VERTEX_POINT('',#29999);
#9052=VERTEX_POINT('',#30001);
#9053=VERTEX_POINT('',#30014);
#9054=VERTEX_POINT('',#30017);
#9055=VERTEX_POINT('',#30021);
#9056=VERTEX_POINT('',#30025);
#9057=VERTEX_POINT('',#30029);
#9058=VERTEX_POINT('',#30032);
#9059=VERTEX_POINT('',#30036);
#9060=VERTEX_POINT('',#30040);
#9061=VERTEX_POINT('',#30045);
#9062=VERTEX_POINT('',#30046);
#9063=VERTEX_POINT('',#30048);
#9064=VERTEX_POINT('',#30050);
#9065=VERTEX_POINT('',#30054);
#9066=VERTEX_POINT('',#30056);
#9067=VERTEX_POINT('',#30060);
#9068=VERTEX_POINT('',#30062);
#9069=VERTEX_POINT('',#30066);
#9070=VERTEX_POINT('',#30068);
#9071=VERTEX_POINT('',#30072);
#9072=VERTEX_POINT('',#30074);
#9073=VERTEX_POINT('',#30084);
#9074=VERTEX_POINT('',#30085);
#9075=VERTEX_POINT('',#30087);
#9076=VERTEX_POINT('',#30089);
#9077=VERTEX_POINT('',#30093);
#9078=VERTEX_POINT('',#30095);
#9079=VERTEX_POINT('',#30099);
#9080=VERTEX_POINT('',#30101);
#9081=VERTEX_POINT('',#30104);
#9082=VERTEX_POINT('',#30107);
#9083=VERTEX_POINT('',#30109);
#9084=VERTEX_POINT('',#30111);
#9085=VERTEX_POINT('',#30113);
#9086=VERTEX_POINT('',#30115);
#9087=VERTEX_POINT('',#30117);
#9088=VERTEX_POINT('',#30121);
#9089=VERTEX_POINT('',#30125);
#9090=VERTEX_POINT('',#30129);
#9091=VERTEX_POINT('',#30131);
#9092=VERTEX_POINT('',#30133);
#9093=VERTEX_POINT('',#30135);
#9094=VERTEX_POINT('',#30141);
#9095=VERTEX_POINT('',#30143);
#9096=VERTEX_POINT('',#30147);
#9097=VERTEX_POINT('',#30150);
#9098=VERTEX_POINT('',#30152);
#9099=VERTEX_POINT('',#30164);
#9100=VERTEX_POINT('',#30166);
#9101=VERTEX_POINT('',#30167);
#9102=VERTEX_POINT('',#30169);
#9103=VERTEX_POINT('',#30171);
#9104=VERTEX_POINT('',#30173);
#9105=VERTEX_POINT('',#30175);
#9106=VERTEX_POINT('',#30179);
#9107=VERTEX_POINT('',#30182);
#9108=VERTEX_POINT('',#30186);
#9109=VERTEX_POINT('',#30190);
#9110=VERTEX_POINT('',#30194);
#9111=VERTEX_POINT('',#30197);
#9112=VERTEX_POINT('',#30203);
#9113=VERTEX_POINT('',#30204);
#9114=VERTEX_POINT('',#30209);
#9115=VERTEX_POINT('',#30213);
#9116=VERTEX_POINT('',#30217);
#9117=VERTEX_POINT('',#30221);
#9118=VERTEX_POINT('',#30230);
#9119=VERTEX_POINT('',#30232);
#9120=VERTEX_POINT('',#30236);
#9121=VERTEX_POINT('',#30238);
#9122=VERTEX_POINT('',#30242);
#9123=VERTEX_POINT('',#30244);
#9124=VERTEX_POINT('',#30248);
#9125=VERTEX_POINT('',#30250);
#9126=VERTEX_POINT('',#30254);
#9127=VERTEX_POINT('',#30256);
#9128=VERTEX_POINT('',#30260);
#9129=VERTEX_POINT('',#30262);
#9130=VERTEX_POINT('',#30266);
#9131=VERTEX_POINT('',#30268);
#9132=VERTEX_POINT('',#30272);
#9133=VERTEX_POINT('',#30274);
#9134=VERTEX_POINT('',#30278);
#9135=VERTEX_POINT('',#30280);
#9136=VERTEX_POINT('',#30284);
#9137=VERTEX_POINT('',#30286);
#9138=VERTEX_POINT('',#30290);
#9139=VERTEX_POINT('',#30292);
#9140=VERTEX_POINT('',#30296);
#9141=VERTEX_POINT('',#30298);
#9142=VERTEX_POINT('',#30302);
#9143=VERTEX_POINT('',#30304);
#9144=VERTEX_POINT('',#30308);
#9145=VERTEX_POINT('',#30310);
#9146=VERTEX_POINT('',#30314);
#9147=VERTEX_POINT('',#30316);
#9148=VERTEX_POINT('',#30320);
#9149=VERTEX_POINT('',#30322);
#9150=VERTEX_POINT('',#30326);
#9151=VERTEX_POINT('',#30328);
#9152=VERTEX_POINT('',#30332);
#9153=VERTEX_POINT('',#30334);
#9154=VERTEX_POINT('',#30338);
#9155=VERTEX_POINT('',#30339);
#9156=VERTEX_POINT('',#30341);
#9157=VERTEX_POINT('',#30343);
#9158=VERTEX_POINT('',#30347);
#9159=VERTEX_POINT('',#30349);
#9160=VERTEX_POINT('',#30353);
#9161=VERTEX_POINT('',#30355);
#9162=VERTEX_POINT('',#30365);
#9163=VERTEX_POINT('',#30366);
#9164=VERTEX_POINT('',#30370);
#9165=VERTEX_POINT('',#30372);
#9166=VERTEX_POINT('',#30374);
#9167=VERTEX_POINT('',#30377);
#9168=VERTEX_POINT('',#30381);
#9169=VERTEX_POINT('',#30382);
#9170=VERTEX_POINT('',#30386);
#9171=VERTEX_POINT('',#30388);
#9172=VERTEX_POINT('',#30390);
#9173=VERTEX_POINT('',#30393);
#9174=VERTEX_POINT('',#30397);
#9175=VERTEX_POINT('',#30398);
#9176=VERTEX_POINT('',#30400);
#9177=VERTEX_POINT('',#30404);
#9178=VERTEX_POINT('',#30406);
#9179=VERTEX_POINT('',#30409);
#9180=VERTEX_POINT('',#30413);
#9181=VERTEX_POINT('',#30414);
#9182=VERTEX_POINT('',#30416);
#9183=VERTEX_POINT('',#30420);
#9184=VERTEX_POINT('',#30422);
#9185=VERTEX_POINT('',#30425);
#9186=VERTEX_POINT('',#30429);
#9187=VERTEX_POINT('',#30431);
#9188=VERTEX_POINT('',#30439);
#9189=VERTEX_POINT('',#30441);
#9190=VERTEX_POINT('',#30445);
#9191=VERTEX_POINT('',#30448);
#9192=VERTEX_POINT('',#30451);
#9193=VERTEX_POINT('',#30455);
#9194=VERTEX_POINT('',#30462);
#9195=VERTEX_POINT('',#30463);
#9196=VERTEX_POINT('',#30467);
#9197=VERTEX_POINT('',#30469);
#9198=VERTEX_POINT('',#30471);
#9199=VERTEX_POINT('',#30474);
#9200=VERTEX_POINT('',#30478);
#9201=VERTEX_POINT('',#30479);
#9202=VERTEX_POINT('',#30483);
#9203=VERTEX_POINT('',#30485);
#9204=VERTEX_POINT('',#30487);
#9205=VERTEX_POINT('',#30490);
#9206=VERTEX_POINT('',#30494);
#9207=VERTEX_POINT('',#30495);
#9208=VERTEX_POINT('',#30497);
#9209=VERTEX_POINT('',#30501);
#9210=VERTEX_POINT('',#30503);
#9211=VERTEX_POINT('',#30506);
#9212=VERTEX_POINT('',#30510);
#9213=VERTEX_POINT('',#30511);
#9214=VERTEX_POINT('',#30513);
#9215=VERTEX_POINT('',#30517);
#9216=VERTEX_POINT('',#30519);
#9217=VERTEX_POINT('',#30522);
#9218=VERTEX_POINT('',#30526);
#9219=VERTEX_POINT('',#30528);
#9220=VERTEX_POINT('',#30536);
#9221=VERTEX_POINT('',#30538);
#9222=VERTEX_POINT('',#30542);
#9223=VERTEX_POINT('',#30545);
#9224=VERTEX_POINT('',#30548);
#9225=VERTEX_POINT('',#30552);
#9226=VERTEX_POINT('',#30559);
#9227=VERTEX_POINT('',#30561);
#9228=VERTEX_POINT('',#30566);
#9229=VERTEX_POINT('',#30568);
#9230=VERTEX_POINT('',#30573);
#9231=VERTEX_POINT('',#30575);
#9232=VERTEX_POINT('',#30580);
#9233=VERTEX_POINT('',#30582);
#9234=VERTEX_POINT('',#30586);
#9235=VERTEX_POINT('',#30588);
#9236=VERTEX_POINT('',#30595);
#9237=VERTEX_POINT('',#30597);
#9238=VERTEX_POINT('',#30601);
#9239=VERTEX_POINT('',#30603);
#9240=VERTEX_POINT('',#30607);
#9241=VERTEX_POINT('',#30609);
#9242=VERTEX_POINT('',#30616);
#9243=VERTEX_POINT('',#30618);
#9244=VERTEX_POINT('',#30622);
#9245=VERTEX_POINT('',#30624);
#9246=VERTEX_POINT('',#30628);
#9247=VERTEX_POINT('',#30629);
#9248=VERTEX_POINT('',#30631);
#9249=VERTEX_POINT('',#30633);
#9250=VERTEX_POINT('',#30637);
#9251=VERTEX_POINT('',#30639);
#9252=VERTEX_POINT('',#30645);
#9253=VERTEX_POINT('',#30646);
#9254=VERTEX_POINT('',#30648);
#9255=VERTEX_POINT('',#30650);
#9256=VERTEX_POINT('',#30654);
#9257=VERTEX_POINT('',#30656);
#9258=VERTEX_POINT('',#30660);
#9259=VERTEX_POINT('',#30662);
#9260=VERTEX_POINT('',#30668);
#9261=VERTEX_POINT('',#30670);
#9262=VERTEX_POINT('',#30672);
#9263=VERTEX_POINT('',#30674);
#9264=VERTEX_POINT('',#30678);
#9265=VERTEX_POINT('',#30680);
#9266=VERTEX_POINT('',#30684);
#9267=VERTEX_POINT('',#30686);
#9268=VERTEX_POINT('',#30698);
#9269=VERTEX_POINT('',#30699);
#9270=VERTEX_POINT('',#30701);
#9271=VERTEX_POINT('',#30703);
#9272=VERTEX_POINT('',#30707);
#9273=VERTEX_POINT('',#30709);
#9274=VERTEX_POINT('',#30713);
#9275=VERTEX_POINT('',#30715);
#9276=VERTEX_POINT('',#30723);
#9277=VERTEX_POINT('',#30725);
#9278=VERTEX_POINT('',#30728);
#9279=VERTEX_POINT('',#30732);
#9280=VERTEX_POINT('',#30735);
#9281=VERTEX_POINT('',#30739);
#9282=VERTEX_POINT('',#30742);
#9283=VERTEX_POINT('',#30746);
#9284=VERTEX_POINT('',#30749);
#9285=VERTEX_POINT('',#30753);
#9286=VERTEX_POINT('',#30756);
#9287=VERTEX_POINT('',#30760);
#9288=VERTEX_POINT('',#30766);
#9289=VERTEX_POINT('',#30767);
#9290=VERTEX_POINT('',#30769);
#9291=VERTEX_POINT('',#30771);
#9292=VERTEX_POINT('',#30775);
#9293=VERTEX_POINT('',#30777);
#9294=VERTEX_POINT('',#30781);
#9295=VERTEX_POINT('',#30783);
#9296=VERTEX_POINT('',#30790);
#9297=VERTEX_POINT('',#30792);
#9298=VERTEX_POINT('',#30795);
#9299=VERTEX_POINT('',#30799);
#9300=VERTEX_POINT('',#30807);
#9301=VERTEX_POINT('',#30808);
#9302=VERTEX_POINT('',#30810);
#9303=VERTEX_POINT('',#30836);
#9304=VERTEX_POINT('',#30879);
#9305=VERTEX_POINT('',#30880);
#9306=VERTEX_POINT('',#30966);
#9307=VERTEX_POINT('',#30967);
#9308=VERTEX_POINT('',#31056);
#9309=VERTEX_POINT('',#31057);
#9310=VERTEX_POINT('',#31143);
#9311=VERTEX_POINT('',#31144);
#9312=VERTEX_POINT('',#31233);
#9313=VERTEX_POINT('',#31234);
#9314=VERTEX_POINT('',#31320);
#9315=VERTEX_POINT('',#31321);
#9316=VERTEX_POINT('',#31407);
#9317=VERTEX_POINT('',#31408);
#9318=VERTEX_POINT('',#31497);
#9319=VERTEX_POINT('',#31498);
#9320=VERTEX_POINT('',#31500);
#9321=VERTEX_POINT('',#31513);
#9322=VERTEX_POINT('',#31514);
#9323=VERTEX_POINT('',#31516);
#9324=VERTEX_POINT('',#31524);
#9325=VERTEX_POINT('',#31539);
#9326=VERTEX_POINT('',#31540);
#9327=VERTEX_POINT('',#31576);
#9328=VERTEX_POINT('',#31577);
#9329=VERTEX_POINT('',#31613);
#9330=VERTEX_POINT('',#31614);
#9331=VERTEX_POINT('',#31651);
#9332=VERTEX_POINT('',#31652);
#9333=VERTEX_POINT('',#31688);
#9334=VERTEX_POINT('',#31689);
#9335=VERTEX_POINT('',#31725);
#9336=VERTEX_POINT('',#31726);
#9337=VERTEX_POINT('',#31763);
#9338=VERTEX_POINT('',#31764);
#9339=VERTEX_POINT('',#31801);
#9340=VERTEX_POINT('',#31802);
#9341=VERTEX_POINT('',#31804);
#9342=VERTEX_POINT('',#31810);
#9343=VERTEX_POINT('',#32874);
#9344=VERTEX_POINT('',#32966);
#9345=VERTEX_POINT('',#32967);
#9346=VERTEX_POINT('',#32971);
#9347=VERTEX_POINT('',#32973);
#9348=VERTEX_POINT('',#32975);
#9349=VERTEX_POINT('',#32978);
#9350=VERTEX_POINT('',#32982);
#9351=VERTEX_POINT('',#32986);
#9352=VERTEX_POINT('',#32990);
#9353=VERTEX_POINT('',#32991);
#9354=VERTEX_POINT('',#32997);
#9355=VERTEX_POINT('',#33002);
#9356=VERTEX_POINT('',#33008);
#9357=VERTEX_POINT('',#33009);
#9358=VERTEX_POINT('',#33011);
#9359=VERTEX_POINT('',#33013);
#9360=VERTEX_POINT('',#33017);
#9361=VERTEX_POINT('',#33019);
#9362=VERTEX_POINT('',#33023);
#9363=VERTEX_POINT('',#33025);
#9364=VERTEX_POINT('',#33029);
#9365=VERTEX_POINT('',#33031);
#9366=VERTEX_POINT('',#33035);
#9367=VERTEX_POINT('',#33037);
#9368=VERTEX_POINT('',#33046);
#9369=VERTEX_POINT('',#33048);
#9370=VERTEX_POINT('',#33051);
#9371=VERTEX_POINT('',#33056);
#9372=VERTEX_POINT('',#33059);
#9373=VERTEX_POINT('',#33063);
#9374=VERTEX_POINT('',#33067);
#9375=VERTEX_POINT('',#33071);
#9376=VERTEX_POINT('',#33074);
#9377=VERTEX_POINT('',#33081);
#9378=VERTEX_POINT('',#33084);
#9379=VERTEX_POINT('',#33088);
#9380=VERTEX_POINT('',#33092);
#9381=VERTEX_POINT('',#33096);
#9382=VERTEX_POINT('',#33099);
#9383=VERTEX_POINT('',#33103);
#9384=VERTEX_POINT('',#33107);
#9385=VERTEX_POINT('',#33112);
#9386=VERTEX_POINT('',#33113);
#9387=VERTEX_POINT('',#33115);
#9388=VERTEX_POINT('',#33117);
#9389=VERTEX_POINT('',#33121);
#9390=VERTEX_POINT('',#33123);
#9391=VERTEX_POINT('',#33127);
#9392=VERTEX_POINT('',#33129);
#9393=VERTEX_POINT('',#33133);
#9394=VERTEX_POINT('',#33135);
#9395=VERTEX_POINT('',#33139);
#9396=VERTEX_POINT('',#33141);
#9397=VERTEX_POINT('',#33260);
#9398=VERTEX_POINT('',#33261);
#9399=VERTEX_POINT('',#33263);
#9400=VERTEX_POINT('',#33283);
#9401=VERTEX_POINT('',#33290);
#9402=VERTEX_POINT('',#33291);
#9403=VERTEX_POINT('',#33377);
#9404=VERTEX_POINT('',#33378);
#9405=VERTEX_POINT('',#33467);
#9406=VERTEX_POINT('',#33468);
#9407=VERTEX_POINT('',#33554);
#9408=VERTEX_POINT('',#33555);
#9409=VERTEX_POINT('',#33641);
#9410=VERTEX_POINT('',#33642);
#9411=VERTEX_POINT('',#33728);
#9412=VERTEX_POINT('',#33729);
#9413=VERTEX_POINT('',#33815);
#9414=VERTEX_POINT('',#33816);
#9415=VERTEX_POINT('',#33902);
#9416=VERTEX_POINT('',#33903);
#9417=VERTEX_POINT('',#33974);
#9418=VERTEX_POINT('',#33975);
#9419=VERTEX_POINT('',#34025);
#9420=VERTEX_POINT('',#34026);
#9421=VERTEX_POINT('',#34073);
#9422=VERTEX_POINT('',#34074);
#9423=VERTEX_POINT('',#34121);
#9424=VERTEX_POINT('',#34122);
#9425=VERTEX_POINT('',#34172);
#9426=VERTEX_POINT('',#34173);
#9427=VERTEX_POINT('',#34223);
#9428=VERTEX_POINT('',#34224);
#9429=VERTEX_POINT('',#34271);
#9430=VERTEX_POINT('',#34272);
#9431=VERTEX_POINT('',#34322);
#9432=VERTEX_POINT('',#34323);
#9433=VERTEX_POINT('',#34373);
#9434=VERTEX_POINT('',#34374);
#9435=VERTEX_POINT('',#34421);
#9436=VERTEX_POINT('',#34422);
#9437=VERTEX_POINT('',#34469);
#9438=VERTEX_POINT('',#34470);
#9439=VERTEX_POINT('',#34520);
#9440=VERTEX_POINT('',#34521);
#9441=VERTEX_POINT('',#34571);
#9442=VERTEX_POINT('',#34572);
#9443=VERTEX_POINT('',#34619);
#9444=VERTEX_POINT('',#34620);
#9445=VERTEX_POINT('',#34670);
#9446=VERTEX_POINT('',#34671);
#9447=VERTEX_POINT('',#34721);
#9448=VERTEX_POINT('',#34722);
#9449=VERTEX_POINT('',#34769);
#9450=VERTEX_POINT('',#34770);
#9451=VERTEX_POINT('',#34817);
#9452=VERTEX_POINT('',#34818);
#9453=VERTEX_POINT('',#34868);
#9454=VERTEX_POINT('',#34869);
#9455=VERTEX_POINT('',#34919);
#9456=VERTEX_POINT('',#34920);
#9457=VERTEX_POINT('',#34967);
#9458=VERTEX_POINT('',#34968);
#9459=VERTEX_POINT('',#35018);
#9460=VERTEX_POINT('',#35019);
#9461=VERTEX_POINT('',#35069);
#9462=VERTEX_POINT('',#35070);
#9463=VERTEX_POINT('',#35117);
#9464=VERTEX_POINT('',#35118);
#9465=VERTEX_POINT('',#35165);
#9466=VERTEX_POINT('',#35166);
#9467=VERTEX_POINT('',#35216);
#9468=VERTEX_POINT('',#35217);
#9469=VERTEX_POINT('',#35267);
#9470=VERTEX_POINT('',#35268);
#9471=VERTEX_POINT('',#35315);
#9472=VERTEX_POINT('',#35316);
#9473=VERTEX_POINT('',#35366);
#9474=VERTEX_POINT('',#35367);
#9475=VERTEX_POINT('',#35417);
#9476=VERTEX_POINT('',#35418);
#9477=VERTEX_POINT('',#35465);
#9478=VERTEX_POINT('',#35466);
#9479=VERTEX_POINT('',#35513);
#9480=VERTEX_POINT('',#35514);
#9481=VERTEX_POINT('',#35564);
#9482=VERTEX_POINT('',#35565);
#9483=VERTEX_POINT('',#35615);
#9484=VERTEX_POINT('',#35616);
#9485=VERTEX_POINT('',#35663);
#9486=VERTEX_POINT('',#35664);
#9487=VERTEX_POINT('',#35714);
#9488=VERTEX_POINT('',#35715);
#9489=VERTEX_POINT('',#35765);
#9490=VERTEX_POINT('',#35766);
#9491=VERTEX_POINT('',#35813);
#9492=VERTEX_POINT('',#35814);
#9493=VERTEX_POINT('',#35861);
#9494=VERTEX_POINT('',#35862);
#9495=VERTEX_POINT('',#35912);
#9496=VERTEX_POINT('',#35913);
#9497=VERTEX_POINT('',#35963);
#9498=VERTEX_POINT('',#35964);
#9499=VERTEX_POINT('',#36011);
#9500=VERTEX_POINT('',#36012);
#9501=VERTEX_POINT('',#36062);
#9502=VERTEX_POINT('',#36063);
#9503=VERTEX_POINT('',#36113);
#9504=VERTEX_POINT('',#36114);
#9505=VERTEX_POINT('',#36161);
#9506=VERTEX_POINT('',#36162);
#9507=VERTEX_POINT('',#36209);
#9508=VERTEX_POINT('',#36210);
#9509=VERTEX_POINT('',#36260);
#9510=VERTEX_POINT('',#36261);
#9511=VERTEX_POINT('',#36326);
#9512=VERTEX_POINT('',#36327);
#9513=VERTEX_POINT('',#36416);
#9514=VERTEX_POINT('',#36417);
#9515=VERTEX_POINT('',#36503);
#9516=VERTEX_POINT('',#36504);
#9517=VERTEX_POINT('',#36590);
#9518=VERTEX_POINT('',#36591);
#9519=VERTEX_POINT('',#36677);
#9520=VERTEX_POINT('',#36678);
#9521=VERTEX_POINT('',#36764);
#9522=VERTEX_POINT('',#36765);
#9523=VERTEX_POINT('',#36851);
#9524=VERTEX_POINT('',#36852);
#9525=VERTEX_POINT('',#36941);
#9526=VERTEX_POINT('',#36942);
#9527=VERTEX_POINT('',#36944);
#9528=VERTEX_POINT('',#36951);
#9529=VERTEX_POINT('',#36952);
#9530=VERTEX_POINT('',#36971);
#9531=VERTEX_POINT('',#36987);
#9532=VERTEX_POINT('',#36988);
#9533=VERTEX_POINT('',#37025);
#9534=VERTEX_POINT('',#37026);
#9535=VERTEX_POINT('',#37061);
#9536=VERTEX_POINT('',#37062);
#9537=VERTEX_POINT('',#37099);
#9538=VERTEX_POINT('',#37100);
#9539=VERTEX_POINT('',#37135);
#9540=VERTEX_POINT('',#37136);
#9541=VERTEX_POINT('',#37173);
#9542=VERTEX_POINT('',#37174);
#9543=VERTEX_POINT('',#37210);
#9544=VERTEX_POINT('',#37211);
#9545=VERTEX_POINT('',#37245);
#9546=VERTEX_POINT('',#37246);
#9547=VERTEX_POINT('',#37272);
#9548=VERTEX_POINT('',#37273);
#9549=VERTEX_POINT('',#37296);
#9550=VERTEX_POINT('',#37297);
#9551=VERTEX_POINT('',#37320);
#9552=VERTEX_POINT('',#37321);
#9553=VERTEX_POINT('',#37344);
#9554=VERTEX_POINT('',#37345);
#9555=VERTEX_POINT('',#37370);
#9556=VERTEX_POINT('',#37371);
#9557=VERTEX_POINT('',#37394);
#9558=VERTEX_POINT('',#37395);
#9559=VERTEX_POINT('',#37418);
#9560=VERTEX_POINT('',#37419);
#9561=VERTEX_POINT('',#37444);
#9562=VERTEX_POINT('',#37445);
#9563=VERTEX_POINT('',#37468);
#9564=VERTEX_POINT('',#37469);
#9565=VERTEX_POINT('',#37492);
#9566=VERTEX_POINT('',#37493);
#9567=VERTEX_POINT('',#37516);
#9568=VERTEX_POINT('',#37517);
#9569=VERTEX_POINT('',#37542);
#9570=VERTEX_POINT('',#37543);
#9571=VERTEX_POINT('',#37566);
#9572=VERTEX_POINT('',#37567);
#9573=VERTEX_POINT('',#37590);
#9574=VERTEX_POINT('',#37591);
#9575=VERTEX_POINT('',#37616);
#9576=VERTEX_POINT('',#37617);
#9577=VERTEX_POINT('',#37640);
#9578=VERTEX_POINT('',#37641);
#9579=VERTEX_POINT('',#37664);
#9580=VERTEX_POINT('',#37665);
#9581=VERTEX_POINT('',#37688);
#9582=VERTEX_POINT('',#37689);
#9583=VERTEX_POINT('',#37714);
#9584=VERTEX_POINT('',#37715);
#9585=VERTEX_POINT('',#37738);
#9586=VERTEX_POINT('',#37739);
#9587=VERTEX_POINT('',#37762);
#9588=VERTEX_POINT('',#37763);
#9589=VERTEX_POINT('',#37788);
#9590=VERTEX_POINT('',#37789);
#9591=VERTEX_POINT('',#37812);
#9592=VERTEX_POINT('',#37813);
#9593=VERTEX_POINT('',#37836);
#9594=VERTEX_POINT('',#37837);
#9595=VERTEX_POINT('',#37860);
#9596=VERTEX_POINT('',#37861);
#9597=VERTEX_POINT('',#37886);
#9598=VERTEX_POINT('',#37887);
#9599=VERTEX_POINT('',#37910);
#9600=VERTEX_POINT('',#37911);
#9601=VERTEX_POINT('',#37934);
#9602=VERTEX_POINT('',#37935);
#9603=VERTEX_POINT('',#37960);
#9604=VERTEX_POINT('',#37961);
#9605=VERTEX_POINT('',#37984);
#9606=VERTEX_POINT('',#37985);
#9607=VERTEX_POINT('',#38008);
#9608=VERTEX_POINT('',#38009);
#9609=VERTEX_POINT('',#38032);
#9610=VERTEX_POINT('',#38033);
#9611=VERTEX_POINT('',#38058);
#9612=VERTEX_POINT('',#38059);
#9613=VERTEX_POINT('',#38082);
#9614=VERTEX_POINT('',#38083);
#9615=VERTEX_POINT('',#38106);
#9616=VERTEX_POINT('',#38107);
#9617=VERTEX_POINT('',#38132);
#9618=VERTEX_POINT('',#38133);
#9619=VERTEX_POINT('',#38156);
#9620=VERTEX_POINT('',#38157);
#9621=VERTEX_POINT('',#38180);
#9622=VERTEX_POINT('',#38181);
#9623=VERTEX_POINT('',#38204);
#9624=VERTEX_POINT('',#38205);
#9625=VERTEX_POINT('',#38230);
#9626=VERTEX_POINT('',#38231);
#9627=VERTEX_POINT('',#38254);
#9628=VERTEX_POINT('',#38255);
#9629=VERTEX_POINT('',#38278);
#9630=VERTEX_POINT('',#38279);
#9631=VERTEX_POINT('',#38304);
#9632=VERTEX_POINT('',#38305);
#9633=VERTEX_POINT('',#38328);
#9634=VERTEX_POINT('',#38329);
#9635=VERTEX_POINT('',#38352);
#9636=VERTEX_POINT('',#38353);
#9637=VERTEX_POINT('',#38377);
#9638=VERTEX_POINT('',#38378);
#9639=VERTEX_POINT('',#38404);
#9640=VERTEX_POINT('',#38405);
#9641=VERTEX_POINT('',#38441);
#9642=VERTEX_POINT('',#38442);
#9643=VERTEX_POINT('',#38477);
#9644=VERTEX_POINT('',#38478);
#9645=VERTEX_POINT('',#38515);
#9646=VERTEX_POINT('',#38516);
#9647=VERTEX_POINT('',#38551);
#9648=VERTEX_POINT('',#38552);
#9649=VERTEX_POINT('',#38589);
#9650=VERTEX_POINT('',#38590);
#9651=VERTEX_POINT('',#38626);
#9652=VERTEX_POINT('',#38627);
#9653=VERTEX_POINT('',#38663);
#9654=VERTEX_POINT('',#38665);
#9655=VERTEX_POINT('',#38703);
#9656=VERTEX_POINT('',#38743);
#9657=VERTEX_POINT('',#40739);
#9658=VERTEX_POINT('',#42824);
#9659=VERTEX_POINT('',#42876);
#9660=VERTEX_POINT('',#42877);
#9661=VERTEX_POINT('',#42879);
#9662=VERTEX_POINT('',#42881);
#9663=VERTEX_POINT('',#42885);
#9664=VERTEX_POINT('',#42887);
#9665=VERTEX_POINT('',#42891);
#9666=VERTEX_POINT('',#42895);
#9667=VERTEX_POINT('',#42901);
#9668=VERTEX_POINT('',#42903);
#9669=VERTEX_POINT('',#42908);
#9670=VERTEX_POINT('',#42912);
#9671=VERTEX_POINT('',#42919);
#9672=VERTEX_POINT('',#42921);
#9673=VERTEX_POINT('',#42925);
#9674=VERTEX_POINT('',#42927);
#9675=VERTEX_POINT('',#42934);
#9676=VERTEX_POINT('',#42935);
#9677=VERTEX_POINT('',#42939);
#9678=VERTEX_POINT('',#42940);
#9679=VERTEX_POINT('',#42949);
#9680=VERTEX_POINT('',#42973);
#9681=VERTEX_POINT('',#42975);
#9682=VERTEX_POINT('',#43015);
#9683=VERTEX_POINT('',#43017);
#9684=VERTEX_POINT('',#43021);
#9685=VERTEX_POINT('',#43023);
#9686=VERTEX_POINT('',#43030);
#9687=VERTEX_POINT('',#43032);
#9688=VERTEX_POINT('',#43036);
#9689=VERTEX_POINT('',#43037);
#9690=VERTEX_POINT('',#43041);
#9691=VERTEX_POINT('',#43042);
#9692=VERTEX_POINT('',#43049);
#9693=VERTEX_POINT('',#43067);
#9694=VERTEX_POINT('',#43069);
#9695=VERTEX_POINT('',#43109);
#9696=VERTEX_POINT('',#43110);
#9697=VERTEX_POINT('',#43112);
#9698=VERTEX_POINT('',#43114);
#9699=VERTEX_POINT('',#43116);
#9700=VERTEX_POINT('',#43118);
#9701=VERTEX_POINT('',#43122);
#9702=VERTEX_POINT('',#43124);
#9703=VERTEX_POINT('',#43128);
#9704=VERTEX_POINT('',#43130);
#9705=VERTEX_POINT('',#43132);
#9706=VERTEX_POINT('',#43134);
#9707=VERTEX_POINT('',#43138);
#9708=VERTEX_POINT('',#43142);
#9709=VERTEX_POINT('',#43154);
#9710=VERTEX_POINT('',#43156);
#9711=VERTEX_POINT('',#43160);
#9712=VERTEX_POINT('',#43162);
#9713=VERTEX_POINT('',#43169);
#9714=VERTEX_POINT('',#43171);
#9715=VERTEX_POINT('',#43175);
#9716=VERTEX_POINT('',#43177);
#9717=VERTEX_POINT('',#43184);
#9718=VERTEX_POINT('',#43185);
#9719=VERTEX_POINT('',#43187);
#9720=VERTEX_POINT('',#43189);
#9721=VERTEX_POINT('',#43191);
#9722=VERTEX_POINT('',#43193);
#9723=VERTEX_POINT('',#43195);
#9724=VERTEX_POINT('',#43197);
#9725=VERTEX_POINT('',#43201);
#9726=VERTEX_POINT('',#43203);
#9727=VERTEX_POINT('',#43207);
#9728=VERTEX_POINT('',#43211);
#9729=VERTEX_POINT('',#43215);
#9730=VERTEX_POINT('',#43219);
#9731=VERTEX_POINT('',#43220);
#9732=VERTEX_POINT('',#43223);
#9733=VERTEX_POINT('',#43235);
#9734=VERTEX_POINT('',#43236);
#9735=VERTEX_POINT('',#43238);
#9736=VERTEX_POINT('',#43240);
#9737=VERTEX_POINT('',#43244);
#9738=VERTEX_POINT('',#43246);
#9739=VERTEX_POINT('',#43250);
#9740=VERTEX_POINT('',#43252);
#9741=VERTEX_POINT('',#43256);
#9742=VERTEX_POINT('',#43258);
#9743=VERTEX_POINT('',#43262);
#9744=VERTEX_POINT('',#43264);
#9745=VERTEX_POINT('',#43272);
#9746=VERTEX_POINT('',#43275);
#9747=VERTEX_POINT('',#43279);
#9748=VERTEX_POINT('',#43283);
#9749=VERTEX_POINT('',#43289);
#9750=VERTEX_POINT('',#43291);
#9751=VERTEX_POINT('',#43295);
#9752=VERTEX_POINT('',#43297);
#9753=VERTEX_POINT('',#43304);
#9754=VERTEX_POINT('',#43307);
#9755=VERTEX_POINT('',#43311);
#9756=VERTEX_POINT('',#43315);
#9757=VERTEX_POINT('',#43319);
#9758=VERTEX_POINT('',#43322);
#9759=VERTEX_POINT('',#43326);
#9760=VERTEX_POINT('',#43330);
#9761=VERTEX_POINT('',#43335);
#9762=VERTEX_POINT('',#43336);
#9763=VERTEX_POINT('',#43338);
#9764=VERTEX_POINT('',#43340);
#9765=VERTEX_POINT('',#43344);
#9766=VERTEX_POINT('',#43346);
#9767=VERTEX_POINT('',#43350);
#9768=VERTEX_POINT('',#43352);
#9769=VERTEX_POINT('',#43356);
#9770=VERTEX_POINT('',#43358);
#9771=VERTEX_POINT('',#43362);
#9772=VERTEX_POINT('',#43364);
#9773=EDGE_CURVE('',#8136,#8136,#7470,.T.);
#9774=EDGE_CURVE('',#8136,#8137,#4606,.T.);
#9775=EDGE_CURVE('',#8137,#8137,#7471,.T.);
#9776=EDGE_CURVE('',#8138,#8139,#4607,.T.);
#9777=EDGE_CURVE('',#8138,#8140,#4608,.T.);
#9778=EDGE_CURVE('',#8140,#8141,#4609,.T.);
#9779=EDGE_CURVE('',#8141,#8139,#4610,.T.);
#9780=EDGE_CURVE('',#8142,#8143,#4611,.T.);
#9781=EDGE_CURVE('',#8142,#8141,#4612,.T.);
#9782=EDGE_CURVE('',#8143,#8140,#4613,.T.);
#9783=EDGE_CURVE('',#8144,#8145,#4614,.T.);
#9784=EDGE_CURVE('',#8144,#8142,#4615,.T.);
#9785=EDGE_CURVE('',#8143,#8145,#4616,.T.);
#9786=EDGE_CURVE('',#8139,#8146,#4617,.T.);
#9787=EDGE_CURVE('',#8146,#8147,#4618,.T.);
#9788=EDGE_CURVE('',#8138,#8147,#4619,.T.);
#9789=EDGE_CURVE('',#8148,#8145,#4620,.T.);
#9790=EDGE_CURVE('',#8149,#8148,#4621,.T.);
#9791=EDGE_CURVE('',#8149,#8144,#4622,.T.);
#9792=EDGE_CURVE('',#8150,#8150,#7472,.T.);
#9793=EDGE_CURVE('',#8150,#8151,#4623,.T.);
#9794=EDGE_CURVE('',#8151,#8151,#7473,.T.);
#9795=EDGE_CURVE('',#8152,#8152,#7474,.T.);
#9796=EDGE_CURVE('',#8152,#8153,#4624,.T.);
#9797=EDGE_CURVE('',#8153,#8153,#7475,.T.);
#9798=EDGE_CURVE('',#8154,#8154,#7476,.T.);
#9799=EDGE_CURVE('',#8154,#8155,#4625,.T.);
#9800=EDGE_CURVE('',#8155,#8155,#7477,.T.);
#9801=EDGE_CURVE('',#8156,#8156,#7478,.T.);
#9802=EDGE_CURVE('',#8156,#8157,#4626,.T.);
#9803=EDGE_CURVE('',#8157,#8157,#7479,.T.);
#9804=EDGE_CURVE('',#8158,#8158,#7480,.T.);
#9805=EDGE_CURVE('',#8158,#8159,#4627,.T.);
#9806=EDGE_CURVE('',#8159,#8159,#7481,.T.);
#9807=EDGE_CURVE('',#8160,#8160,#7482,.T.);
#9808=EDGE_CURVE('',#8160,#8161,#4628,.T.);
#9809=EDGE_CURVE('',#8161,#8161,#7483,.T.);
#9810=EDGE_CURVE('',#8162,#8162,#7484,.T.);
#9811=EDGE_CURVE('',#8162,#8163,#4629,.T.);
#9812=EDGE_CURVE('',#8163,#8163,#7485,.T.);
#9813=EDGE_CURVE('',#8164,#8164,#7486,.T.);
#9814=EDGE_CURVE('',#8164,#8165,#4630,.T.);
#9815=EDGE_CURVE('',#8165,#8165,#7487,.T.);
#9816=EDGE_CURVE('',#8166,#8166,#7488,.T.);
#9817=EDGE_CURVE('',#8166,#8167,#4631,.T.);
#9818=EDGE_CURVE('',#8167,#8167,#7489,.T.);
#9819=EDGE_CURVE('',#8168,#8168,#7490,.T.);
#9820=EDGE_CURVE('',#8168,#8169,#4632,.T.);
#9821=EDGE_CURVE('',#8169,#8169,#7491,.T.);
#9822=EDGE_CURVE('',#8170,#8170,#7492,.T.);
#9823=EDGE_CURVE('',#8170,#8171,#4633,.T.);
#9824=EDGE_CURVE('',#8171,#8171,#7493,.T.);
#9825=EDGE_CURVE('',#8172,#8172,#7494,.T.);
#9826=EDGE_CURVE('',#8172,#8173,#4634,.T.);
#9827=EDGE_CURVE('',#8173,#8173,#7495,.T.);
#9828=EDGE_CURVE('',#8174,#8174,#7496,.T.);
#9829=EDGE_CURVE('',#8174,#8175,#4635,.T.);
#9830=EDGE_CURVE('',#8175,#8175,#7497,.T.);
#9831=EDGE_CURVE('',#8176,#8176,#7498,.T.);
#9832=EDGE_CURVE('',#8176,#8177,#4636,.T.);
#9833=EDGE_CURVE('',#8177,#8177,#7499,.T.);
#9834=EDGE_CURVE('',#8178,#8178,#7500,.T.);
#9835=EDGE_CURVE('',#8178,#8179,#4637,.T.);
#9836=EDGE_CURVE('',#8179,#8179,#7501,.T.);
#9837=EDGE_CURVE('',#8180,#8180,#7502,.T.);
#9838=EDGE_CURVE('',#8180,#8181,#4638,.T.);
#9839=EDGE_CURVE('',#8181,#8181,#7503,.T.);
#9840=EDGE_CURVE('',#8182,#8182,#7504,.T.);
#9841=EDGE_CURVE('',#8182,#8183,#4639,.T.);
#9842=EDGE_CURVE('',#8183,#8183,#7505,.T.);
#9843=EDGE_CURVE('',#8184,#8184,#7506,.T.);
#9844=EDGE_CURVE('',#8184,#8185,#4640,.T.);
#9845=EDGE_CURVE('',#8185,#8185,#7507,.T.);
#9846=EDGE_CURVE('',#8186,#8186,#7508,.T.);
#9847=EDGE_CURVE('',#8186,#8187,#4641,.T.);
#9848=EDGE_CURVE('',#8187,#8187,#7509,.T.);
#9849=EDGE_CURVE('',#8146,#8188,#4642,.T.);
#9850=EDGE_CURVE('',#8188,#8189,#4643,.T.);
#9851=EDGE_CURVE('',#8147,#8189,#4644,.T.);
#9852=EDGE_CURVE('',#8190,#8149,#4645,.T.);
#9853=EDGE_CURVE('',#8191,#8148,#4646,.T.);
#9854=EDGE_CURVE('',#8190,#8191,#4647,.T.);
#9855=EDGE_CURVE('',#8188,#8190,#4648,.T.);
#9856=EDGE_CURVE('',#8189,#8191,#4649,.T.);
#9857=EDGE_CURVE('',#8192,#8193,#4650,.T.);
#9858=EDGE_CURVE('',#8193,#8194,#4651,.T.);
#9859=EDGE_CURVE('',#8195,#8194,#4652,.T.);
#9860=EDGE_CURVE('',#8192,#8195,#4653,.T.);
#9861=EDGE_CURVE('',#8196,#8192,#4654,.T.);
#9862=EDGE_CURVE('',#8197,#8195,#4655,.T.);
#9863=EDGE_CURVE('',#8196,#8197,#4656,.T.);
#9864=EDGE_CURVE('',#8198,#8196,#4657,.T.);
#9865=EDGE_CURVE('',#8199,#8197,#4658,.T.);
#9866=EDGE_CURVE('',#8198,#8199,#4659,.T.);
#9867=EDGE_CURVE('',#8193,#8198,#4660,.T.);
#9868=EDGE_CURVE('',#8194,#8199,#4661,.T.);
#9869=EDGE_CURVE('',#8200,#8201,#4662,.T.);
#9870=EDGE_CURVE('',#8201,#8202,#4663,.T.);
#9871=EDGE_CURVE('',#8203,#8202,#4664,.T.);
#9872=EDGE_CURVE('',#8200,#8203,#4665,.T.);
#9873=EDGE_CURVE('',#8204,#8200,#4666,.T.);
#9874=EDGE_CURVE('',#8205,#8203,#4667,.T.);
#9875=EDGE_CURVE('',#8204,#8205,#4668,.T.);
#9876=EDGE_CURVE('',#8206,#8204,#4669,.T.);
#9877=EDGE_CURVE('',#8207,#8205,#4670,.T.);
#9878=EDGE_CURVE('',#8206,#8207,#4671,.T.);
#9879=EDGE_CURVE('',#8201,#8206,#4672,.T.);
#9880=EDGE_CURVE('',#8202,#8207,#4673,.T.);
#9881=EDGE_CURVE('',#8208,#8208,#7510,.T.);
#9882=EDGE_CURVE('',#8208,#8209,#4674,.T.);
#9883=EDGE_CURVE('',#8209,#8209,#7511,.T.);
#9884=EDGE_CURVE('',#8210,#8210,#7512,.T.);
#9885=EDGE_CURVE('',#8210,#8211,#4675,.T.);
#9886=EDGE_CURVE('',#8211,#8211,#7513,.T.);
#9887=EDGE_CURVE('',#8212,#8212,#7514,.T.);
#9888=EDGE_CURVE('',#8212,#8213,#4676,.T.);
#9889=EDGE_CURVE('',#8213,#8213,#7515,.T.);
#9890=EDGE_CURVE('',#8214,#8214,#7516,.T.);
#9891=EDGE_CURVE('',#8214,#8215,#4677,.T.);
#9892=EDGE_CURVE('',#8215,#8215,#7517,.T.);
#9893=EDGE_CURVE('',#8216,#8216,#7518,.T.);
#9894=EDGE_CURVE('',#8216,#8217,#4678,.T.);
#9895=EDGE_CURVE('',#8217,#8217,#7519,.T.);
#9896=EDGE_CURVE('',#8218,#8218,#7520,.T.);
#9897=EDGE_CURVE('',#8218,#8219,#4679,.T.);
#9898=EDGE_CURVE('',#8219,#8219,#7521,.T.);
#9899=EDGE_CURVE('',#8220,#8220,#7522,.T.);
#9900=EDGE_CURVE('',#8220,#8221,#4680,.T.);
#9901=EDGE_CURVE('',#8221,#8221,#7523,.T.);
#9902=EDGE_CURVE('',#8222,#8222,#7524,.T.);
#9903=EDGE_CURVE('',#8222,#8223,#4681,.T.);
#9904=EDGE_CURVE('',#8223,#8223,#7525,.T.);
#9905=EDGE_CURVE('',#8224,#8225,#4682,.T.);
#9906=EDGE_CURVE('',#8226,#8224,#4683,.T.);
#9907=EDGE_CURVE('',#8227,#8226,#4684,.T.);
#9908=EDGE_CURVE('',#8227,#8225,#4685,.T.);
#9909=EDGE_CURVE('',#8225,#8228,#4686,.T.);
#9910=EDGE_CURVE('',#8229,#8227,#4687,.T.);
#9911=EDGE_CURVE('',#8229,#8228,#4688,.T.);
#9912=EDGE_CURVE('',#8228,#8230,#4689,.T.);
#9913=EDGE_CURVE('',#8231,#8229,#4690,.T.);
#9914=EDGE_CURVE('',#8231,#8230,#4691,.T.);
#9915=EDGE_CURVE('',#8230,#8224,#4692,.T.);
#9916=EDGE_CURVE('',#8226,#8231,#4693,.T.);
#9917=EDGE_CURVE('',#8232,#8232,#7526,.T.);
#9918=EDGE_CURVE('',#8232,#8233,#4694,.T.);
#9919=EDGE_CURVE('',#8233,#8233,#7527,.T.);
#9920=EDGE_CURVE('',#8234,#8234,#7528,.T.);
#9921=EDGE_CURVE('',#8234,#8235,#4695,.T.);
#9922=EDGE_CURVE('',#8235,#8235,#7529,.T.);
#9923=EDGE_CURVE('',#8236,#8237,#4696,.T.);
#9924=EDGE_CURVE('',#8237,#8238,#4697,.T.);
#9925=EDGE_CURVE('',#8239,#8238,#4698,.T.);
#9926=EDGE_CURVE('',#8236,#8239,#4699,.T.);
#9927=EDGE_CURVE('',#8240,#8236,#4700,.T.);
#9928=EDGE_CURVE('',#8241,#8239,#4701,.T.);
#9929=EDGE_CURVE('',#8240,#8241,#4702,.T.);
#9930=EDGE_CURVE('',#8242,#8240,#4703,.T.);
#9931=EDGE_CURVE('',#8243,#8241,#4704,.T.);
#9932=EDGE_CURVE('',#8242,#8243,#4705,.T.);
#9933=EDGE_CURVE('',#8237,#8242,#4706,.T.);
#9934=EDGE_CURVE('',#8238,#8243,#4707,.T.);
#9935=EDGE_CURVE('',#8244,#8244,#7530,.T.);
#9936=EDGE_CURVE('',#8244,#8245,#4708,.T.);
#9937=EDGE_CURVE('',#8245,#8245,#7531,.T.);
#9938=EDGE_CURVE('',#8246,#8246,#7532,.T.);
#9939=EDGE_CURVE('',#8246,#8247,#4709,.T.);
#9940=EDGE_CURVE('',#8247,#8247,#7533,.T.);
#9941=EDGE_CURVE('',#8248,#8248,#7534,.T.);
#9942=EDGE_CURVE('',#8248,#8249,#4710,.T.);
#9943=EDGE_CURVE('',#8249,#8249,#7535,.T.);
#9944=EDGE_CURVE('',#8250,#8250,#7536,.T.);
#9945=EDGE_CURVE('',#8250,#8251,#4711,.T.);
#9946=EDGE_CURVE('',#8251,#8251,#7537,.T.);
#9947=EDGE_CURVE('',#8252,#8252,#7538,.T.);
#9948=EDGE_CURVE('',#8252,#8253,#4712,.T.);
#9949=EDGE_CURVE('',#8253,#8253,#7539,.T.);
#9950=EDGE_CURVE('',#8254,#8254,#7540,.T.);
#9951=EDGE_CURVE('',#8254,#8255,#4713,.T.);
#9952=EDGE_CURVE('',#8255,#8255,#7541,.T.);
#9953=EDGE_CURVE('',#8256,#8257,#4714,.T.);
#9954=EDGE_CURVE('',#8257,#8258,#4715,.T.);
#9955=EDGE_CURVE('',#8259,#8258,#4716,.T.);
#9956=EDGE_CURVE('',#8256,#8259,#4717,.T.);
#9957=EDGE_CURVE('',#8260,#8256,#4718,.T.);
#9958=EDGE_CURVE('',#8261,#8259,#4719,.T.);
#9959=EDGE_CURVE('',#8260,#8261,#4720,.T.);
#9960=EDGE_CURVE('',#8262,#8260,#4721,.T.);
#9961=EDGE_CURVE('',#8263,#8261,#4722,.T.);
#9962=EDGE_CURVE('',#8262,#8263,#4723,.T.);
#9963=EDGE_CURVE('',#8257,#8262,#4724,.T.);
#9964=EDGE_CURVE('',#8258,#8263,#4725,.T.);
#9965=EDGE_CURVE('',#8264,#8264,#7542,.T.);
#9966=EDGE_CURVE('',#8264,#8265,#4726,.T.);
#9967=EDGE_CURVE('',#8265,#8265,#7543,.T.);
#9968=EDGE_CURVE('',#8266,#8266,#7544,.T.);
#9969=EDGE_CURVE('',#8266,#8267,#4727,.T.);
#9970=EDGE_CURVE('',#8267,#8267,#7545,.T.);
#9971=EDGE_CURVE('',#8268,#8268,#7546,.T.);
#9972=EDGE_CURVE('',#8268,#8269,#4728,.T.);
#9973=EDGE_CURVE('',#8269,#8269,#7547,.T.);
#9974=EDGE_CURVE('',#8270,#8270,#7548,.T.);
#9975=EDGE_CURVE('',#8270,#8271,#4729,.T.);
#9976=EDGE_CURVE('',#8271,#8271,#7549,.T.);
#9977=EDGE_CURVE('',#8272,#8272,#7550,.T.);
#9978=EDGE_CURVE('',#8272,#8273,#4730,.T.);
#9979=EDGE_CURVE('',#8273,#8273,#7551,.T.);
#9980=EDGE_CURVE('',#8274,#8274,#7552,.T.);
#9981=EDGE_CURVE('',#8274,#8275,#4731,.T.);
#9982=EDGE_CURVE('',#8275,#8275,#7553,.T.);
#9983=EDGE_CURVE('',#8276,#8277,#4732,.T.);
#9984=EDGE_CURVE('',#8277,#8278,#4733,.T.);
#9985=EDGE_CURVE('',#8279,#8278,#4734,.T.);
#9986=EDGE_CURVE('',#8276,#8279,#4735,.T.);
#9987=EDGE_CURVE('',#8280,#8276,#4736,.T.);
#9988=EDGE_CURVE('',#8281,#8279,#4737,.T.);
#9989=EDGE_CURVE('',#8280,#8281,#4738,.T.);
#9990=EDGE_CURVE('',#8282,#8280,#4739,.T.);
#9991=EDGE_CURVE('',#8283,#8281,#4740,.T.);
#9992=EDGE_CURVE('',#8282,#8283,#4741,.T.);
#9993=EDGE_CURVE('',#8277,#8282,#4742,.T.);
#9994=EDGE_CURVE('',#8278,#8283,#4743,.T.);
#9995=EDGE_CURVE('',#8284,#8284,#7554,.T.);
#9996=EDGE_CURVE('',#8284,#8285,#4744,.T.);
#9997=EDGE_CURVE('',#8285,#8285,#7555,.T.);
#9998=EDGE_CURVE('',#8286,#8286,#7556,.T.);
#9999=EDGE_CURVE('',#8286,#8287,#4745,.T.);
#10000=EDGE_CURVE('',#8287,#8287,#7557,.T.);
#10001=EDGE_CURVE('',#8288,#8288,#7558,.T.);
#10002=EDGE_CURVE('',#8288,#8289,#4746,.T.);
#10003=EDGE_CURVE('',#8289,#8289,#7559,.T.);
#10004=EDGE_CURVE('',#8290,#8290,#7560,.T.);
#10005=EDGE_CURVE('',#8290,#8291,#4747,.T.);
#10006=EDGE_CURVE('',#8291,#8291,#7561,.T.);
#10007=EDGE_CURVE('',#8292,#8293,#4748,.T.);
#10008=EDGE_CURVE('',#8293,#8294,#4749,.T.);
#10009=EDGE_CURVE('',#8295,#8294,#4750,.T.);
#10010=EDGE_CURVE('',#8292,#8295,#4751,.T.);
#10011=EDGE_CURVE('',#8296,#8292,#4752,.T.);
#10012=EDGE_CURVE('',#8297,#8295,#4753,.T.);
#10013=EDGE_CURVE('',#8296,#8297,#4754,.T.);
#10014=EDGE_CURVE('',#8298,#8296,#4755,.T.);
#10015=EDGE_CURVE('',#8299,#8297,#4756,.T.);
#10016=EDGE_CURVE('',#8298,#8299,#4757,.T.);
#10017=EDGE_CURVE('',#8293,#8298,#4758,.T.);
#10018=EDGE_CURVE('',#8294,#8299,#4759,.T.);
#10019=EDGE_CURVE('',#8300,#8300,#7562,.T.);
#10020=EDGE_CURVE('',#8300,#8301,#4760,.T.);
#10021=EDGE_CURVE('',#8301,#8301,#7563,.T.);
#10022=EDGE_CURVE('',#8302,#8302,#7564,.T.);
#10023=EDGE_CURVE('',#8302,#8303,#4761,.T.);
#10024=EDGE_CURVE('',#8303,#8303,#7565,.T.);
#10025=EDGE_CURVE('',#8304,#8304,#7566,.T.);
#10026=EDGE_CURVE('',#8304,#8305,#4762,.T.);
#10027=EDGE_CURVE('',#8305,#8306,#7567,.T.);
#10028=EDGE_CURVE('',#8307,#8306,#4763,.T.);
#10029=EDGE_CURVE('',#8308,#8307,#7568,.T.);
#10030=EDGE_CURVE('',#8309,#8308,#4764,.T.);
#10031=EDGE_CURVE('',#8309,#8305,#7569,.T.);
#10032=EDGE_CURVE('',#8306,#8309,#4765,.T.);
#10033=EDGE_CURVE('',#8310,#8310,#7570,.T.);
#10034=EDGE_CURVE('',#8310,#8311,#4766,.T.);
#10035=EDGE_CURVE('',#8311,#8312,#7571,.T.);
#10036=EDGE_CURVE('',#8313,#8312,#4767,.T.);
#10037=EDGE_CURVE('',#8314,#8313,#7572,.T.);
#10038=EDGE_CURVE('',#8315,#8314,#4768,.T.);
#10039=EDGE_CURVE('',#8315,#8311,#7573,.T.);
#10040=EDGE_CURVE('',#8312,#8315,#4769,.T.);
#10041=EDGE_CURVE('',#8307,#8314,#4770,.T.);
#10042=EDGE_CURVE('',#8313,#8316,#4771,.T.);
#10043=EDGE_CURVE('',#8317,#8316,#4772,.T.);
#10044=EDGE_CURVE('',#8317,#8318,#4773,.T.);
#10045=EDGE_CURVE('',#8318,#8319,#4774,.T.);
#10046=EDGE_CURVE('',#8319,#8308,#4775,.T.);
#10047=EDGE_CURVE('',#8319,#8320,#4776,.T.);
#10048=EDGE_CURVE('',#8321,#8320,#4777,.T.);
#10049=EDGE_CURVE('',#8316,#8321,#4778,.T.);
#10050=EDGE_CURVE('',#8322,#8323,#4779,.T.);
#10051=EDGE_CURVE('',#8323,#8321,#4780,.T.);
#10052=EDGE_CURVE('',#8320,#8322,#4781,.T.);
#10053=EDGE_CURVE('',#8324,#8325,#4782,.T.);
#10054=EDGE_CURVE('',#8324,#8317,#4783,.T.);
#10055=EDGE_CURVE('',#8325,#8323,#4784,.T.);
#10056=EDGE_CURVE('',#8326,#8327,#4785,.T.);
#10057=EDGE_CURVE('',#8326,#8324,#4786,.T.);
#10058=EDGE_CURVE('',#8327,#8325,#4787,.T.);
#10059=EDGE_CURVE('',#8318,#8326,#4788,.T.);
#10060=EDGE_CURVE('',#8327,#8322,#4789,.T.);
#10061=EDGE_CURVE('',#8328,#8328,#7574,.T.);
#10062=EDGE_CURVE('',#8328,#8329,#4790,.T.);
#10063=EDGE_CURVE('',#8329,#8329,#7575,.T.);
#10064=EDGE_CURVE('',#8330,#8330,#7576,.T.);
#10065=EDGE_CURVE('',#8330,#8331,#4791,.T.);
#10066=EDGE_CURVE('',#8331,#8331,#7577,.T.);
#10067=EDGE_CURVE('',#8332,#8332,#7578,.T.);
#10068=EDGE_CURVE('',#8332,#8333,#4792,.T.);
#10069=EDGE_CURVE('',#8333,#8333,#7579,.T.);
#10070=EDGE_CURVE('',#8334,#8334,#7580,.T.);
#10071=EDGE_CURVE('',#8334,#8335,#4793,.T.);
#10072=EDGE_CURVE('',#8335,#8335,#7581,.T.);
#10073=EDGE_CURVE('',#8336,#8337,#4794,.T.);
#10074=EDGE_CURVE('',#8337,#8338,#4795,.T.);
#10075=EDGE_CURVE('',#8339,#8338,#4796,.T.);
#10076=EDGE_CURVE('',#8336,#8339,#4797,.T.);
#10077=EDGE_CURVE('',#8340,#8336,#4798,.T.);
#10078=EDGE_CURVE('',#8341,#8339,#4799,.T.);
#10079=EDGE_CURVE('',#8340,#8341,#4800,.T.);
#10080=EDGE_CURVE('',#8342,#8340,#4801,.T.);
#10081=EDGE_CURVE('',#8343,#8341,#4802,.T.);
#10082=EDGE_CURVE('',#8342,#8343,#4803,.T.);
#10083=EDGE_CURVE('',#8337,#8342,#4804,.T.);
#10084=EDGE_CURVE('',#8338,#8343,#4805,.T.);
#10085=EDGE_CURVE('',#8344,#8344,#7582,.T.);
#10086=EDGE_CURVE('',#8344,#8345,#4806,.T.);
#10087=EDGE_CURVE('',#8345,#8345,#7583,.T.);
#10088=EDGE_CURVE('',#8346,#8346,#7584,.T.);
#10089=EDGE_CURVE('',#8346,#8347,#4807,.T.);
#10090=EDGE_CURVE('',#8347,#8347,#7585,.T.);
#10091=EDGE_CURVE('',#8348,#8348,#7586,.T.);
#10092=EDGE_CURVE('',#8348,#8349,#4808,.T.);
#10093=EDGE_CURVE('',#8349,#8350,#7587,.T.);
#10094=EDGE_CURVE('',#8351,#8350,#4809,.T.);
#10095=EDGE_CURVE('',#8352,#8351,#7588,.T.);
#10096=EDGE_CURVE('',#8353,#8352,#4810,.T.);
#10097=EDGE_CURVE('',#8353,#8349,#7589,.T.);
#10098=EDGE_CURVE('',#8350,#8353,#4811,.T.);
#10099=EDGE_CURVE('',#8354,#8354,#7590,.T.);
#10100=EDGE_CURVE('',#8354,#8355,#4812,.T.);
#10101=EDGE_CURVE('',#8355,#8356,#7591,.T.);
#10102=EDGE_CURVE('',#8357,#8356,#4813,.T.);
#10103=EDGE_CURVE('',#8358,#8357,#7592,.T.);
#10104=EDGE_CURVE('',#8359,#8358,#4814,.T.);
#10105=EDGE_CURVE('',#8359,#8355,#7593,.T.);
#10106=EDGE_CURVE('',#8356,#8359,#4815,.T.);
#10107=EDGE_CURVE('',#8351,#8358,#4816,.T.);
#10108=EDGE_CURVE('',#8357,#8360,#4817,.T.);
#10109=EDGE_CURVE('',#8361,#8360,#4818,.T.);
#10110=EDGE_CURVE('',#8361,#8362,#4819,.T.);
#10111=EDGE_CURVE('',#8362,#8363,#4820,.T.);
#10112=EDGE_CURVE('',#8363,#8352,#4821,.T.);
#10113=EDGE_CURVE('',#8363,#8364,#4822,.T.);
#10114=EDGE_CURVE('',#8365,#8364,#4823,.T.);
#10115=EDGE_CURVE('',#8360,#8365,#4824,.T.);
#10116=EDGE_CURVE('',#8366,#8367,#4825,.T.);
#10117=EDGE_CURVE('',#8367,#8365,#4826,.T.);
#10118=EDGE_CURVE('',#8364,#8366,#4827,.T.);
#10119=EDGE_CURVE('',#8368,#8369,#4828,.T.);
#10120=EDGE_CURVE('',#8368,#8361,#4829,.T.);
#10121=EDGE_CURVE('',#8369,#8367,#4830,.T.);
#10122=EDGE_CURVE('',#8370,#8371,#4831,.T.);
#10123=EDGE_CURVE('',#8370,#8368,#4832,.T.);
#10124=EDGE_CURVE('',#8371,#8369,#4833,.T.);
#10125=EDGE_CURVE('',#8362,#8370,#4834,.T.);
#10126=EDGE_CURVE('',#8371,#8366,#4835,.T.);
#10127=EDGE_CURVE('',#8372,#8372,#7594,.T.);
#10128=EDGE_CURVE('',#8372,#8373,#4836,.T.);
#10129=EDGE_CURVE('',#8373,#8373,#7595,.T.);
#10130=EDGE_CURVE('',#8374,#8374,#7596,.T.);
#10131=EDGE_CURVE('',#8374,#8375,#4837,.T.);
#10132=EDGE_CURVE('',#8375,#8375,#7597,.T.);
#10133=EDGE_CURVE('',#8376,#8376,#7598,.T.);
#10134=EDGE_CURVE('',#8376,#8377,#4838,.T.);
#10135=EDGE_CURVE('',#8377,#8377,#7599,.T.);
#10136=EDGE_CURVE('',#8378,#8378,#7600,.T.);
#10137=EDGE_CURVE('',#8378,#8379,#4839,.T.);
#10138=EDGE_CURVE('',#8379,#8379,#7601,.T.);
#10139=EDGE_CURVE('',#8380,#8380,#7602,.T.);
#10140=EDGE_CURVE('',#8380,#8381,#4840,.T.);
#10141=EDGE_CURVE('',#8381,#8381,#7603,.T.);
#10142=EDGE_CURVE('',#8382,#8382,#7604,.T.);
#10143=EDGE_CURVE('',#8382,#8383,#4841,.T.);
#10144=EDGE_CURVE('',#8383,#8383,#7605,.T.);
#10145=EDGE_CURVE('',#8384,#8384,#7606,.T.);
#10146=EDGE_CURVE('',#8384,#8385,#4842,.T.);
#10147=EDGE_CURVE('',#8385,#8385,#7607,.T.);
#10148=EDGE_CURVE('',#8386,#8386,#7608,.T.);
#10149=EDGE_CURVE('',#8386,#8387,#4843,.T.);
#10150=EDGE_CURVE('',#8387,#8387,#7609,.T.);
#10151=EDGE_CURVE('',#8388,#8388,#7610,.T.);
#10152=EDGE_CURVE('',#8388,#8389,#4844,.T.);
#10153=EDGE_CURVE('',#8389,#8389,#7611,.T.);
#10154=EDGE_CURVE('',#8390,#8390,#7612,.T.);
#10155=EDGE_CURVE('',#8390,#8391,#4845,.T.);
#10156=EDGE_CURVE('',#8391,#8391,#7613,.T.);
#10157=EDGE_CURVE('',#8392,#8393,#4846,.T.);
#10158=EDGE_CURVE('',#8393,#8394,#4847,.T.);
#10159=EDGE_CURVE('',#8395,#8394,#4848,.T.);
#10160=EDGE_CURVE('',#8392,#8395,#4849,.T.);
#10161=EDGE_CURVE('',#8396,#8392,#4850,.T.);
#10162=EDGE_CURVE('',#8397,#8395,#4851,.T.);
#10163=EDGE_CURVE('',#8396,#8397,#4852,.T.);
#10164=EDGE_CURVE('',#8398,#8396,#4853,.T.);
#10165=EDGE_CURVE('',#8399,#8397,#4854,.T.);
#10166=EDGE_CURVE('',#8398,#8399,#4855,.T.);
#10167=EDGE_CURVE('',#8393,#8398,#4856,.T.);
#10168=EDGE_CURVE('',#8394,#8399,#4857,.T.);
#10169=EDGE_CURVE('',#8400,#8400,#7614,.T.);
#10170=EDGE_CURVE('',#8400,#8401,#4858,.T.);
#10171=EDGE_CURVE('',#8401,#8401,#7615,.T.);
#10172=EDGE_CURVE('',#8402,#8402,#7616,.T.);
#10173=EDGE_CURVE('',#8402,#8403,#4859,.T.);
#10174=EDGE_CURVE('',#8403,#8403,#7617,.T.);
#10175=EDGE_CURVE('',#8404,#8404,#7618,.T.);
#10176=EDGE_CURVE('',#8404,#8405,#4860,.T.);
#10177=EDGE_CURVE('',#8405,#8405,#7619,.T.);
#10178=EDGE_CURVE('',#8406,#8406,#7620,.T.);
#10179=EDGE_CURVE('',#8406,#8407,#4861,.T.);
#10180=EDGE_CURVE('',#8407,#8407,#7621,.T.);
#10181=EDGE_CURVE('',#8408,#8408,#7622,.T.);
#10182=EDGE_CURVE('',#8408,#8409,#4862,.T.);
#10183=EDGE_CURVE('',#8409,#8409,#7623,.T.);
#10184=EDGE_CURVE('',#8410,#8410,#7624,.T.);
#10185=EDGE_CURVE('',#8410,#8411,#4863,.T.);
#10186=EDGE_CURVE('',#8411,#8411,#7625,.T.);
#10187=EDGE_CURVE('',#8412,#8412,#7626,.T.);
#10188=EDGE_CURVE('',#8412,#8413,#4864,.T.);
#10189=EDGE_CURVE('',#8413,#8413,#7627,.T.);
#10190=EDGE_CURVE('',#8414,#8414,#7628,.T.);
#10191=EDGE_CURVE('',#8414,#8415,#4865,.T.);
#10192=EDGE_CURVE('',#8415,#8415,#7629,.T.);
#10193=EDGE_CURVE('',#8416,#8416,#7630,.T.);
#10194=EDGE_CURVE('',#8416,#8417,#4866,.T.);
#10195=EDGE_CURVE('',#8417,#8417,#7631,.T.);
#10196=EDGE_CURVE('',#8418,#8418,#7632,.T.);
#10197=EDGE_CURVE('',#8418,#8419,#4867,.T.);
#10198=EDGE_CURVE('',#8419,#8419,#7633,.T.);
#10199=EDGE_CURVE('',#8420,#8420,#7634,.T.);
#10200=EDGE_CURVE('',#8421,#8421,#7635,.T.);
#10201=EDGE_CURVE('',#8421,#8420,#4868,.T.);
#10202=EDGE_CURVE('',#8422,#8423,#4869,.T.);
#10203=EDGE_CURVE('',#8424,#8422,#7636,.T.);
#10204=EDGE_CURVE('',#8425,#8424,#4870,.T.);
#10205=EDGE_CURVE('',#8423,#8425,#7637,.T.);
#10206=EDGE_CURVE('',#8426,#8427,#4871,.T.);
#10207=EDGE_CURVE('',#8428,#8426,#7638,.T.);
#10208=EDGE_CURVE('',#8429,#8428,#4872,.T.);
#10209=EDGE_CURVE('',#8427,#8429,#7639,.T.);
#10210=EDGE_CURVE('',#8428,#8430,#4873,.T.);
#10211=EDGE_CURVE('',#8430,#8431,#4874,.T.);
#10212=EDGE_CURVE('',#8429,#8431,#4875,.T.);
#10213=EDGE_CURVE('',#8432,#8422,#4876,.T.);
#10214=EDGE_CURVE('',#8430,#8432,#4877,.T.);
#10215=EDGE_CURVE('',#8424,#8426,#4878,.T.);
#10216=EDGE_CURVE('',#8425,#8427,#4879,.T.);
#10217=EDGE_CURVE('',#8432,#8433,#4880,.T.);
#10218=EDGE_CURVE('',#8431,#8433,#4881,.T.);
#10219=EDGE_CURVE('',#8433,#8423,#4882,.T.);
#10220=EDGE_CURVE('',#8434,#8434,#7640,.T.);
#10221=EDGE_CURVE('',#8434,#8435,#4883,.T.);
#10222=EDGE_CURVE('',#8435,#8435,#7641,.T.);
#10223=EDGE_CURVE('',#8436,#8436,#7642,.T.);
#10224=EDGE_CURVE('',#8436,#8437,#4884,.T.);
#10225=EDGE_CURVE('',#8437,#8437,#7643,.T.);
#10226=EDGE_CURVE('',#8438,#8438,#7644,.T.);
#10227=EDGE_CURVE('',#8438,#8439,#4885,.T.);
#10228=EDGE_CURVE('',#8439,#8439,#7645,.T.);
#10229=EDGE_CURVE('',#8440,#8440,#7646,.T.);
#10230=EDGE_CURVE('',#8440,#8441,#4886,.T.);
#10231=EDGE_CURVE('',#8441,#8441,#7647,.T.);
#10232=EDGE_CURVE('',#8442,#8442,#7648,.T.);
#10233=EDGE_CURVE('',#8442,#8443,#4887,.T.);
#10234=EDGE_CURVE('',#8443,#8443,#7649,.T.);
#10235=EDGE_CURVE('',#8444,#8444,#7650,.T.);
#10236=EDGE_CURVE('',#8444,#8445,#4888,.T.);
#10237=EDGE_CURVE('',#8445,#8445,#7651,.T.);
#10238=EDGE_CURVE('',#8446,#8446,#7652,.T.);
#10239=EDGE_CURVE('',#8446,#8447,#4889,.T.);
#10240=EDGE_CURVE('',#8447,#8447,#7653,.T.);
#10241=EDGE_CURVE('',#8448,#8448,#7654,.T.);
#10242=EDGE_CURVE('',#8448,#8449,#4890,.T.);
#10243=EDGE_CURVE('',#8449,#8449,#7655,.T.);
#10244=EDGE_CURVE('',#8450,#8450,#7656,.T.);
#10245=EDGE_CURVE('',#8450,#8451,#4891,.T.);
#10246=EDGE_CURVE('',#8451,#8451,#7657,.T.);
#10247=EDGE_CURVE('',#8452,#8452,#7658,.T.);
#10248=EDGE_CURVE('',#8452,#8453,#4892,.T.);
#10249=EDGE_CURVE('',#8453,#8453,#7659,.T.);
#10250=EDGE_CURVE('',#8454,#8454,#7660,.T.);
#10251=EDGE_CURVE('',#8455,#8455,#7661,.T.);
#10252=EDGE_CURVE('',#8455,#8454,#4893,.T.);
#10253=EDGE_CURVE('',#8456,#8456,#7662,.T.);
#10254=EDGE_CURVE('',#8456,#8457,#4894,.T.);
#10255=EDGE_CURVE('',#8457,#8457,#7663,.T.);
#10256=EDGE_CURVE('',#8458,#8458,#7664,.T.);
#10257=EDGE_CURVE('',#8458,#8459,#4895,.T.);
#10258=EDGE_CURVE('',#8459,#8459,#7665,.T.);
#10259=EDGE_CURVE('',#8460,#8460,#7666,.T.);
#10260=EDGE_CURVE('',#8460,#8461,#4896,.T.);
#10261=EDGE_CURVE('',#8461,#8461,#7667,.T.);
#10262=EDGE_CURVE('',#8462,#8462,#7668,.T.);
#10263=EDGE_CURVE('',#8462,#8463,#4897,.T.);
#10264=EDGE_CURVE('',#8463,#8463,#7669,.T.);
#10265=EDGE_CURVE('',#8464,#8464,#7670,.T.);
#10266=EDGE_CURVE('',#8464,#8465,#4898,.T.);
#10267=EDGE_CURVE('',#8465,#8465,#7671,.T.);
#10268=EDGE_CURVE('',#8466,#8466,#7672,.T.);
#10269=EDGE_CURVE('',#8466,#8467,#4899,.T.);
#10270=EDGE_CURVE('',#8467,#8467,#7673,.T.);
#10271=EDGE_CURVE('',#8468,#8468,#7674,.T.);
#10272=EDGE_CURVE('',#8468,#8469,#4900,.T.);
#10273=EDGE_CURVE('',#8469,#8469,#7675,.T.);
#10274=EDGE_CURVE('',#8470,#8470,#7676,.T.);
#10275=EDGE_CURVE('',#8470,#8471,#4901,.T.);
#10276=EDGE_CURVE('',#8471,#8471,#7677,.T.);
#10277=EDGE_CURVE('',#8472,#8472,#7678,.T.);
#10278=EDGE_CURVE('',#8472,#8473,#4902,.T.);
#10279=EDGE_CURVE('',#8473,#8473,#7679,.T.);
#10280=EDGE_CURVE('',#8474,#8474,#7680,.T.);
#10281=EDGE_CURVE('',#8474,#8475,#4903,.T.);
#10282=EDGE_CURVE('',#8475,#8475,#7681,.T.);
#10283=EDGE_CURVE('',#8476,#8476,#7682,.T.);
#10284=EDGE_CURVE('',#8477,#8477,#7683,.T.);
#10285=EDGE_CURVE('',#8477,#8478,#4904,.T.);
#10286=EDGE_CURVE('',#8478,#8478,#7684,.T.);
#10287=EDGE_CURVE('',#8479,#8479,#7685,.T.);
#10288=EDGE_CURVE('',#8480,#8480,#7686,.T.);
#10289=EDGE_CURVE('',#8480,#8481,#4905,.T.);
#10290=EDGE_CURVE('',#8481,#8481,#7687,.T.);
#10291=EDGE_CURVE('',#8482,#8482,#7688,.T.);
#10292=EDGE_CURVE('',#8483,#8483,#7689,.T.);
#10293=EDGE_CURVE('',#8483,#8484,#4906,.T.);
#10294=EDGE_CURVE('',#8484,#8484,#7690,.T.);
#10295=EDGE_CURVE('',#8485,#8485,#7691,.T.);
#10296=EDGE_CURVE('',#8486,#8486,#7692,.T.);
#10297=EDGE_CURVE('',#8486,#8476,#4907,.T.);
#10298=EDGE_CURVE('',#8487,#8487,#7693,.T.);
#10299=EDGE_CURVE('',#8487,#8479,#4908,.T.);
#10300=EDGE_CURVE('',#8488,#8488,#7694,.T.);
#10301=EDGE_CURVE('',#8488,#8482,#4909,.T.);
#10302=EDGE_CURVE('',#8489,#8489,#7695,.T.);
#10303=EDGE_CURVE('',#8489,#8485,#4910,.T.);
#10304=EDGE_CURVE('',#8490,#8490,#7696,.T.);
#10305=EDGE_CURVE('',#8490,#8491,#4911,.T.);
#10306=EDGE_CURVE('',#8491,#8491,#7697,.T.);
#10307=EDGE_CURVE('',#8492,#8493,#4912,.T.);
#10308=EDGE_CURVE('',#8492,#8494,#4913,.T.);
#10309=EDGE_CURVE('',#8494,#8495,#4914,.T.);
#10310=EDGE_CURVE('',#8493,#8495,#4915,.T.);
#10311=EDGE_CURVE('',#8493,#8496,#4916,.T.);
#10312=EDGE_CURVE('',#8495,#8497,#4917,.T.);
#10313=EDGE_CURVE('',#8496,#8497,#4918,.T.);
#10314=EDGE_CURVE('',#8496,#8498,#4919,.T.);
#10315=EDGE_CURVE('',#8497,#8499,#4920,.T.);
#10316=EDGE_CURVE('',#8498,#8499,#4921,.T.);
#10317=EDGE_CURVE('',#8498,#8492,#4922,.T.);
#10318=EDGE_CURVE('',#8499,#8494,#4923,.T.);
#10319=EDGE_CURVE('',#8500,#8501,#4924,.T.);
#10320=EDGE_CURVE('',#8500,#8502,#4925,.T.);
#10321=EDGE_CURVE('',#8502,#8503,#4926,.T.);
#10322=EDGE_CURVE('',#8501,#8503,#4927,.T.);
#10323=EDGE_CURVE('',#8501,#8504,#4928,.T.);
#10324=EDGE_CURVE('',#8503,#8505,#4929,.T.);
#10325=EDGE_CURVE('',#8504,#8505,#4930,.T.);
#10326=EDGE_CURVE('',#8504,#8506,#4931,.T.);
#10327=EDGE_CURVE('',#8505,#8507,#4932,.T.);
#10328=EDGE_CURVE('',#8506,#8507,#4933,.T.);
#10329=EDGE_CURVE('',#8506,#8500,#4934,.T.);
#10330=EDGE_CURVE('',#8507,#8502,#4935,.T.);
#10331=EDGE_CURVE('',#8508,#8509,#4936,.T.);
#10332=EDGE_CURVE('',#8508,#8510,#4937,.T.);
#10333=EDGE_CURVE('',#8510,#8511,#4938,.T.);
#10334=EDGE_CURVE('',#8509,#8511,#4939,.T.);
#10335=EDGE_CURVE('',#8509,#8512,#4940,.T.);
#10336=EDGE_CURVE('',#8511,#8513,#4941,.T.);
#10337=EDGE_CURVE('',#8512,#8513,#4942,.T.);
#10338=EDGE_CURVE('',#8512,#8514,#4943,.T.);
#10339=EDGE_CURVE('',#8513,#8515,#4944,.T.);
#10340=EDGE_CURVE('',#8514,#8515,#4945,.T.);
#10341=EDGE_CURVE('',#8514,#8508,#4946,.T.);
#10342=EDGE_CURVE('',#8515,#8510,#4947,.T.);
#10343=EDGE_CURVE('',#8516,#8517,#4948,.T.);
#10344=EDGE_CURVE('',#8516,#8518,#4949,.T.);
#10345=EDGE_CURVE('',#8518,#8519,#4950,.T.);
#10346=EDGE_CURVE('',#8517,#8519,#4951,.T.);
#10347=EDGE_CURVE('',#8517,#8520,#4952,.T.);
#10348=EDGE_CURVE('',#8519,#8521,#4953,.T.);
#10349=EDGE_CURVE('',#8520,#8521,#4954,.T.);
#10350=EDGE_CURVE('',#8520,#8522,#4955,.T.);
#10351=EDGE_CURVE('',#8521,#8523,#4956,.T.);
#10352=EDGE_CURVE('',#8522,#8523,#4957,.T.);
#10353=EDGE_CURVE('',#8522,#8516,#4958,.T.);
#10354=EDGE_CURVE('',#8523,#8518,#4959,.T.);
#10355=EDGE_CURVE('',#8524,#8525,#4960,.T.);
#10356=EDGE_CURVE('',#8524,#8526,#4961,.T.);
#10357=EDGE_CURVE('',#8526,#8527,#4962,.T.);
#10358=EDGE_CURVE('',#8525,#8527,#4963,.T.);
#10359=EDGE_CURVE('',#8525,#8528,#4964,.T.);
#10360=EDGE_CURVE('',#8527,#8529,#4965,.T.);
#10361=EDGE_CURVE('',#8528,#8529,#4966,.T.);
#10362=EDGE_CURVE('',#8528,#8530,#4967,.T.);
#10363=EDGE_CURVE('',#8529,#8531,#4968,.T.);
#10364=EDGE_CURVE('',#8530,#8531,#4969,.T.);
#10365=EDGE_CURVE('',#8530,#8524,#4970,.T.);
#10366=EDGE_CURVE('',#8531,#8526,#4971,.T.);
#10367=EDGE_CURVE('',#8532,#8533,#4972,.T.);
#10368=EDGE_CURVE('',#8532,#8534,#4973,.T.);
#10369=EDGE_CURVE('',#8534,#8535,#4974,.T.);
#10370=EDGE_CURVE('',#8533,#8535,#4975,.T.);
#10371=EDGE_CURVE('',#8533,#8536,#4976,.T.);
#10372=EDGE_CURVE('',#8535,#8537,#4977,.T.);
#10373=EDGE_CURVE('',#8536,#8537,#4978,.T.);
#10374=EDGE_CURVE('',#8536,#8538,#4979,.T.);
#10375=EDGE_CURVE('',#8537,#8539,#4980,.T.);
#10376=EDGE_CURVE('',#8538,#8539,#4981,.T.);
#10377=EDGE_CURVE('',#8538,#8532,#4982,.T.);
#10378=EDGE_CURVE('',#8539,#8534,#4983,.T.);
#10379=EDGE_CURVE('',#8540,#8541,#4984,.T.);
#10380=EDGE_CURVE('',#8540,#8542,#4985,.T.);
#10381=EDGE_CURVE('',#8542,#8543,#4986,.T.);
#10382=EDGE_CURVE('',#8541,#8543,#4987,.T.);
#10383=EDGE_CURVE('',#8541,#8544,#4988,.T.);
#10384=EDGE_CURVE('',#8543,#8545,#4989,.T.);
#10385=EDGE_CURVE('',#8544,#8545,#4990,.T.);
#10386=EDGE_CURVE('',#8544,#8546,#4991,.T.);
#10387=EDGE_CURVE('',#8545,#8547,#4992,.T.);
#10388=EDGE_CURVE('',#8546,#8547,#4993,.T.);
#10389=EDGE_CURVE('',#8546,#8540,#4994,.T.);
#10390=EDGE_CURVE('',#8547,#8542,#4995,.T.);
#10391=EDGE_CURVE('',#8548,#8549,#4996,.T.);
#10392=EDGE_CURVE('',#8548,#8550,#4997,.T.);
#10393=EDGE_CURVE('',#8550,#8551,#4998,.T.);
#10394=EDGE_CURVE('',#8549,#8551,#4999,.T.);
#10395=EDGE_CURVE('',#8549,#8552,#5000,.T.);
#10396=EDGE_CURVE('',#8551,#8553,#5001,.T.);
#10397=EDGE_CURVE('',#8552,#8553,#5002,.T.);
#10398=EDGE_CURVE('',#8552,#8554,#5003,.T.);
#10399=EDGE_CURVE('',#8553,#8555,#5004,.T.);
#10400=EDGE_CURVE('',#8554,#8555,#5005,.T.);
#10401=EDGE_CURVE('',#8554,#8548,#5006,.T.);
#10402=EDGE_CURVE('',#8555,#8550,#5007,.T.);
#10403=EDGE_CURVE('',#8556,#8557,#5008,.T.);
#10404=EDGE_CURVE('',#8556,#8558,#5009,.T.);
#10405=EDGE_CURVE('',#8558,#8559,#5010,.T.);
#10406=EDGE_CURVE('',#8557,#8559,#5011,.T.);
#10407=EDGE_CURVE('',#8557,#8560,#5012,.T.);
#10408=EDGE_CURVE('',#8559,#8561,#5013,.T.);
#10409=EDGE_CURVE('',#8560,#8561,#5014,.T.);
#10410=EDGE_CURVE('',#8560,#8562,#5015,.T.);
#10411=EDGE_CURVE('',#8561,#8563,#5016,.T.);
#10412=EDGE_CURVE('',#8562,#8563,#5017,.T.);
#10413=EDGE_CURVE('',#8562,#8556,#5018,.T.);
#10414=EDGE_CURVE('',#8563,#8558,#5019,.T.);
#10415=EDGE_CURVE('',#8564,#8565,#5020,.T.);
#10416=EDGE_CURVE('',#8564,#8566,#5021,.T.);
#10417=EDGE_CURVE('',#8566,#8567,#5022,.T.);
#10418=EDGE_CURVE('',#8565,#8567,#5023,.T.);
#10419=EDGE_CURVE('',#8565,#8568,#5024,.T.);
#10420=EDGE_CURVE('',#8567,#8569,#5025,.T.);
#10421=EDGE_CURVE('',#8568,#8569,#5026,.T.);
#10422=EDGE_CURVE('',#8568,#8570,#5027,.T.);
#10423=EDGE_CURVE('',#8569,#8571,#5028,.T.);
#10424=EDGE_CURVE('',#8570,#8571,#5029,.T.);
#10425=EDGE_CURVE('',#8570,#8564,#5030,.T.);
#10426=EDGE_CURVE('',#8571,#8566,#5031,.T.);
#10427=EDGE_CURVE('',#8572,#8573,#5032,.T.);
#10428=EDGE_CURVE('',#8572,#8574,#5033,.T.);
#10429=EDGE_CURVE('',#8574,#8575,#5034,.T.);
#10430=EDGE_CURVE('',#8573,#8575,#5035,.T.);
#10431=EDGE_CURVE('',#8573,#8576,#5036,.T.);
#10432=EDGE_CURVE('',#8575,#8577,#5037,.T.);
#10433=EDGE_CURVE('',#8576,#8577,#5038,.T.);
#10434=EDGE_CURVE('',#8576,#8578,#5039,.T.);
#10435=EDGE_CURVE('',#8577,#8579,#5040,.T.);
#10436=EDGE_CURVE('',#8578,#8579,#5041,.T.);
#10437=EDGE_CURVE('',#8578,#8572,#5042,.T.);
#10438=EDGE_CURVE('',#8579,#8574,#5043,.T.);
#10439=EDGE_CURVE('',#8580,#8581,#5044,.T.);
#10440=EDGE_CURVE('',#8580,#8582,#5045,.T.);
#10441=EDGE_CURVE('',#8582,#8583,#5046,.T.);
#10442=EDGE_CURVE('',#8581,#8583,#5047,.T.);
#10443=EDGE_CURVE('',#8581,#8584,#5048,.T.);
#10444=EDGE_CURVE('',#8583,#8585,#5049,.T.);
#10445=EDGE_CURVE('',#8584,#8585,#5050,.T.);
#10446=EDGE_CURVE('',#8584,#8586,#5051,.T.);
#10447=EDGE_CURVE('',#8585,#8587,#5052,.T.);
#10448=EDGE_CURVE('',#8586,#8587,#5053,.T.);
#10449=EDGE_CURVE('',#8586,#8580,#5054,.T.);
#10450=EDGE_CURVE('',#8587,#8582,#5055,.T.);
#10451=EDGE_CURVE('',#8588,#8589,#5056,.T.);
#10452=EDGE_CURVE('',#8588,#8590,#5057,.T.);
#10453=EDGE_CURVE('',#8590,#8591,#5058,.T.);
#10454=EDGE_CURVE('',#8589,#8591,#5059,.T.);
#10455=EDGE_CURVE('',#8589,#8592,#5060,.T.);
#10456=EDGE_CURVE('',#8591,#8593,#5061,.T.);
#10457=EDGE_CURVE('',#8592,#8593,#5062,.T.);
#10458=EDGE_CURVE('',#8592,#8594,#5063,.T.);
#10459=EDGE_CURVE('',#8593,#8595,#5064,.T.);
#10460=EDGE_CURVE('',#8594,#8595,#5065,.T.);
#10461=EDGE_CURVE('',#8594,#8588,#5066,.T.);
#10462=EDGE_CURVE('',#8595,#8590,#5067,.T.);
#10463=EDGE_CURVE('',#8596,#8597,#5068,.T.);
#10464=EDGE_CURVE('',#8596,#8598,#5069,.T.);
#10465=EDGE_CURVE('',#8598,#8599,#5070,.T.);
#10466=EDGE_CURVE('',#8597,#8599,#5071,.T.);
#10467=EDGE_CURVE('',#8597,#8600,#5072,.T.);
#10468=EDGE_CURVE('',#8599,#8601,#5073,.T.);
#10469=EDGE_CURVE('',#8600,#8601,#5074,.T.);
#10470=EDGE_CURVE('',#8600,#8602,#5075,.T.);
#10471=EDGE_CURVE('',#8601,#8603,#5076,.T.);
#10472=EDGE_CURVE('',#8602,#8603,#5077,.T.);
#10473=EDGE_CURVE('',#8602,#8596,#5078,.T.);
#10474=EDGE_CURVE('',#8603,#8598,#5079,.T.);
#10475=EDGE_CURVE('',#8604,#8605,#5080,.T.);
#10476=EDGE_CURVE('',#8604,#8606,#5081,.T.);
#10477=EDGE_CURVE('',#8606,#8607,#5082,.T.);
#10478=EDGE_CURVE('',#8605,#8607,#5083,.T.);
#10479=EDGE_CURVE('',#8605,#8608,#5084,.T.);
#10480=EDGE_CURVE('',#8607,#8609,#5085,.T.);
#10481=EDGE_CURVE('',#8608,#8609,#5086,.T.);
#10482=EDGE_CURVE('',#8608,#8610,#5087,.T.);
#10483=EDGE_CURVE('',#8609,#8611,#5088,.T.);
#10484=EDGE_CURVE('',#8610,#8611,#5089,.T.);
#10485=EDGE_CURVE('',#8610,#8604,#5090,.T.);
#10486=EDGE_CURVE('',#8611,#8606,#5091,.T.);
#10487=EDGE_CURVE('',#8612,#8613,#5092,.T.);
#10488=EDGE_CURVE('',#8612,#8614,#5093,.T.);
#10489=EDGE_CURVE('',#8614,#8615,#5094,.T.);
#10490=EDGE_CURVE('',#8613,#8615,#5095,.T.);
#10491=EDGE_CURVE('',#8613,#8616,#5096,.T.);
#10492=EDGE_CURVE('',#8615,#8617,#5097,.T.);
#10493=EDGE_CURVE('',#8616,#8617,#5098,.T.);
#10494=EDGE_CURVE('',#8616,#8618,#5099,.T.);
#10495=EDGE_CURVE('',#8617,#8619,#5100,.T.);
#10496=EDGE_CURVE('',#8618,#8619,#5101,.T.);
#10497=EDGE_CURVE('',#8618,#8612,#5102,.T.);
#10498=EDGE_CURVE('',#8619,#8614,#5103,.T.);
#10499=EDGE_CURVE('',#8620,#8621,#5104,.T.);
#10500=EDGE_CURVE('',#8620,#8622,#5105,.T.);
#10501=EDGE_CURVE('',#8622,#8623,#5106,.T.);
#10502=EDGE_CURVE('',#8621,#8623,#5107,.T.);
#10503=EDGE_CURVE('',#8621,#8624,#5108,.T.);
#10504=EDGE_CURVE('',#8623,#8625,#5109,.T.);
#10505=EDGE_CURVE('',#8624,#8625,#5110,.T.);
#10506=EDGE_CURVE('',#8624,#8626,#5111,.T.);
#10507=EDGE_CURVE('',#8625,#8627,#5112,.T.);
#10508=EDGE_CURVE('',#8626,#8627,#5113,.T.);
#10509=EDGE_CURVE('',#8626,#8620,#5114,.T.);
#10510=EDGE_CURVE('',#8627,#8622,#5115,.T.);
#10511=EDGE_CURVE('',#8628,#8629,#5116,.T.);
#10512=EDGE_CURVE('',#8628,#8630,#5117,.T.);
#10513=EDGE_CURVE('',#8630,#8631,#5118,.T.);
#10514=EDGE_CURVE('',#8629,#8631,#5119,.T.);
#10515=EDGE_CURVE('',#8629,#8632,#5120,.T.);
#10516=EDGE_CURVE('',#8631,#8633,#5121,.T.);
#10517=EDGE_CURVE('',#8632,#8633,#5122,.T.);
#10518=EDGE_CURVE('',#8632,#8634,#5123,.T.);
#10519=EDGE_CURVE('',#8633,#8635,#5124,.T.);
#10520=EDGE_CURVE('',#8634,#8635,#5125,.T.);
#10521=EDGE_CURVE('',#8634,#8628,#5126,.T.);
#10522=EDGE_CURVE('',#8635,#8630,#5127,.T.);
#10523=EDGE_CURVE('',#8636,#8637,#5128,.T.);
#10524=EDGE_CURVE('',#8636,#8638,#5129,.T.);
#10525=EDGE_CURVE('',#8638,#8639,#5130,.T.);
#10526=EDGE_CURVE('',#8637,#8639,#5131,.T.);
#10527=EDGE_CURVE('',#8637,#8640,#5132,.T.);
#10528=EDGE_CURVE('',#8639,#8641,#5133,.T.);
#10529=EDGE_CURVE('',#8640,#8641,#5134,.T.);
#10530=EDGE_CURVE('',#8640,#8642,#5135,.T.);
#10531=EDGE_CURVE('',#8641,#8643,#5136,.T.);
#10532=EDGE_CURVE('',#8642,#8643,#5137,.T.);
#10533=EDGE_CURVE('',#8642,#8636,#5138,.T.);
#10534=EDGE_CURVE('',#8643,#8638,#5139,.T.);
#10535=EDGE_CURVE('',#8644,#8645,#5140,.T.);
#10536=EDGE_CURVE('',#8644,#8646,#5141,.T.);
#10537=EDGE_CURVE('',#8646,#8647,#5142,.T.);
#10538=EDGE_CURVE('',#8645,#8647,#5143,.T.);
#10539=EDGE_CURVE('',#8645,#8648,#5144,.T.);
#10540=EDGE_CURVE('',#8647,#8649,#5145,.T.);
#10541=EDGE_CURVE('',#8648,#8649,#5146,.T.);
#10542=EDGE_CURVE('',#8648,#8650,#5147,.T.);
#10543=EDGE_CURVE('',#8649,#8651,#5148,.T.);
#10544=EDGE_CURVE('',#8650,#8651,#5149,.T.);
#10545=EDGE_CURVE('',#8650,#8644,#5150,.T.);
#10546=EDGE_CURVE('',#8651,#8646,#5151,.T.);
#10547=EDGE_CURVE('',#8652,#8653,#5152,.T.);
#10548=EDGE_CURVE('',#8652,#8654,#5153,.T.);
#10549=EDGE_CURVE('',#8654,#8655,#5154,.T.);
#10550=EDGE_CURVE('',#8653,#8655,#5155,.T.);
#10551=EDGE_CURVE('',#8653,#8656,#5156,.T.);
#10552=EDGE_CURVE('',#8655,#8657,#5157,.T.);
#10553=EDGE_CURVE('',#8656,#8657,#5158,.T.);
#10554=EDGE_CURVE('',#8656,#8658,#5159,.T.);
#10555=EDGE_CURVE('',#8657,#8659,#5160,.T.);
#10556=EDGE_CURVE('',#8658,#8659,#5161,.T.);
#10557=EDGE_CURVE('',#8658,#8652,#5162,.T.);
#10558=EDGE_CURVE('',#8659,#8654,#5163,.T.);
#10559=EDGE_CURVE('',#8660,#8661,#5164,.T.);
#10560=EDGE_CURVE('',#8660,#8662,#5165,.T.);
#10561=EDGE_CURVE('',#8662,#8663,#5166,.T.);
#10562=EDGE_CURVE('',#8661,#8663,#5167,.T.);
#10563=EDGE_CURVE('',#8661,#8664,#5168,.T.);
#10564=EDGE_CURVE('',#8663,#8665,#5169,.T.);
#10565=EDGE_CURVE('',#8664,#8665,#5170,.T.);
#10566=EDGE_CURVE('',#8664,#8666,#5171,.T.);
#10567=EDGE_CURVE('',#8665,#8667,#5172,.T.);
#10568=EDGE_CURVE('',#8666,#8667,#5173,.T.);
#10569=EDGE_CURVE('',#8666,#8660,#5174,.T.);
#10570=EDGE_CURVE('',#8667,#8662,#5175,.T.);
#10571=EDGE_CURVE('',#8668,#8669,#5176,.T.);
#10572=EDGE_CURVE('',#8668,#8670,#5177,.T.);
#10573=EDGE_CURVE('',#8670,#8671,#5178,.T.);
#10574=EDGE_CURVE('',#8669,#8671,#5179,.T.);
#10575=EDGE_CURVE('',#8669,#8672,#5180,.T.);
#10576=EDGE_CURVE('',#8671,#8673,#5181,.T.);
#10577=EDGE_CURVE('',#8672,#8673,#5182,.T.);
#10578=EDGE_CURVE('',#8672,#8674,#5183,.T.);
#10579=EDGE_CURVE('',#8673,#8675,#5184,.T.);
#10580=EDGE_CURVE('',#8674,#8675,#5185,.T.);
#10581=EDGE_CURVE('',#8674,#8668,#5186,.T.);
#10582=EDGE_CURVE('',#8675,#8670,#5187,.T.);
#10583=EDGE_CURVE('',#8676,#8677,#5188,.T.);
#10584=EDGE_CURVE('',#8676,#8678,#5189,.T.);
#10585=EDGE_CURVE('',#8678,#8679,#5190,.T.);
#10586=EDGE_CURVE('',#8677,#8679,#5191,.T.);
#10587=EDGE_CURVE('',#8677,#8680,#5192,.T.);
#10588=EDGE_CURVE('',#8679,#8681,#5193,.T.);
#10589=EDGE_CURVE('',#8680,#8681,#5194,.T.);
#10590=EDGE_CURVE('',#8680,#8682,#5195,.T.);
#10591=EDGE_CURVE('',#8681,#8683,#5196,.T.);
#10592=EDGE_CURVE('',#8682,#8683,#5197,.T.);
#10593=EDGE_CURVE('',#8682,#8676,#5198,.T.);
#10594=EDGE_CURVE('',#8683,#8678,#5199,.T.);
#10595=EDGE_CURVE('',#8684,#8685,#5200,.T.);
#10596=EDGE_CURVE('',#8684,#8686,#5201,.T.);
#10597=EDGE_CURVE('',#8686,#8687,#5202,.T.);
#10598=EDGE_CURVE('',#8685,#8687,#5203,.T.);
#10599=EDGE_CURVE('',#8685,#8688,#5204,.T.);
#10600=EDGE_CURVE('',#8687,#8689,#5205,.T.);
#10601=EDGE_CURVE('',#8688,#8689,#5206,.T.);
#10602=EDGE_CURVE('',#8688,#8690,#5207,.T.);
#10603=EDGE_CURVE('',#8689,#8691,#5208,.T.);
#10604=EDGE_CURVE('',#8690,#8691,#5209,.T.);
#10605=EDGE_CURVE('',#8690,#8684,#5210,.T.);
#10606=EDGE_CURVE('',#8691,#8686,#5211,.T.);
#10607=EDGE_CURVE('',#8692,#8692,#7698,.T.);
#10608=EDGE_CURVE('',#8692,#8693,#5212,.T.);
#10609=EDGE_CURVE('',#8693,#8693,#7699,.T.);
#10610=EDGE_CURVE('',#8694,#8694,#7700,.T.);
#10611=EDGE_CURVE('',#8694,#8695,#5213,.T.);
#10612=EDGE_CURVE('',#8695,#8695,#7701,.T.);
#10613=EDGE_CURVE('',#8696,#8697,#5214,.T.);
#10614=EDGE_CURVE('',#8697,#8698,#5215,.T.);
#10615=EDGE_CURVE('',#8699,#8698,#5216,.T.);
#10616=EDGE_CURVE('',#8696,#8699,#5217,.T.);
#10617=EDGE_CURVE('',#8700,#8696,#5218,.T.);
#10618=EDGE_CURVE('',#8701,#8699,#5219,.T.);
#10619=EDGE_CURVE('',#8700,#8701,#5220,.T.);
#10620=EDGE_CURVE('',#8702,#8700,#5221,.T.);
#10621=EDGE_CURVE('',#8703,#8701,#5222,.T.);
#10622=EDGE_CURVE('',#8702,#8703,#5223,.T.);
#10623=EDGE_CURVE('',#8697,#8702,#5224,.T.);
#10624=EDGE_CURVE('',#8698,#8703,#5225,.T.);
#10625=EDGE_CURVE('',#8704,#8704,#7702,.T.);
#10626=EDGE_CURVE('',#8704,#8705,#5226,.T.);
#10627=EDGE_CURVE('',#8705,#8705,#7703,.T.);
#10628=EDGE_CURVE('',#8706,#8706,#7704,.T.);
#10629=EDGE_CURVE('',#8706,#8704,#5227,.T.);
#10630=EDGE_CURVE('',#8707,#8707,#7705,.T.);
#10631=EDGE_CURVE('',#8707,#8706,#5228,.T.);
#10632=EDGE_CURVE('',#8708,#8709,#5229,.T.);
#10633=EDGE_CURVE('',#8709,#8708,#7706,.T.);
#10634=EDGE_CURVE('',#8710,#8708,#5230,.T.);
#10635=EDGE_CURVE('',#8711,#8710,#7707,.T.);
#10636=EDGE_CURVE('',#8709,#8711,#5231,.T.);
#10637=EDGE_CURVE('',#8712,#8713,#5232,.T.);
#10638=EDGE_CURVE('',#8712,#8714,#7708,.T.);
#10639=EDGE_CURVE('',#8715,#8714,#5233,.T.);
#10640=EDGE_CURVE('',#8713,#8715,#7709,.T.);
#10641=EDGE_CURVE('',#8714,#8712,#5234,.T.);
#10642=EDGE_CURVE('',#8710,#8716,#5235,.T.);
#10643=EDGE_CURVE('',#8717,#8716,#5236,.T.);
#10644=EDGE_CURVE('',#8717,#8718,#5237,.T.);
#10645=EDGE_CURVE('',#8719,#8718,#5238,.T.);
#10646=EDGE_CURVE('',#8719,#8711,#5239,.T.);
#10647=EDGE_CURVE('',#8720,#8720,#7710,.T.);
#10648=EDGE_CURVE('',#8721,#8719,#5240,.T.);
#10649=EDGE_CURVE('',#8721,#8722,#5241,.T.);
#10650=EDGE_CURVE('',#8716,#8722,#5242,.T.);
#10651=EDGE_CURVE('',#8723,#8723,#7711,.T.);
#10652=EDGE_CURVE('',#8724,#8725,#5243,.T.);
#10653=EDGE_CURVE('',#8726,#8725,#5244,.T.);
#10654=EDGE_CURVE('',#8713,#8726,#5245,.T.);
#10655=EDGE_CURVE('',#8727,#8715,#5246,.T.);
#10656=EDGE_CURVE('',#8724,#8727,#5247,.T.);
#10657=EDGE_CURVE('',#8728,#8728,#7712,.T.);
#10658=EDGE_CURVE('',#8729,#8729,#7713,.T.);
#10659=EDGE_CURVE('',#8729,#8730,#5248,.T.);
#10660=EDGE_CURVE('',#8730,#8730,#7714,.T.);
#10661=EDGE_CURVE('',#8723,#8731,#5249,.T.);
#10662=EDGE_CURVE('',#8731,#8731,#7715,.T.);
#10663=EDGE_CURVE('',#8732,#8732,#7716,.T.);
#10664=EDGE_CURVE('',#8732,#8720,#5250,.T.);
#10665=EDGE_CURVE('',#8733,#8733,#7717,.T.);
#10666=EDGE_CURVE('',#8733,#8728,#5251,.T.);
#10667=EDGE_CURVE('',#8734,#8734,#7718,.T.);
#10668=EDGE_CURVE('',#8734,#8735,#5252,.T.);
#10669=EDGE_CURVE('',#8735,#8735,#7719,.T.);
#10670=EDGE_CURVE('',#8718,#8736,#5253,.T.);
#10671=EDGE_CURVE('',#8736,#8737,#5254,.T.);
#10672=EDGE_CURVE('',#8737,#8724,#5255,.T.);
#10673=EDGE_CURVE('',#8727,#8738,#5256,.T.);
#10674=EDGE_CURVE('',#8738,#8739,#5257,.T.);
#10675=EDGE_CURVE('',#8739,#8740,#5258,.T.);
#10676=EDGE_CURVE('',#8740,#8741,#5259,.T.);
#10677=EDGE_CURVE('',#8741,#8742,#5260,.T.);
#10678=EDGE_CURVE('',#8742,#8721,#5261,.T.);
#10679=EDGE_CURVE('',#8743,#8717,#5262,.T.);
#10680=EDGE_CURVE('',#8736,#8743,#5263,.T.);
#10681=EDGE_CURVE('',#8744,#8743,#5264,.T.);
#10682=EDGE_CURVE('',#8737,#8744,#5265,.T.);
#10683=EDGE_CURVE('',#8725,#8744,#5266,.T.);
#10684=EDGE_CURVE('',#8745,#8726,#5267,.T.);
#10685=EDGE_CURVE('',#8738,#8745,#5268,.T.);
#10686=EDGE_CURVE('',#8746,#8745,#5269,.T.);
#10687=EDGE_CURVE('',#8739,#8746,#5270,.T.);
#10688=EDGE_CURVE('',#8747,#8746,#5271,.T.);
#10689=EDGE_CURVE('',#8740,#8747,#5272,.T.);
#10690=EDGE_CURVE('',#8748,#8747,#5273,.T.);
#10691=EDGE_CURVE('',#8741,#8748,#5274,.T.);
#10692=EDGE_CURVE('',#8749,#8748,#5275,.T.);
#10693=EDGE_CURVE('',#8742,#8749,#5276,.T.);
#10694=EDGE_CURVE('',#8722,#8749,#5277,.T.);
#10695=EDGE_CURVE('',#8750,#8751,#5278,.T.);
#10696=EDGE_CURVE('',#8751,#8752,#5279,.T.);
#10697=EDGE_CURVE('',#8752,#8753,#5280,.T.);
#10698=EDGE_CURVE('',#8750,#8753,#5281,.T.);
#10699=EDGE_CURVE('',#8751,#8754,#5282,.T.);
#10700=EDGE_CURVE('',#8754,#8755,#5283,.T.);
#10701=EDGE_CURVE('',#8755,#8752,#5284,.T.);
#10702=EDGE_CURVE('',#8754,#8756,#5285,.T.);
#10703=EDGE_CURVE('',#8756,#8757,#5286,.T.);
#10704=EDGE_CURVE('',#8757,#8755,#5287,.T.);
#10705=EDGE_CURVE('',#8756,#8758,#5288,.T.);
#10706=EDGE_CURVE('',#8758,#8759,#5289,.T.);
#10707=EDGE_CURVE('',#8759,#8757,#5290,.T.);
#10708=EDGE_CURVE('',#8758,#8760,#5291,.T.);
#10709=EDGE_CURVE('',#8760,#8761,#5292,.T.);
#10710=EDGE_CURVE('',#8761,#8759,#5293,.T.);
#10711=EDGE_CURVE('',#8760,#8750,#5294,.T.);
#10712=EDGE_CURVE('',#8753,#8761,#5295,.T.);
#10713=EDGE_CURVE('',#8762,#8762,#7720,.T.);
#10714=EDGE_CURVE('',#8763,#8763,#7721,.T.);
#10715=EDGE_CURVE('',#8764,#8764,#7722,.T.);
#10716=EDGE_CURVE('',#8764,#8763,#5296,.T.);
#10717=EDGE_CURVE('',#8765,#8765,#7723,.T.);
#10718=EDGE_CURVE('',#8765,#8764,#5297,.T.);
#10719=EDGE_CURVE('',#8766,#8766,#7724,.T.);
#10720=EDGE_CURVE('',#8766,#8765,#5298,.T.);
#10721=EDGE_CURVE('',#8767,#8767,#7725,.T.);
#10722=EDGE_CURVE('',#8768,#8768,#7726,.F.);
#10723=EDGE_CURVE('',#8768,#8767,#5299,.T.);
#10724=EDGE_CURVE('',#8762,#8768,#5300,.T.);
#10725=EDGE_CURVE('',#8769,#8770,#7727,.T.);
#10726=EDGE_CURVE('',#8770,#8769,#7728,.T.);
#10727=EDGE_CURVE('',#8770,#8771,#7729,.T.);
#10728=EDGE_CURVE('',#8772,#8771,#7730,.T.);
#10729=EDGE_CURVE('',#8771,#8772,#7731,.T.);
#10730=EDGE_CURVE('',#8772,#8773,#5301,.T.);
#10731=EDGE_CURVE('',#8773,#8773,#7732,.T.);
#10732=EDGE_CURVE('',#8774,#8774,#7733,.T.);
#10733=EDGE_CURVE('',#8774,#8775,#5302,.T.);
#10734=EDGE_CURVE('',#8775,#8775,#7734,.T.);
#10735=EDGE_CURVE('',#8775,#8776,#5303,.T.);
#10736=EDGE_CURVE('',#8776,#8776,#7735,.T.);
#10737=EDGE_CURVE('',#8777,#8777,#7736,.T.);
#10738=EDGE_CURVE('',#8777,#8769,#5304,.T.);
#10739=EDGE_CURVE('',#8778,#8778,#7737,.T.);
#10740=EDGE_CURVE('',#8778,#8774,#5305,.T.);
#10741=EDGE_CURVE('',#8779,#8780,#7738,.T.);
#10742=EDGE_CURVE('',#8780,#8779,#7739,.T.);
#10743=EDGE_CURVE('',#8780,#8781,#7740,.T.);
#10744=EDGE_CURVE('',#8782,#8781,#7741,.T.);
#10745=EDGE_CURVE('',#8781,#8782,#7742,.T.);
#10746=EDGE_CURVE('',#8783,#8783,#7743,.T.);
#10747=EDGE_CURVE('',#8783,#8782,#5306,.T.);
#10748=EDGE_CURVE('',#8784,#8784,#7744,.T.);
#10749=EDGE_CURVE('',#8785,#8785,#7745,.T.);
#10750=EDGE_CURVE('',#8786,#8786,#7746,.T.);
#10751=EDGE_CURVE('',#8786,#8784,#5307,.T.);
#10752=EDGE_CURVE('',#8787,#8787,#7747,.T.);
#10753=EDGE_CURVE('',#8787,#8786,#5308,.T.);
#10754=EDGE_CURVE('',#8788,#8788,#7748,.T.);
#10755=EDGE_CURVE('',#8788,#8787,#5309,.T.);
#10756=EDGE_CURVE('',#8779,#8785,#5310,.T.);
#10757=EDGE_CURVE('',#8789,#8790,#7749,.T.);
#10758=EDGE_CURVE('',#8791,#8792,#7750,.T.);
#10759=EDGE_CURVE('',#8793,#8794,#7751,.T.);
#10760=EDGE_CURVE('',#8795,#8796,#7752,.T.);
#10761=EDGE_CURVE('',#8797,#8798,#7753,.T.);
#10762=EDGE_CURVE('',#8799,#8800,#7754,.T.);
#10763=EDGE_CURVE('',#8801,#8802,#7755,.T.);
#10764=EDGE_CURVE('',#8803,#8804,#553,.T.);
#10765=EDGE_CURVE('',#8805,#8803,#7756,.T.);
#10766=EDGE_CURVE('',#8806,#8805,#554,.T.);
#10767=EDGE_CURVE('',#8804,#8806,#7757,.T.);
#10768=EDGE_CURVE('',#8807,#8805,#7758,.T.);
#10769=EDGE_CURVE('',#8807,#8808,#555,.T.);
#10770=EDGE_CURVE('',#8809,#8808,#7759,.T.);
#10771=EDGE_CURVE('',#8809,#8810,#556,.T.);
#10772=EDGE_CURVE('',#8811,#8810,#7760,.T.);
#10773=EDGE_CURVE('',#8811,#8812,#5311,.T.);
#10774=EDGE_CURVE('',#8812,#8812,#7761,.T.);
#10775=EDGE_CURVE('',#8813,#8811,#7762,.T.);
#10776=EDGE_CURVE('',#8813,#8814,#557,.T.);
#10777=EDGE_CURVE('',#8815,#8814,#7763,.T.);
#10778=EDGE_CURVE('',#8815,#8816,#558,.T.);
#10779=EDGE_CURVE('',#8817,#8816,#7764,.T.);
#10780=EDGE_CURVE('',#8817,#8818,#559,.T.);
#10781=EDGE_CURVE('',#8819,#8818,#7765,.T.);
#10782=EDGE_CURVE('',#8819,#8820,#560,.T.);
#10783=EDGE_CURVE('',#8806,#8820,#7766,.T.);
#10784=EDGE_CURVE('',#8803,#8821,#7767,.T.);
#10785=EDGE_CURVE('',#8821,#8807,#7768,.T.);
#10786=EDGE_CURVE('',#8822,#8821,#561,.T.);
#10787=EDGE_CURVE('',#8808,#8822,#7769,.T.);
#10788=EDGE_CURVE('',#8822,#8823,#7770,.T.);
#10789=EDGE_CURVE('',#8823,#8809,#7771,.T.);
#10790=EDGE_CURVE('',#8824,#8823,#562,.T.);
#10791=EDGE_CURVE('',#8810,#8824,#7772,.T.);
#10792=EDGE_CURVE('',#8824,#8825,#7773,.T.);
#10793=EDGE_CURVE('',#8825,#8826,#7774,.T.);
#10794=EDGE_CURVE('',#8826,#8813,#7775,.T.);
#10795=EDGE_CURVE('',#8827,#8826,#563,.T.);
#10796=EDGE_CURVE('',#8814,#8827,#7776,.T.);
#10797=EDGE_CURVE('',#8827,#8828,#7777,.T.);
#10798=EDGE_CURVE('',#8828,#8815,#7778,.T.);
#10799=EDGE_CURVE('',#8829,#8828,#564,.T.);
#10800=EDGE_CURVE('',#8816,#8829,#7779,.T.);
#10801=EDGE_CURVE('',#8829,#8830,#7780,.T.);
#10802=EDGE_CURVE('',#8830,#8817,#7781,.T.);
#10803=EDGE_CURVE('',#8831,#8830,#565,.T.);
#10804=EDGE_CURVE('',#8818,#8831,#7782,.T.);
#10805=EDGE_CURVE('',#8832,#8832,#7783,.T.);
#10806=EDGE_CURVE('',#8832,#8825,#5312,.T.);
#10807=EDGE_CURVE('',#8833,#8804,#7784,.T.);
#10808=EDGE_CURVE('',#8833,#8834,#566,.T.);
#10809=EDGE_CURVE('',#8831,#8834,#7785,.T.);
#10810=EDGE_CURVE('',#8820,#8833,#7786,.T.);
#10811=EDGE_CURVE('',#8834,#8819,#7787,.T.);
#10812=EDGE_CURVE('',#8835,#8835,#7788,.T.);
#10813=EDGE_CURVE('',#8836,#8836,#7789,.T.);
#10814=EDGE_CURVE('',#8837,#8837,#7790,.T.);
#10815=EDGE_CURVE('',#8837,#8835,#5313,.T.);
#10816=EDGE_CURVE('',#8838,#8838,#7791,.T.);
#10817=EDGE_CURVE('',#8838,#8836,#5314,.T.);
#10818=EDGE_CURVE('',#8839,#8839,#7792,.T.);
#10819=EDGE_CURVE('',#8840,#8840,#7793,.T.);
#10820=EDGE_CURVE('',#8841,#8841,#7794,.T.);
#10821=EDGE_CURVE('',#8841,#8839,#5315,.T.);
#10822=EDGE_CURVE('',#8842,#8842,#7795,.T.);
#10823=EDGE_CURVE('',#8842,#8840,#5316,.T.);
#10824=EDGE_CURVE('',#8843,#8844,#7796,.T.);
#10825=EDGE_CURVE('',#8844,#8843,#7797,.T.);
#10826=EDGE_CURVE('',#8844,#8845,#7798,.T.);
#10827=EDGE_CURVE('',#8846,#8845,#7799,.T.);
#10828=EDGE_CURVE('',#8845,#8846,#7800,.T.);
#10829=EDGE_CURVE('',#8846,#8847,#5317,.T.);
#10830=EDGE_CURVE('',#8847,#8847,#7801,.T.);
#10831=EDGE_CURVE('',#8848,#8848,#7802,.T.);
#10832=EDGE_CURVE('',#8848,#8849,#5318,.T.);
#10833=EDGE_CURVE('',#8849,#8849,#7803,.T.);
#10834=EDGE_CURVE('',#8849,#8850,#5319,.T.);
#10835=EDGE_CURVE('',#8850,#8850,#7804,.T.);
#10836=EDGE_CURVE('',#8851,#8851,#7805,.T.);
#10837=EDGE_CURVE('',#8851,#8843,#5320,.T.);
#10838=EDGE_CURVE('',#8852,#8852,#7806,.T.);
#10839=EDGE_CURVE('',#8852,#8848,#5321,.T.);
#10840=EDGE_CURVE('',#8853,#8854,#7807,.T.);
#10841=EDGE_CURVE('',#8854,#8853,#7808,.T.);
#10842=EDGE_CURVE('',#8854,#8855,#7809,.T.);
#10843=EDGE_CURVE('',#8856,#8855,#7810,.T.);
#10844=EDGE_CURVE('',#8855,#8856,#7811,.T.);
#10845=EDGE_CURVE('',#8857,#8857,#7812,.T.);
#10846=EDGE_CURVE('',#8857,#8856,#5322,.T.);
#10847=EDGE_CURVE('',#8858,#8858,#7813,.T.);
#10848=EDGE_CURVE('',#8859,#8859,#7814,.T.);
#10849=EDGE_CURVE('',#8860,#8860,#7815,.T.);
#10850=EDGE_CURVE('',#8860,#8858,#5323,.T.);
#10851=EDGE_CURVE('',#8861,#8861,#7816,.T.);
#10852=EDGE_CURVE('',#8861,#8860,#5324,.T.);
#10853=EDGE_CURVE('',#8862,#8862,#7817,.T.);
#10854=EDGE_CURVE('',#8862,#8861,#5325,.T.);
#10855=EDGE_CURVE('',#8853,#8859,#5326,.T.);
#10856=EDGE_CURVE('',#8863,#8864,#7818,.T.);
#10857=EDGE_CURVE('',#8865,#8866,#7819,.T.);
#10858=EDGE_CURVE('',#8867,#8868,#7820,.T.);
#10859=EDGE_CURVE('',#8869,#8870,#7821,.T.);
#10860=EDGE_CURVE('',#8871,#8872,#7822,.T.);
#10861=EDGE_CURVE('',#8873,#8874,#7823,.T.);
#10862=EDGE_CURVE('',#8875,#8876,#7824,.T.);
#10863=EDGE_CURVE('',#8877,#8878,#7825,.T.);
#10864=EDGE_CURVE('',#8879,#8880,#567,.T.);
#10865=EDGE_CURVE('',#8881,#8879,#7826,.T.);
#10866=EDGE_CURVE('',#8882,#8881,#568,.T.);
#10867=EDGE_CURVE('',#8880,#8882,#7827,.T.);
#10868=EDGE_CURVE('',#8883,#8881,#7828,.T.);
#10869=EDGE_CURVE('',#8883,#8884,#569,.T.);
#10870=EDGE_CURVE('',#8885,#8884,#7829,.T.);
#10871=EDGE_CURVE('',#8885,#8886,#570,.T.);
#10872=EDGE_CURVE('',#8887,#8886,#7830,.T.);
#10873=EDGE_CURVE('',#8887,#8888,#571,.T.);
#10874=EDGE_CURVE('',#8888,#8889,#5327,.T.);
#10875=EDGE_CURVE('',#8889,#8889,#7831,.T.);
#10876=EDGE_CURVE('',#8888,#8890,#572,.T.);
#10877=EDGE_CURVE('',#8891,#8890,#7832,.T.);
#10878=EDGE_CURVE('',#8891,#8892,#573,.T.);
#10879=EDGE_CURVE('',#8893,#8892,#7833,.T.);
#10880=EDGE_CURVE('',#8893,#8894,#574,.T.);
#10881=EDGE_CURVE('',#8895,#8894,#7834,.T.);
#10882=EDGE_CURVE('',#8895,#8896,#575,.T.);
#10883=EDGE_CURVE('',#8897,#8896,#7835,.T.);
#10884=EDGE_CURVE('',#8897,#8898,#576,.T.);
#10885=EDGE_CURVE('',#8882,#8898,#7836,.T.);
#10886=EDGE_CURVE('',#8879,#8899,#7837,.T.);
#10887=EDGE_CURVE('',#8899,#8883,#7838,.T.);
#10888=EDGE_CURVE('',#8900,#8899,#577,.T.);
#10889=EDGE_CURVE('',#8884,#8900,#7839,.T.);
#10890=EDGE_CURVE('',#8900,#8901,#7840,.T.);
#10891=EDGE_CURVE('',#8901,#8885,#7841,.T.);
#10892=EDGE_CURVE('',#8902,#8901,#578,.T.);
#10893=EDGE_CURVE('',#8886,#8902,#7842,.T.);
#10894=EDGE_CURVE('',#8902,#8903,#7843,.T.);
#10895=EDGE_CURVE('',#8903,#8887,#7844,.T.);
#10896=EDGE_CURVE('',#8904,#8905,#579,.T.);
#10897=EDGE_CURVE('',#8890,#8904,#7845,.T.);
#10898=EDGE_CURVE('',#8905,#8903,#580,.T.);
#10899=EDGE_CURVE('',#8904,#8906,#7846,.T.);
#10900=EDGE_CURVE('',#8906,#8891,#7847,.T.);
#10901=EDGE_CURVE('',#8907,#8906,#581,.T.);
#10902=EDGE_CURVE('',#8892,#8907,#7848,.T.);
#10903=EDGE_CURVE('',#8907,#8908,#7849,.T.);
#10904=EDGE_CURVE('',#8908,#8893,#7850,.T.);
#10905=EDGE_CURVE('',#8909,#8908,#582,.T.);
#10906=EDGE_CURVE('',#8894,#8909,#7851,.T.);
#10907=EDGE_CURVE('',#8909,#8910,#7852,.T.);
#10908=EDGE_CURVE('',#8910,#8895,#7853,.T.);
#10909=EDGE_CURVE('',#8911,#8910,#583,.T.);
#10910=EDGE_CURVE('',#8896,#8911,#7854,.T.);
#10911=EDGE_CURVE('',#8912,#8912,#7855,.T.);
#10912=EDGE_CURVE('',#8912,#8905,#5328,.T.);
#10913=EDGE_CURVE('',#8913,#8880,#7856,.T.);
#10914=EDGE_CURVE('',#8913,#8914,#584,.T.);
#10915=EDGE_CURVE('',#8911,#8914,#7857,.T.);
#10916=EDGE_CURVE('',#8898,#8913,#7858,.T.);
#10917=EDGE_CURVE('',#8914,#8897,#7859,.T.);
#10918=EDGE_CURVE('',#8915,#8915,#7860,.T.);
#10919=EDGE_CURVE('',#8916,#8916,#7861,.T.);
#10920=EDGE_CURVE('',#8917,#8917,#7862,.T.);
#10921=EDGE_CURVE('',#8917,#8915,#5329,.T.);
#10922=EDGE_CURVE('',#8918,#8918,#7863,.T.);
#10923=EDGE_CURVE('',#8918,#8916,#5330,.T.);
#10924=EDGE_CURVE('',#8919,#8919,#7864,.T.);
#10925=EDGE_CURVE('',#8920,#8920,#7865,.T.);
#10926=EDGE_CURVE('',#8921,#8921,#7866,.T.);
#10927=EDGE_CURVE('',#8921,#8919,#5331,.T.);
#10928=EDGE_CURVE('',#8922,#8922,#7867,.T.);
#10929=EDGE_CURVE('',#8922,#8920,#5332,.T.);
#10930=EDGE_CURVE('',#8923,#8923,#7868,.T.);
#10931=EDGE_CURVE('',#8924,#8924,#7869,.T.);
#10932=EDGE_CURVE('',#8925,#8925,#7870,.T.);
#10933=EDGE_CURVE('',#8924,#8923,#5333,.T.);
#10934=EDGE_CURVE('',#8926,#8926,#7871,.T.);
#10935=EDGE_CURVE('',#8927,#8927,#7872,.T.);
#10936=EDGE_CURVE('',#8927,#8926,#5334,.T.);
#10937=EDGE_CURVE('',#8928,#8928,#7873,.T.);
#10938=EDGE_CURVE('',#8928,#8927,#5335,.T.);
#10939=EDGE_CURVE('',#8929,#8929,#7874,.T.);
#10940=EDGE_CURVE('',#8929,#8928,#5336,.T.);
#10941=EDGE_CURVE('',#8930,#8930,#7875,.T.);
#10942=EDGE_CURVE('',#8931,#8931,#7876,.F.);
#10943=EDGE_CURVE('',#8931,#8930,#5337,.T.);
#10944=EDGE_CURVE('',#8925,#8931,#5338,.T.);
#10945=EDGE_CURVE('',#8932,#8933,#5339,.T.);
#10946=EDGE_CURVE('',#8933,#8934,#5340,.T.);
#10947=EDGE_CURVE('',#8934,#8935,#5341,.T.);
#10948=EDGE_CURVE('',#8932,#8935,#5342,.T.);
#10949=EDGE_CURVE('',#8933,#8936,#5343,.T.);
#10950=EDGE_CURVE('',#8936,#8937,#5344,.T.);
#10951=EDGE_CURVE('',#8937,#8934,#5345,.T.);
#10952=EDGE_CURVE('',#8936,#8938,#5346,.T.);
#10953=EDGE_CURVE('',#8938,#8939,#5347,.T.);
#10954=EDGE_CURVE('',#8939,#8937,#5348,.T.);
#10955=EDGE_CURVE('',#8938,#8940,#5349,.T.);
#10956=EDGE_CURVE('',#8940,#8941,#5350,.T.);
#10957=EDGE_CURVE('',#8941,#8939,#5351,.T.);
#10958=EDGE_CURVE('',#8940,#8942,#5352,.T.);
#10959=EDGE_CURVE('',#8942,#8943,#5353,.T.);
#10960=EDGE_CURVE('',#8943,#8941,#5354,.T.);
#10961=EDGE_CURVE('',#8942,#8932,#5355,.T.);
#10962=EDGE_CURVE('',#8935,#8943,#5356,.T.);
#10963=EDGE_CURVE('',#8944,#8945,#5357,.T.);
#10964=EDGE_CURVE('',#8945,#8946,#5358,.T.);
#10965=EDGE_CURVE('',#8946,#8947,#5359,.T.);
#10966=EDGE_CURVE('',#8944,#8947,#5360,.T.);
#10967=EDGE_CURVE('',#8945,#8948,#5361,.T.);
#10968=EDGE_CURVE('',#8948,#8949,#5362,.T.);
#10969=EDGE_CURVE('',#8949,#8946,#5363,.T.);
#10970=EDGE_CURVE('',#8948,#8950,#5364,.T.);
#10971=EDGE_CURVE('',#8950,#8951,#5365,.T.);
#10972=EDGE_CURVE('',#8951,#8949,#5366,.T.);
#10973=EDGE_CURVE('',#8950,#8952,#5367,.T.);
#10974=EDGE_CURVE('',#8952,#8953,#5368,.T.);
#10975=EDGE_CURVE('',#8953,#8951,#5369,.T.);
#10976=EDGE_CURVE('',#8952,#8954,#5370,.T.);
#10977=EDGE_CURVE('',#8954,#8955,#5371,.T.);
#10978=EDGE_CURVE('',#8955,#8953,#5372,.T.);
#10979=EDGE_CURVE('',#8954,#8944,#5373,.T.);
#10980=EDGE_CURVE('',#8947,#8955,#5374,.T.);
#10981=EDGE_CURVE('',#8956,#8956,#7877,.T.);
#10982=EDGE_CURVE('',#8957,#8957,#7878,.T.);
#10983=EDGE_CURVE('',#8958,#8958,#7879,.T.);
#10984=EDGE_CURVE('',#8958,#8957,#5375,.T.);
#10985=EDGE_CURVE('',#8959,#8959,#7880,.T.);
#10986=EDGE_CURVE('',#8959,#8958,#5376,.T.);
#10987=EDGE_CURVE('',#8960,#8960,#7881,.T.);
#10988=EDGE_CURVE('',#8960,#8959,#5377,.T.);
#10989=EDGE_CURVE('',#8961,#8961,#7882,.T.);
#10990=EDGE_CURVE('',#8962,#8962,#7883,.F.);
#10991=EDGE_CURVE('',#8962,#8961,#5378,.T.);
#10992=EDGE_CURVE('',#8956,#8962,#5379,.T.);
#10993=EDGE_CURVE('',#8963,#8964,#5380,.T.);
#10994=EDGE_CURVE('',#8963,#8965,#5381,.T.);
#10995=EDGE_CURVE('',#8966,#8965,#5382,.T.);
#10996=EDGE_CURVE('',#8964,#8966,#5383,.T.);
#10997=EDGE_CURVE('',#8967,#8963,#5384,.T.);
#10998=EDGE_CURVE('',#8967,#8968,#5385,.T.);
#10999=EDGE_CURVE('',#8965,#8968,#5386,.T.);
#11000=EDGE_CURVE('',#8969,#8967,#5387,.T.);
#11001=EDGE_CURVE('',#8969,#8970,#5388,.T.);
#11002=EDGE_CURVE('',#8968,#8970,#5389,.T.);
#11003=EDGE_CURVE('',#8971,#8969,#5390,.T.);
#11004=EDGE_CURVE('',#8971,#8972,#5391,.T.);
#11005=EDGE_CURVE('',#8970,#8972,#5392,.T.);
#11006=EDGE_CURVE('',#8973,#8971,#5393,.T.);
#11007=EDGE_CURVE('',#8973,#8974,#5394,.T.);
#11008=EDGE_CURVE('',#8972,#8974,#5395,.T.);
#11009=EDGE_CURVE('',#8975,#8973,#5396,.T.);
#11010=EDGE_CURVE('',#8975,#8976,#5397,.T.);
#11011=EDGE_CURVE('',#8974,#8976,#5398,.T.);
#11012=EDGE_CURVE('',#8977,#8975,#5399,.T.);
#11013=EDGE_CURVE('',#8977,#8978,#5400,.T.);
#11014=EDGE_CURVE('',#8976,#8978,#5401,.T.);
#11015=EDGE_CURVE('',#8979,#8977,#5402,.T.);
#11016=EDGE_CURVE('',#8979,#8980,#5403,.T.);
#11017=EDGE_CURVE('',#8978,#8980,#5404,.T.);
#11018=EDGE_CURVE('',#8981,#8979,#5405,.T.);
#11019=EDGE_CURVE('',#8982,#8981,#5406,.T.);
#11020=EDGE_CURVE('',#8980,#8982,#5407,.T.);
#11021=EDGE_CURVE('',#8983,#8984,#5408,.T.);
#11022=EDGE_CURVE('',#8983,#8985,#5409,.T.);
#11023=EDGE_CURVE('',#8986,#8985,#5410,.T.);
#11024=EDGE_CURVE('',#8984,#8986,#5411,.T.);
#11025=EDGE_CURVE('',#8987,#8983,#5412,.T.);
#11026=EDGE_CURVE('',#8987,#8988,#5413,.T.);
#11027=EDGE_CURVE('',#8985,#8988,#5414,.T.);
#11028=EDGE_CURVE('',#8989,#8987,#5415,.T.);
#11029=EDGE_CURVE('',#8989,#8990,#5416,.T.);
#11030=EDGE_CURVE('',#8988,#8990,#5417,.T.);
#11031=EDGE_CURVE('',#8991,#8989,#5418,.T.);
#11032=EDGE_CURVE('',#8991,#8992,#5419,.T.);
#11033=EDGE_CURVE('',#8990,#8992,#5420,.T.);
#11034=EDGE_CURVE('',#8993,#8991,#5421,.T.);
#11035=EDGE_CURVE('',#8993,#8994,#5422,.T.);
#11036=EDGE_CURVE('',#8992,#8994,#5423,.T.);
#11037=EDGE_CURVE('',#8995,#8993,#5424,.T.);
#11038=EDGE_CURVE('',#8995,#8996,#5425,.T.);
#11039=EDGE_CURVE('',#8994,#8996,#5426,.T.);
#11040=EDGE_CURVE('',#8997,#8995,#5427,.T.);
#11041=EDGE_CURVE('',#8997,#8998,#5428,.T.);
#11042=EDGE_CURVE('',#8996,#8998,#5429,.T.);
#11043=EDGE_CURVE('',#8999,#8997,#5430,.T.);
#11044=EDGE_CURVE('',#8999,#9000,#5431,.T.);
#11045=EDGE_CURVE('',#8998,#9000,#5432,.T.);
#11046=EDGE_CURVE('',#9001,#8999,#5433,.T.);
#11047=EDGE_CURVE('',#9002,#9001,#5434,.T.);
#11048=EDGE_CURVE('',#9000,#9002,#5435,.T.);
#11049=EDGE_CURVE('',#9003,#9004,#5436,.T.);
#11050=EDGE_CURVE('',#9003,#9005,#5437,.T.);
#11051=EDGE_CURVE('',#9006,#9005,#5438,.T.);
#11052=EDGE_CURVE('',#9004,#9006,#5439,.T.);
#11053=EDGE_CURVE('',#9007,#9003,#5440,.T.);
#11054=EDGE_CURVE('',#9007,#9008,#5441,.T.);
#11055=EDGE_CURVE('',#9005,#9008,#5442,.T.);
#11056=EDGE_CURVE('',#9009,#9007,#5443,.T.);
#11057=EDGE_CURVE('',#9009,#9010,#5444,.T.);
#11058=EDGE_CURVE('',#9008,#9010,#5445,.T.);
#11059=EDGE_CURVE('',#9011,#9009,#5446,.T.);
#11060=EDGE_CURVE('',#9011,#9012,#5447,.T.);
#11061=EDGE_CURVE('',#9010,#9012,#5448,.T.);
#11062=EDGE_CURVE('',#9013,#9011,#5449,.T.);
#11063=EDGE_CURVE('',#9013,#9014,#5450,.T.);
#11064=EDGE_CURVE('',#9012,#9014,#5451,.T.);
#11065=EDGE_CURVE('',#9015,#9013,#5452,.T.);
#11066=EDGE_CURVE('',#9015,#9016,#5453,.T.);
#11067=EDGE_CURVE('',#9014,#9016,#5454,.T.);
#11068=EDGE_CURVE('',#9017,#9015,#5455,.T.);
#11069=EDGE_CURVE('',#9017,#9018,#5456,.T.);
#11070=EDGE_CURVE('',#9016,#9018,#5457,.T.);
#11071=EDGE_CURVE('',#9019,#9017,#5458,.T.);
#11072=EDGE_CURVE('',#9019,#9020,#5459,.T.);
#11073=EDGE_CURVE('',#9018,#9020,#5460,.T.);
#11074=EDGE_CURVE('',#9021,#9019,#5461,.T.);
#11075=EDGE_CURVE('',#9022,#9021,#5462,.T.);
#11076=EDGE_CURVE('',#9020,#9022,#5463,.T.);
#11077=EDGE_CURVE('',#9023,#9024,#5464,.T.);
#11078=EDGE_CURVE('',#9023,#9025,#5465,.T.);
#11079=EDGE_CURVE('',#9026,#9025,#5466,.T.);
#11080=EDGE_CURVE('',#9024,#9026,#5467,.T.);
#11081=EDGE_CURVE('',#9027,#9023,#5468,.T.);
#11082=EDGE_CURVE('',#9027,#9028,#5469,.T.);
#11083=EDGE_CURVE('',#9025,#9028,#5470,.T.);
#11084=EDGE_CURVE('',#9029,#9027,#5471,.T.);
#11085=EDGE_CURVE('',#9029,#9030,#5472,.T.);
#11086=EDGE_CURVE('',#9028,#9030,#5473,.T.);
#11087=EDGE_CURVE('',#9031,#9029,#5474,.T.);
#11088=EDGE_CURVE('',#9031,#9032,#5475,.T.);
#11089=EDGE_CURVE('',#9030,#9032,#5476,.T.);
#11090=EDGE_CURVE('',#9033,#9031,#5477,.T.);
#11091=EDGE_CURVE('',#9033,#9034,#5478,.T.);
#11092=EDGE_CURVE('',#9032,#9034,#5479,.T.);
#11093=EDGE_CURVE('',#9035,#9033,#5480,.T.);
#11094=EDGE_CURVE('',#9035,#9036,#5481,.T.);
#11095=EDGE_CURVE('',#9034,#9036,#5482,.T.);
#11096=EDGE_CURVE('',#9037,#9035,#5483,.T.);
#11097=EDGE_CURVE('',#9037,#9038,#5484,.T.);
#11098=EDGE_CURVE('',#9036,#9038,#5485,.T.);
#11099=EDGE_CURVE('',#9039,#9037,#5486,.T.);
#11100=EDGE_CURVE('',#9039,#9040,#5487,.T.);
#11101=EDGE_CURVE('',#9038,#9040,#5488,.T.);
#11102=EDGE_CURVE('',#9041,#9039,#5489,.T.);
#11103=EDGE_CURVE('',#9042,#9041,#5490,.T.);
#11104=EDGE_CURVE('',#9040,#9042,#5491,.T.);
#11105=EDGE_CURVE('',#9043,#9043,#7884,.T.);
#11106=EDGE_CURVE('',#9043,#9044,#5492,.T.);
#11107=EDGE_CURVE('',#9044,#9044,#7885,.T.);
#11108=EDGE_CURVE('',#8981,#9045,#5493,.T.);
#11109=EDGE_CURVE('',#9045,#9046,#5494,.T.);
#11110=EDGE_CURVE('',#8982,#9046,#5495,.T.);
#11111=EDGE_CURVE('',#9047,#8966,#5496,.T.);
#11112=EDGE_CURVE('',#9048,#9047,#5497,.T.);
#11113=EDGE_CURVE('',#9048,#8964,#5498,.T.);
#11114=EDGE_CURVE('',#9001,#9048,#5499,.T.);
#11115=EDGE_CURVE('',#9002,#9047,#5500,.T.);
#11116=EDGE_CURVE('',#9049,#8986,#5501,.T.);
#11117=EDGE_CURVE('',#9050,#9049,#5502,.T.);
#11118=EDGE_CURVE('',#9050,#8984,#5503,.T.);
#11119=EDGE_CURVE('',#9021,#9050,#5504,.T.);
#11120=EDGE_CURVE('',#9022,#9049,#5505,.T.);
#11121=EDGE_CURVE('',#9051,#9006,#5506,.T.);
#11122=EDGE_CURVE('',#9052,#9051,#5507,.T.);
#11123=EDGE_CURVE('',#9052,#9004,#5508,.T.);
#11124=EDGE_CURVE('',#9041,#9052,#5509,.T.);
#11125=EDGE_CURVE('',#9042,#9051,#5510,.T.);
#11126=EDGE_CURVE('',#9046,#9026,#5511,.T.);
#11127=EDGE_CURVE('',#9045,#9024,#5512,.T.);
#11128=EDGE_CURVE('',#9053,#9053,#7886,.T.);
#11129=EDGE_CURVE('',#9054,#9054,#7887,.T.);
#11130=EDGE_CURVE('',#9054,#9053,#5513,.T.);
#11131=EDGE_CURVE('',#9055,#9055,#7888,.T.);
#11132=EDGE_CURVE('',#9055,#9054,#5514,.T.);
#11133=EDGE_CURVE('',#9056,#9056,#7889,.T.);
#11134=EDGE_CURVE('',#9056,#9055,#5515,.T.);
#11135=EDGE_CURVE('',#9057,#9057,#7890,.T.);
#11136=EDGE_CURVE('',#9058,#9058,#7891,.F.);
#11137=EDGE_CURVE('',#9058,#9057,#5516,.T.);
#11138=EDGE_CURVE('',#9059,#9059,#7892,.F.);
#11139=EDGE_CURVE('',#9059,#9058,#5517,.T.);
#11140=EDGE_CURVE('',#9060,#9060,#7893,.T.);
#11141=EDGE_CURVE('',#9060,#9059,#5518,.T.);
#11142=EDGE_CURVE('',#9061,#9062,#5519,.T.);
#11143=EDGE_CURVE('',#9062,#9063,#5520,.T.);
#11144=EDGE_CURVE('',#9063,#9064,#5521,.T.);
#11145=EDGE_CURVE('',#9061,#9064,#5522,.T.);
#11146=EDGE_CURVE('',#9062,#9065,#5523,.T.);
#11147=EDGE_CURVE('',#9065,#9066,#5524,.T.);
#11148=EDGE_CURVE('',#9066,#9063,#5525,.T.);
#11149=EDGE_CURVE('',#9065,#9067,#5526,.T.);
#11150=EDGE_CURVE('',#9067,#9068,#5527,.T.);
#11151=EDGE_CURVE('',#9068,#9066,#5528,.T.);
#11152=EDGE_CURVE('',#9067,#9069,#5529,.T.);
#11153=EDGE_CURVE('',#9069,#9070,#5530,.T.);
#11154=EDGE_CURVE('',#9070,#9068,#5531,.T.);
#11155=EDGE_CURVE('',#9069,#9071,#5532,.T.);
#11156=EDGE_CURVE('',#9071,#9072,#5533,.T.);
#11157=EDGE_CURVE('',#9072,#9070,#5534,.T.);
#11158=EDGE_CURVE('',#9071,#9061,#5535,.T.);
#11159=EDGE_CURVE('',#9064,#9072,#5536,.T.);
#11160=EDGE_CURVE('',#9073,#9074,#5537,.T.);
#11161=EDGE_CURVE('',#9075,#9073,#5538,.T.);
#11162=EDGE_CURVE('',#9076,#9075,#5539,.T.);
#11163=EDGE_CURVE('',#9074,#9076,#5540,.T.);
#11164=EDGE_CURVE('',#9075,#9077,#5541,.T.);
#11165=EDGE_CURVE('',#9078,#9077,#5542,.T.);
#11166=EDGE_CURVE('',#9076,#9078,#5543,.T.);
#11167=EDGE_CURVE('',#9077,#9079,#5544,.T.);
#11168=EDGE_CURVE('',#9079,#9080,#5545,.T.);
#11169=EDGE_CURVE('',#9080,#9078,#5546,.T.);
#11170=EDGE_CURVE('',#9081,#9081,#7894,.T.);
#11171=EDGE_CURVE('',#9082,#9073,#5547,.T.);
#11172=EDGE_CURVE('',#9083,#9082,#5548,.T.);
#11173=EDGE_CURVE('',#9083,#9084,#5549,.T.);
#11174=EDGE_CURVE('',#9085,#9084,#5550,.T.);
#11175=EDGE_CURVE('',#9085,#9086,#5551,.T.);
#11176=EDGE_CURVE('',#9086,#9087,#5552,.T.);
#11177=EDGE_CURVE('',#9087,#9079,#5553,.T.);
#11178=EDGE_CURVE('',#9087,#9088,#5554,.T.);
#11179=EDGE_CURVE('',#9088,#9080,#5555,.T.);
#11180=EDGE_CURVE('',#9089,#9086,#5556,.T.);
#11181=EDGE_CURVE('',#9088,#9089,#5557,.T.);
#11182=EDGE_CURVE('',#9090,#9089,#5558,.T.);
#11183=EDGE_CURVE('',#9091,#9090,#5559,.T.);
#11184=EDGE_CURVE('',#9091,#9092,#5560,.T.);
#11185=EDGE_CURVE('',#9093,#9092,#5561,.T.);
#11186=EDGE_CURVE('',#9093,#9074,#5562,.T.);
#11187=EDGE_CURVE('',#9090,#9085,#5563,.T.);
#11188=EDGE_CURVE('',#9084,#9094,#5564,.T.);
#11189=EDGE_CURVE('',#9094,#9095,#15,.T.);
#11190=EDGE_CURVE('',#9095,#9091,#5565,.T.);
#11191=EDGE_CURVE('',#9096,#9094,#7895,.F.);
#11192=EDGE_CURVE('',#9096,#9081,#5566,.T.);
#11193=EDGE_CURVE('',#9097,#9096,#7896,.F.);
#11194=EDGE_CURVE('',#9098,#9097,#16,.T.);
#11195=EDGE_CURVE('',#9095,#9098,#7897,.F.);
#11196=EDGE_CURVE('',#9097,#9083,#5567,.T.);
#11197=EDGE_CURVE('',#9092,#9098,#5568,.T.);
#11198=EDGE_CURVE('',#9082,#9093,#5569,.T.);
#11199=EDGE_CURVE('',#9099,#9099,#7898,.T.);
#11200=EDGE_CURVE('',#9100,#9101,#5570,.T.);
#11201=EDGE_CURVE('',#9102,#9100,#5571,.T.);
#11202=EDGE_CURVE('',#9103,#9102,#5572,.T.);
#11203=EDGE_CURVE('',#9104,#9103,#5573,.T.);
#11204=EDGE_CURVE('',#9105,#9104,#5574,.T.);
#11205=EDGE_CURVE('',#9101,#9105,#5575,.T.);
#11206=EDGE_CURVE('',#9106,#9106,#7899,.T.);
#11207=EDGE_CURVE('',#9107,#9107,#7900,.T.);
#11208=EDGE_CURVE('',#9107,#9106,#5576,.T.);
#11209=EDGE_CURVE('',#9108,#9108,#7901,.T.);
#11210=EDGE_CURVE('',#9108,#9107,#5577,.T.);
#11211=EDGE_CURVE('',#9109,#9109,#7902,.T.);
#11212=EDGE_CURVE('',#9109,#9108,#5578,.T.);
#11213=EDGE_CURVE('',#9110,#9110,#7903,.T.);
#11214=EDGE_CURVE('',#9111,#9111,#7904,.F.);
#11215=EDGE_CURVE('',#9111,#9110,#5579,.T.);
#11216=EDGE_CURVE('',#9099,#9111,#5580,.T.);
#11217=EDGE_CURVE('',#9112,#9113,#5581,.T.);
#11218=EDGE_CURVE('',#9113,#9100,#5582,.T.);
#11219=EDGE_CURVE('',#9112,#9101,#5583,.T.);
#11220=EDGE_CURVE('',#9113,#9114,#5584,.T.);
#11221=EDGE_CURVE('',#9114,#9102,#5585,.T.);
#11222=EDGE_CURVE('',#9114,#9115,#5586,.T.);
#11223=EDGE_CURVE('',#9115,#9103,#5587,.T.);
#11224=EDGE_CURVE('',#9115,#9116,#5588,.T.);
#11225=EDGE_CURVE('',#9116,#9104,#5589,.T.);
#11226=EDGE_CURVE('',#9116,#9117,#5590,.T.);
#11227=EDGE_CURVE('',#9117,#9105,#5591,.T.);
#11228=EDGE_CURVE('',#9117,#9112,#5592,.T.);
#11229=EDGE_CURVE('',#9118,#9118,#7905,.T.);
#11230=EDGE_CURVE('',#9118,#9119,#5593,.T.);
#11231=EDGE_CURVE('',#9119,#9119,#7906,.T.);
#11232=EDGE_CURVE('',#9120,#9120,#7907,.T.);
#11233=EDGE_CURVE('',#9120,#9121,#5594,.T.);
#11234=EDGE_CURVE('',#9121,#9121,#7908,.T.);
#11235=EDGE_CURVE('',#9122,#9122,#7909,.T.);
#11236=EDGE_CURVE('',#9122,#9123,#5595,.T.);
#11237=EDGE_CURVE('',#9123,#9123,#7910,.T.);
#11238=EDGE_CURVE('',#9124,#9124,#7911,.T.);
#11239=EDGE_CURVE('',#9124,#9125,#5596,.T.);
#11240=EDGE_CURVE('',#9125,#9125,#7912,.T.);
#11241=EDGE_CURVE('',#9126,#9126,#7913,.T.);
#11242=EDGE_CURVE('',#9126,#9127,#5597,.T.);
#11243=EDGE_CURVE('',#9127,#9127,#7914,.T.);
#11244=EDGE_CURVE('',#9128,#9128,#7915,.T.);
#11245=EDGE_CURVE('',#9128,#9129,#5598,.T.);
#11246=EDGE_CURVE('',#9129,#9129,#7916,.T.);
#11247=EDGE_CURVE('',#9130,#9130,#7917,.T.);
#11248=EDGE_CURVE('',#9130,#9131,#5599,.T.);
#11249=EDGE_CURVE('',#9131,#9131,#7918,.T.);
#11250=EDGE_CURVE('',#9132,#9132,#7919,.T.);
#11251=EDGE_CURVE('',#9132,#9133,#5600,.T.);
#11252=EDGE_CURVE('',#9133,#9133,#7920,.T.);
#11253=EDGE_CURVE('',#9134,#9134,#7921,.T.);
#11254=EDGE_CURVE('',#9134,#9135,#5601,.T.);
#11255=EDGE_CURVE('',#9135,#9135,#7922,.T.);
#11256=EDGE_CURVE('',#9136,#9136,#7923,.T.);
#11257=EDGE_CURVE('',#9136,#9137,#5602,.T.);
#11258=EDGE_CURVE('',#9137,#9137,#7924,.T.);
#11259=EDGE_CURVE('',#9138,#9138,#7925,.T.);
#11260=EDGE_CURVE('',#9138,#9139,#5603,.T.);
#11261=EDGE_CURVE('',#9139,#9139,#7926,.T.);
#11262=EDGE_CURVE('',#9140,#9140,#7927,.T.);
#11263=EDGE_CURVE('',#9140,#9141,#5604,.T.);
#11264=EDGE_CURVE('',#9141,#9141,#7928,.T.);
#11265=EDGE_CURVE('',#9142,#9142,#7929,.T.);
#11266=EDGE_CURVE('',#9142,#9143,#5605,.T.);
#11267=EDGE_CURVE('',#9143,#9143,#7930,.T.);
#11268=EDGE_CURVE('',#9144,#9144,#7931,.T.);
#11269=EDGE_CURVE('',#9144,#9145,#5606,.T.);
#11270=EDGE_CURVE('',#9145,#9145,#7932,.T.);
#11271=EDGE_CURVE('',#9146,#9146,#7933,.T.);
#11272=EDGE_CURVE('',#9146,#9147,#5607,.T.);
#11273=EDGE_CURVE('',#9147,#9147,#7934,.T.);
#11274=EDGE_CURVE('',#9148,#9148,#7935,.T.);
#11275=EDGE_CURVE('',#9148,#9149,#5608,.T.);
#11276=EDGE_CURVE('',#9149,#9149,#7936,.T.);
#11277=EDGE_CURVE('',#9150,#9150,#7937,.T.);
#11278=EDGE_CURVE('',#9150,#9151,#5609,.T.);
#11279=EDGE_CURVE('',#9151,#9151,#7938,.T.);
#11280=EDGE_CURVE('',#9152,#9152,#7939,.T.);
#11281=EDGE_CURVE('',#9152,#9153,#5610,.T.);
#11282=EDGE_CURVE('',#9153,#9153,#7940,.T.);
#11283=EDGE_CURVE('',#9154,#9155,#5611,.T.);
#11284=EDGE_CURVE('',#9155,#9156,#5612,.T.);
#11285=EDGE_CURVE('',#9157,#9156,#5613,.T.);
#11286=EDGE_CURVE('',#9154,#9157,#5614,.T.);
#11287=EDGE_CURVE('',#9158,#9154,#5615,.T.);
#11288=EDGE_CURVE('',#9159,#9157,#5616,.T.);
#11289=EDGE_CURVE('',#9158,#9159,#5617,.T.);
#11290=EDGE_CURVE('',#9160,#9158,#5618,.T.);
#11291=EDGE_CURVE('',#9161,#9159,#5619,.T.);
#11292=EDGE_CURVE('',#9160,#9161,#5620,.T.);
#11293=EDGE_CURVE('',#9155,#9160,#5621,.T.);
#11294=EDGE_CURVE('',#9156,#9161,#5622,.T.);
#11295=EDGE_CURVE('',#9162,#9163,#7941,.T.);
#11296=EDGE_CURVE('',#9162,#9163,#7942,.T.);
#11297=EDGE_CURVE('',#9164,#9162,#5623,.T.);
#11298=EDGE_CURVE('',#9165,#9164,#7943,.T.);
#11299=EDGE_CURVE('',#9165,#9166,#5624,.T.);
#11300=EDGE_CURVE('',#9166,#9166,#7944,.T.);
#11301=EDGE_CURVE('',#9167,#9165,#7945,.T.);
#11302=EDGE_CURVE('',#9163,#9167,#5625,.T.);
#11303=EDGE_CURVE('',#9168,#9169,#7946,.T.);
#11304=EDGE_CURVE('',#9168,#9169,#7947,.T.);
#11305=EDGE_CURVE('',#9170,#9168,#5626,.T.);
#11306=EDGE_CURVE('',#9171,#9170,#7948,.T.);
#11307=EDGE_CURVE('',#9171,#9172,#5627,.T.);
#11308=EDGE_CURVE('',#9172,#9172,#7949,.T.);
#11309=EDGE_CURVE('',#9173,#9171,#7950,.T.);
#11310=EDGE_CURVE('',#9169,#9173,#5628,.T.);
#11311=EDGE_CURVE('',#9174,#9175,#7951,.T.);
#11312=EDGE_CURVE('',#9174,#9176,#7952,.T.);
#11313=EDGE_CURVE('',#9176,#9175,#7953,.T.);
#11314=EDGE_CURVE('',#9177,#9174,#5629,.T.);
#11315=EDGE_CURVE('',#9178,#9177,#7954,.T.);
#11316=EDGE_CURVE('',#9175,#9178,#5630,.T.);
#11317=EDGE_CURVE('',#9176,#9179,#5631,.T.);
#11318=EDGE_CURVE('',#9179,#9179,#7955,.T.);
#11319=EDGE_CURVE('',#9180,#9181,#7956,.T.);
#11320=EDGE_CURVE('',#9180,#9182,#7957,.T.);
#11321=EDGE_CURVE('',#9182,#9181,#7958,.T.);
#11322=EDGE_CURVE('',#9183,#9180,#5632,.T.);
#11323=EDGE_CURVE('',#9184,#9183,#7959,.T.);
#11324=EDGE_CURVE('',#9181,#9184,#5633,.T.);
#11325=EDGE_CURVE('',#9182,#9185,#5634,.T.);
#11326=EDGE_CURVE('',#9185,#9185,#7960,.T.);
#11327=EDGE_CURVE('',#9167,#9186,#7961,.T.);
#11328=EDGE_CURVE('',#9186,#9187,#5635,.T.);
#11329=EDGE_CURVE('',#9187,#9187,#7962,.T.);
#11330=EDGE_CURVE('',#9186,#9170,#7963,.T.);
#11331=EDGE_CURVE('',#9173,#9177,#7964,.T.);
#11332=EDGE_CURVE('',#9178,#9183,#7965,.T.);
#11333=EDGE_CURVE('',#9184,#9164,#7966,.T.);
#11334=EDGE_CURVE('',#9188,#9188,#7967,.T.);
#11335=EDGE_CURVE('',#9188,#9189,#5636,.T.);
#11336=EDGE_CURVE('',#9189,#9189,#7968,.T.);
#11337=EDGE_CURVE('',#9190,#9190,#7969,.T.);
#11338=EDGE_CURVE('',#9191,#9191,#7970,.T.);
#11339=EDGE_CURVE('',#9192,#9192,#7971,.T.);
#11340=EDGE_CURVE('',#9192,#9191,#5637,.T.);
#11341=EDGE_CURVE('',#9190,#9193,#5638,.T.);
#11342=EDGE_CURVE('',#9193,#9193,#7972,.T.);
#11343=EDGE_CURVE('',#9194,#9195,#7973,.T.);
#11344=EDGE_CURVE('',#9194,#9195,#7974,.T.);
#11345=EDGE_CURVE('',#9196,#9194,#5639,.T.);
#11346=EDGE_CURVE('',#9197,#9196,#7975,.T.);
#11347=EDGE_CURVE('',#9197,#9198,#5640,.T.);
#11348=EDGE_CURVE('',#9198,#9198,#7976,.T.);
#11349=EDGE_CURVE('',#9199,#9197,#7977,.T.);
#11350=EDGE_CURVE('',#9195,#9199,#5641,.T.);
#11351=EDGE_CURVE('',#9200,#9201,#7978,.T.);
#11352=EDGE_CURVE('',#9200,#9201,#7979,.T.);
#11353=EDGE_CURVE('',#9202,#9200,#5642,.T.);
#11354=EDGE_CURVE('',#9203,#9202,#7980,.T.);
#11355=EDGE_CURVE('',#9203,#9204,#5643,.T.);
#11356=EDGE_CURVE('',#9204,#9204,#7981,.T.);
#11357=EDGE_CURVE('',#9205,#9203,#7982,.T.);
#11358=EDGE_CURVE('',#9201,#9205,#5644,.T.);
#11359=EDGE_CURVE('',#9206,#9207,#7983,.T.);
#11360=EDGE_CURVE('',#9206,#9208,#7984,.T.);
#11361=EDGE_CURVE('',#9208,#9207,#7985,.T.);
#11362=EDGE_CURVE('',#9209,#9206,#5645,.T.);
#11363=EDGE_CURVE('',#9210,#9209,#7986,.T.);
#11364=EDGE_CURVE('',#9207,#9210,#5646,.T.);
#11365=EDGE_CURVE('',#9208,#9211,#5647,.T.);
#11366=EDGE_CURVE('',#9211,#9211,#7987,.T.);
#11367=EDGE_CURVE('',#9212,#9213,#7988,.T.);
#11368=EDGE_CURVE('',#9212,#9214,#7989,.T.);
#11369=EDGE_CURVE('',#9214,#9213,#7990,.T.);
#11370=EDGE_CURVE('',#9215,#9212,#5648,.T.);
#11371=EDGE_CURVE('',#9216,#9215,#7991,.T.);
#11372=EDGE_CURVE('',#9213,#9216,#5649,.T.);
#11373=EDGE_CURVE('',#9214,#9217,#5650,.T.);
#11374=EDGE_CURVE('',#9217,#9217,#7992,.T.);
#11375=EDGE_CURVE('',#9199,#9218,#7993,.T.);
#11376=EDGE_CURVE('',#9218,#9219,#5651,.T.);
#11377=EDGE_CURVE('',#9219,#9219,#7994,.T.);
#11378=EDGE_CURVE('',#9218,#9202,#7995,.T.);
#11379=EDGE_CURVE('',#9205,#9209,#7996,.T.);
#11380=EDGE_CURVE('',#9210,#9215,#7997,.T.);
#11381=EDGE_CURVE('',#9216,#9196,#7998,.T.);
#11382=EDGE_CURVE('',#9220,#9220,#7999,.T.);
#11383=EDGE_CURVE('',#9220,#9221,#5652,.T.);
#11384=EDGE_CURVE('',#9221,#9221,#8000,.T.);
#11385=EDGE_CURVE('',#9222,#9222,#8001,.T.);
#11386=EDGE_CURVE('',#9223,#9223,#8002,.T.);
#11387=EDGE_CURVE('',#9224,#9224,#8003,.T.);
#11388=EDGE_CURVE('',#9224,#9223,#5653,.T.);
#11389=EDGE_CURVE('',#9222,#9225,#5654,.T.);
#11390=EDGE_CURVE('',#9225,#9225,#8004,.T.);
#11391=EDGE_CURVE('',#9226,#9226,#8005,.T.);
#11392=EDGE_CURVE('',#9226,#9227,#5655,.T.);
#11393=EDGE_CURVE('',#9227,#9227,#8006,.T.);
#11394=EDGE_CURVE('',#9228,#9228,#8007,.T.);
#11395=EDGE_CURVE('',#9228,#9229,#5656,.T.);
#11396=EDGE_CURVE('',#9229,#9229,#8008,.T.);
#11397=EDGE_CURVE('',#9230,#9230,#8009,.T.);
#11398=EDGE_CURVE('',#9230,#9231,#5657,.T.);
#11399=EDGE_CURVE('',#9231,#9231,#8010,.T.);
#11400=EDGE_CURVE('',#9232,#9232,#8011,.T.);
#11401=EDGE_CURVE('',#9232,#9233,#5658,.T.);
#11402=EDGE_CURVE('',#9233,#9233,#8012,.T.);
#11403=EDGE_CURVE('',#9234,#9234,#8013,.T.);
#11404=EDGE_CURVE('',#9234,#9235,#5659,.T.);
#11405=EDGE_CURVE('',#9235,#9235,#8014,.T.);
#11406=EDGE_CURVE('',#9236,#9236,#8015,.T.);
#11407=EDGE_CURVE('',#9236,#9237,#5660,.T.);
#11408=EDGE_CURVE('',#9237,#9237,#8016,.T.);
#11409=EDGE_CURVE('',#9238,#9238,#8017,.T.);
#11410=EDGE_CURVE('',#9238,#9239,#5661,.T.);
#11411=EDGE_CURVE('',#9239,#9239,#8018,.T.);
#11412=EDGE_CURVE('',#9240,#9240,#8019,.T.);
#11413=EDGE_CURVE('',#9240,#9241,#5662,.T.);
#11414=EDGE_CURVE('',#9241,#9241,#8020,.T.);
#11415=EDGE_CURVE('',#9242,#9242,#8021,.T.);
#11416=EDGE_CURVE('',#9242,#9243,#5663,.T.);
#11417=EDGE_CURVE('',#9243,#9243,#8022,.T.);
#11418=EDGE_CURVE('',#9244,#9244,#8023,.T.);
#11419=EDGE_CURVE('',#9244,#9245,#5664,.T.);
#11420=EDGE_CURVE('',#9245,#9245,#8024,.T.);
#11421=EDGE_CURVE('',#9246,#9247,#5665,.T.);
#11422=EDGE_CURVE('',#9248,#9247,#5666,.T.);
#11423=EDGE_CURVE('',#9249,#9248,#5667,.T.);
#11424=EDGE_CURVE('',#9246,#9249,#5668,.T.);
#11425=EDGE_CURVE('',#9250,#9246,#5669,.T.);
#11426=EDGE_CURVE('',#9251,#9249,#5670,.T.);
#11427=EDGE_CURVE('',#9250,#9251,#5671,.T.);
#11428=EDGE_CURVE('',#9251,#9248,#5672,.T.);
#11429=EDGE_CURVE('',#9252,#9253,#5673,.T.);
#11430=EDGE_CURVE('',#9252,#9254,#5674,.T.);
#11431=EDGE_CURVE('',#9254,#9255,#5675,.T.);
#11432=EDGE_CURVE('',#9253,#9255,#5676,.T.);
#11433=EDGE_CURVE('',#9256,#9252,#5677,.T.);
#11434=EDGE_CURVE('',#9257,#9256,#5678,.T.);
#11435=EDGE_CURVE('',#9254,#9257,#5679,.T.);
#11436=EDGE_CURVE('',#9258,#9256,#5680,.T.);
#11437=EDGE_CURVE('',#9259,#9258,#5681,.T.);
#11438=EDGE_CURVE('',#9257,#9259,#5682,.T.);
#11439=EDGE_CURVE('',#9255,#9259,#5683,.T.);
#11440=EDGE_CURVE('',#9247,#9260,#5684,.T.);
#11441=EDGE_CURVE('',#9260,#9261,#5685,.T.);
#11442=EDGE_CURVE('',#9262,#9261,#5686,.T.);
#11443=EDGE_CURVE('',#9263,#9262,#5687,.T.);
#11444=EDGE_CURVE('',#9263,#9250,#5688,.T.);
#11445=EDGE_CURVE('',#9260,#9264,#5689,.T.);
#11446=EDGE_CURVE('',#9264,#9265,#5690,.T.);
#11447=EDGE_CURVE('',#9261,#9265,#5691,.T.);
#11448=EDGE_CURVE('',#9266,#9263,#5692,.T.);
#11449=EDGE_CURVE('',#9267,#9262,#5693,.T.);
#11450=EDGE_CURVE('',#9266,#9267,#5694,.T.);
#11451=EDGE_CURVE('',#9265,#9253,#5695,.T.);
#11452=EDGE_CURVE('',#9264,#9266,#5696,.T.);
#11453=EDGE_CURVE('',#9258,#9267,#5697,.T.);
#11454=EDGE_CURVE('',#9268,#9269,#8025,.T.);
#11455=EDGE_CURVE('',#9270,#9268,#5698,.T.);
#11456=EDGE_CURVE('',#9271,#9270,#5699,.T.);
#11457=EDGE_CURVE('',#9269,#9271,#5700,.T.);
#11458=EDGE_CURVE('',#9269,#9272,#5701,.T.);
#11459=EDGE_CURVE('',#9273,#9271,#5702,.T.);
#11460=EDGE_CURVE('',#9273,#9272,#5703,.T.);
#11461=EDGE_CURVE('',#9272,#9274,#8026,.T.);
#11462=EDGE_CURVE('',#9275,#9273,#5704,.T.);
#11463=EDGE_CURVE('',#9274,#9275,#5705,.T.);
#11464=EDGE_CURVE('',#9274,#9268,#5706,.T.);
#11465=EDGE_CURVE('',#9275,#9270,#5707,.T.);
#11466=EDGE_CURVE('',#9276,#9276,#8027,.T.);
#11467=EDGE_CURVE('',#9277,#9277,#8028,.T.);
#11468=EDGE_CURVE('',#9278,#9278,#8029,.T.);
#11469=EDGE_CURVE('',#9278,#9276,#5708,.T.);
#11470=EDGE_CURVE('',#9279,#9279,#8030,.T.);
#11471=EDGE_CURVE('',#9280,#9280,#8031,.T.);
#11472=EDGE_CURVE('',#9280,#9279,#5709,.T.);
#11473=EDGE_CURVE('',#9281,#9281,#8032,.T.);
#11474=EDGE_CURVE('',#9282,#9282,#8033,.T.);
#11475=EDGE_CURVE('',#9282,#9281,#5710,.T.);
#11476=EDGE_CURVE('',#9283,#9283,#8034,.T.);
#11477=EDGE_CURVE('',#9284,#9284,#8035,.T.);
#11478=EDGE_CURVE('',#9284,#9283,#5711,.T.);
#11479=EDGE_CURVE('',#9285,#9285,#8036,.T.);
#11480=EDGE_CURVE('',#9286,#9286,#8037,.T.);
#11481=EDGE_CURVE('',#9286,#9285,#5712,.T.);
#11482=EDGE_CURVE('',#9287,#9287,#8038,.T.);
#11483=EDGE_CURVE('',#9287,#9277,#5713,.T.);
#11484=EDGE_CURVE('',#9288,#9289,#8039,.T.);
#11485=EDGE_CURVE('',#9290,#9288,#5714,.T.);
#11486=EDGE_CURVE('',#9291,#9290,#8040,.T.);
#11487=EDGE_CURVE('',#9289,#9291,#5715,.T.);
#11488=EDGE_CURVE('',#9289,#9292,#5716,.T.);
#11489=EDGE_CURVE('',#9293,#9291,#5717,.T.);
#11490=EDGE_CURVE('',#9293,#9292,#5718,.T.);
#11491=EDGE_CURVE('',#9292,#9294,#8041,.T.);
#11492=EDGE_CURVE('',#9295,#9293,#8042,.T.);
#11493=EDGE_CURVE('',#9294,#9295,#5719,.T.);
#11494=EDGE_CURVE('',#9294,#9288,#5720,.T.);
#11495=EDGE_CURVE('',#9290,#9295,#5721,.T.);
#11496=EDGE_CURVE('',#9296,#9296,#8043,.T.);
#11497=EDGE_CURVE('',#9297,#9297,#8044,.T.);
#11498=EDGE_CURVE('',#9298,#9298,#8045,.T.);
#11499=EDGE_CURVE('',#9298,#9296,#5722,.T.);
#11500=EDGE_CURVE('',#9299,#9299,#8046,.T.);
#11501=EDGE_CURVE('',#9299,#9297,#5723,.T.);
#11502=EDGE_CURVE('',#9300,#9301,#5724,.T.);
#11503=EDGE_CURVE('',#9301,#9302,#585,.T.);
#11504=EDGE_CURVE('',#9302,#9303,#8047,.F.);
#11505=EDGE_CURVE('',#9303,#9300,#586,.T.);
#11506=EDGE_CURVE('',#9304,#9305,#5725,.T.);
#11507=EDGE_CURVE('',#9305,#9301,#587,.T.);
#11508=EDGE_CURVE('',#9300,#9304,#588,.T.);
#11509=EDGE_CURVE('',#9306,#9307,#5726,.T.);
#11510=EDGE_CURVE('',#9307,#9305,#589,.T.);
#11511=EDGE_CURVE('',#9304,#9306,#590,.T.);
#11512=EDGE_CURVE('',#9308,#9309,#5727,.T.);
#11513=EDGE_CURVE('',#9309,#9307,#591,.T.);
#11514=EDGE_CURVE('',#9306,#9308,#592,.T.);
#11515=EDGE_CURVE('',#9310,#9311,#5728,.T.);
#11516=EDGE_CURVE('',#9311,#9309,#593,.T.);
#11517=EDGE_CURVE('',#9308,#9310,#594,.T.);
#11518=EDGE_CURVE('',#9312,#9313,#5729,.T.);
#11519=EDGE_CURVE('',#9313,#9311,#595,.T.);
#11520=EDGE_CURVE('',#9310,#9312,#596,.T.);
#11521=EDGE_CURVE('',#9314,#9315,#5730,.T.);
#11522=EDGE_CURVE('',#9315,#9313,#597,.T.);
#11523=EDGE_CURVE('',#9312,#9314,#598,.T.);
#11524=EDGE_CURVE('',#9316,#9317,#5731,.T.);
#11525=EDGE_CURVE('',#9317,#9315,#599,.T.);
#11526=EDGE_CURVE('',#9314,#9316,#600,.T.);
#11527=EDGE_CURVE('',#9318,#9319,#5732,.T.);
#11528=EDGE_CURVE('',#9320,#9318,#8048,.F.);
#11529=EDGE_CURVE('',#9320,#9319,#601,.T.);
#11530=EDGE_CURVE('',#9321,#9322,#5733,.T.);
#11531=EDGE_CURVE('',#9322,#9323,#602,.T.);
#11532=EDGE_CURVE('',#9324,#9323,#8049,.T.);
#11533=EDGE_CURVE('',#9321,#9324,#603,.T.);
#11534=EDGE_CURVE('',#9325,#9326,#5734,.T.);
#11535=EDGE_CURVE('',#9326,#9322,#604,.T.);
#11536=EDGE_CURVE('',#9325,#9321,#605,.T.);
#11537=EDGE_CURVE('',#9327,#9328,#5735,.T.);
#11538=EDGE_CURVE('',#9328,#9326,#606,.T.);
#11539=EDGE_CURVE('',#9327,#9325,#607,.T.);
#11540=EDGE_CURVE('',#9329,#9330,#5736,.T.);
#11541=EDGE_CURVE('',#9330,#9328,#608,.T.);
#11542=EDGE_CURVE('',#9329,#9327,#609,.T.);
#11543=EDGE_CURVE('',#9331,#9332,#5737,.T.);
#11544=EDGE_CURVE('',#9332,#9330,#610,.T.);
#11545=EDGE_CURVE('',#9331,#9329,#611,.T.);
#11546=EDGE_CURVE('',#9333,#9334,#5738,.T.);
#11547=EDGE_CURVE('',#9334,#9332,#612,.T.);
#11548=EDGE_CURVE('',#9333,#9331,#613,.T.);
#11549=EDGE_CURVE('',#9335,#9336,#5739,.T.);
#11550=EDGE_CURVE('',#9336,#9334,#614,.T.);
#11551=EDGE_CURVE('',#9335,#9333,#615,.T.);
#11552=EDGE_CURVE('',#9337,#9338,#5740,.T.);
#11553=EDGE_CURVE('',#9338,#9336,#616,.T.);
#11554=EDGE_CURVE('',#9337,#9335,#617,.T.);
#11555=EDGE_CURVE('',#9339,#9340,#5741,.T.);
#11556=EDGE_CURVE('',#9341,#9339,#618,.T.);
#11557=EDGE_CURVE('',#9342,#9341,#8050,.T.);
#11558=EDGE_CURVE('',#9342,#9340,#619,.T.);
#11559=EDGE_CURVE('',#9340,#9338,#620,.T.);
#11560=EDGE_CURVE('',#9339,#9337,#621,.T.);
#11561=EDGE_CURVE('',#9323,#9320,#622,.T.);
#11562=EDGE_CURVE('',#9302,#9342,#623,.T.);
#11563=EDGE_CURVE('',#9319,#9317,#624,.T.);
#11564=EDGE_CURVE('',#9343,#9324,#625,.T.);
#11565=EDGE_CURVE('',#9316,#9343,#626,.T.);
#11566=EDGE_CURVE('',#9341,#9303,#627,.T.);
#11567=EDGE_CURVE('',#9344,#9345,#5742,.T.);
#11568=EDGE_CURVE('',#9345,#9344,#8051,.T.);
#11569=EDGE_CURVE('',#9318,#9343,#8052,.F.);
#11570=EDGE_CURVE('',#9346,#9346,#8053,.T.);
#11571=EDGE_CURVE('',#9347,#9347,#8054,.T.);
#11572=EDGE_CURVE('',#9348,#9348,#8055,.T.);
#11573=EDGE_CURVE('',#9349,#9349,#8056,.T.);
#11574=EDGE_CURVE('',#9349,#9348,#5743,.T.);
#11575=EDGE_CURVE('',#9350,#9350,#8057,.T.);
#11576=EDGE_CURVE('',#9350,#9347,#5744,.T.);
#11577=EDGE_CURVE('',#9351,#9351,#8058,.T.);
#11578=EDGE_CURVE('',#9351,#9346,#5745,.T.);
#11579=EDGE_CURVE('',#9352,#9353,#5746,.T.);
#11580=EDGE_CURVE('',#9345,#9352,#5747,.T.);
#11581=EDGE_CURVE('',#9353,#9344,#5748,.T.);
#11582=EDGE_CURVE('',#9352,#9353,#8059,.T.);
#11583=EDGE_CURVE('',#9354,#9354,#8060,.T.);
#11584=EDGE_CURVE('',#9354,#9355,#5749,.T.);
#11585=EDGE_CURVE('',#9355,#9355,#8061,.T.);
#11586=EDGE_CURVE('',#9356,#9357,#5750,.T.);
#11587=EDGE_CURVE('',#9357,#9358,#5751,.T.);
#11588=EDGE_CURVE('',#9358,#9359,#5752,.T.);
#11589=EDGE_CURVE('',#9356,#9359,#5753,.T.);
#11590=EDGE_CURVE('',#9357,#9360,#5754,.T.);
#11591=EDGE_CURVE('',#9360,#9361,#5755,.T.);
#11592=EDGE_CURVE('',#9361,#9358,#5756,.T.);
#11593=EDGE_CURVE('',#9360,#9362,#5757,.T.);
#11594=EDGE_CURVE('',#9362,#9363,#5758,.T.);
#11595=EDGE_CURVE('',#9363,#9361,#5759,.T.);
#11596=EDGE_CURVE('',#9362,#9364,#5760,.T.);
#11597=EDGE_CURVE('',#9364,#9365,#5761,.T.);
#11598=EDGE_CURVE('',#9365,#9363,#5762,.T.);
#11599=EDGE_CURVE('',#9364,#9366,#5763,.T.);
#11600=EDGE_CURVE('',#9366,#9367,#5764,.T.);
#11601=EDGE_CURVE('',#9367,#9365,#5765,.T.);
#11602=EDGE_CURVE('',#9366,#9356,#5766,.T.);
#11603=EDGE_CURVE('',#9359,#9367,#5767,.T.);
#11604=EDGE_CURVE('',#9368,#9368,#8062,.T.);
#11605=EDGE_CURVE('',#9369,#9369,#8063,.T.);
#11606=EDGE_CURVE('',#9368,#9370,#5768,.T.);
#11607=EDGE_CURVE('',#9370,#9370,#8064,.T.);
#11608=EDGE_CURVE('',#9371,#9371,#8065,.T.);
#11609=EDGE_CURVE('',#9372,#9372,#8066,.T.);
#11610=EDGE_CURVE('',#9372,#9371,#5769,.T.);
#11611=EDGE_CURVE('',#9373,#9373,#8067,.T.);
#11612=EDGE_CURVE('',#9373,#9372,#5770,.T.);
#11613=EDGE_CURVE('',#9374,#9374,#8068,.T.);
#11614=EDGE_CURVE('',#9374,#9373,#5771,.T.);
#11615=EDGE_CURVE('',#9375,#9375,#8069,.T.);
#11616=EDGE_CURVE('',#9376,#9376,#8070,.F.);
#11617=EDGE_CURVE('',#9376,#9375,#5772,.T.);
#11618=EDGE_CURVE('',#9369,#9376,#5773,.T.);
#11619=EDGE_CURVE('',#9377,#9377,#8071,.T.);
#11620=EDGE_CURVE('',#9378,#9378,#8072,.T.);
#11621=EDGE_CURVE('',#9378,#9377,#5774,.T.);
#11622=EDGE_CURVE('',#9379,#9379,#8073,.T.);
#11623=EDGE_CURVE('',#9379,#9378,#5775,.T.);
#11624=EDGE_CURVE('',#9380,#9380,#8074,.T.);
#11625=EDGE_CURVE('',#9380,#9379,#5776,.T.);
#11626=EDGE_CURVE('',#9381,#9381,#8075,.T.);
#11627=EDGE_CURVE('',#9382,#9382,#8076,.F.);
#11628=EDGE_CURVE('',#9382,#9381,#5777,.T.);
#11629=EDGE_CURVE('',#9383,#9383,#8077,.F.);
#11630=EDGE_CURVE('',#9383,#9382,#5778,.T.);
#11631=EDGE_CURVE('',#9384,#9384,#8078,.T.);
#11632=EDGE_CURVE('',#9384,#9383,#5779,.T.);
#11633=EDGE_CURVE('',#9385,#9386,#5780,.T.);
#11634=EDGE_CURVE('',#9386,#9387,#5781,.T.);
#11635=EDGE_CURVE('',#9387,#9388,#5782,.T.);
#11636=EDGE_CURVE('',#9385,#9388,#5783,.T.);
#11637=EDGE_CURVE('',#9386,#9389,#5784,.T.);
#11638=EDGE_CURVE('',#9389,#9390,#5785,.T.);
#11639=EDGE_CURVE('',#9390,#9387,#5786,.T.);
#11640=EDGE_CURVE('',#9389,#9391,#5787,.T.);
#11641=EDGE_CURVE('',#9391,#9392,#5788,.T.);
#11642=EDGE_CURVE('',#9392,#9390,#5789,.T.);
#11643=EDGE_CURVE('',#9391,#9393,#5790,.T.);
#11644=EDGE_CURVE('',#9393,#9394,#5791,.T.);
#11645=EDGE_CURVE('',#9394,#9392,#5792,.T.);
#11646=EDGE_CURVE('',#9393,#9395,#5793,.T.);
#11647=EDGE_CURVE('',#9395,#9396,#5794,.T.);
#11648=EDGE_CURVE('',#9396,#9394,#5795,.T.);
#11649=EDGE_CURVE('',#9395,#9385,#5796,.T.);
#11650=EDGE_CURVE('',#9388,#9396,#5797,.T.);
#11651=EDGE_CURVE('',#9397,#9398,#5798,.T.);
#11652=EDGE_CURVE('',#9397,#9399,#628,.T.);
#11653=EDGE_CURVE('',#9399,#9400,#8079,.F.);
#11654=EDGE_CURVE('',#9400,#9398,#629,.T.);
#11655=EDGE_CURVE('',#9401,#9402,#5799,.T.);
#11656=EDGE_CURVE('',#9401,#9397,#630,.T.);
#11657=EDGE_CURVE('',#9398,#9402,#631,.T.);
#11658=EDGE_CURVE('',#9403,#9404,#5800,.T.);
#11659=EDGE_CURVE('',#9403,#9401,#632,.T.);
#11660=EDGE_CURVE('',#9402,#9404,#633,.T.);
#11661=EDGE_CURVE('',#9405,#9406,#5801,.T.);
#11662=EDGE_CURVE('',#9405,#9403,#634,.T.);
#11663=EDGE_CURVE('',#9404,#9406,#635,.T.);
#11664=EDGE_CURVE('',#9407,#9408,#5802,.T.);
#11665=EDGE_CURVE('',#9407,#9405,#636,.T.);
#11666=EDGE_CURVE('',#9406,#9408,#637,.T.);
#11667=EDGE_CURVE('',#9409,#9410,#5803,.T.);
#11668=EDGE_CURVE('',#9409,#9407,#638,.T.);
#11669=EDGE_CURVE('',#9408,#9410,#639,.T.);
#11670=EDGE_CURVE('',#9411,#9412,#5804,.T.);
#11671=EDGE_CURVE('',#9411,#9409,#640,.T.);
#11672=EDGE_CURVE('',#9410,#9412,#641,.T.);
#11673=EDGE_CURVE('',#9413,#9414,#5805,.T.);
#11674=EDGE_CURVE('',#9413,#9411,#642,.T.);
#11675=EDGE_CURVE('',#9412,#9414,#643,.T.);
#11676=EDGE_CURVE('',#9415,#9416,#5806,.T.);
#11677=EDGE_CURVE('',#9415,#9413,#644,.T.);
#11678=EDGE_CURVE('',#9414,#9416,#645,.T.);
#11679=EDGE_CURVE('',#9417,#9418,#5807,.T.);
#11680=EDGE_CURVE('',#9417,#9415,#646,.T.);
#11681=EDGE_CURVE('',#9416,#9418,#647,.T.);
#11682=EDGE_CURVE('',#9419,#9420,#5808,.T.);
#11683=EDGE_CURVE('',#9419,#9417,#648,.T.);
#11684=EDGE_CURVE('',#9418,#9420,#649,.T.);
#11685=EDGE_CURVE('',#9421,#9422,#5809,.T.);
#11686=EDGE_CURVE('',#9421,#9419,#650,.T.);
#11687=EDGE_CURVE('',#9420,#9422,#651,.T.);
#11688=EDGE_CURVE('',#9423,#9424,#5810,.T.);
#11689=EDGE_CURVE('',#9423,#9421,#652,.T.);
#11690=EDGE_CURVE('',#9422,#9424,#653,.T.);
#11691=EDGE_CURVE('',#9425,#9426,#5811,.T.);
#11692=EDGE_CURVE('',#9425,#9423,#654,.T.);
#11693=EDGE_CURVE('',#9424,#9426,#655,.T.);
#11694=EDGE_CURVE('',#9427,#9428,#5812,.T.);
#11695=EDGE_CURVE('',#9427,#9425,#656,.T.);
#11696=EDGE_CURVE('',#9426,#9428,#657,.T.);
#11697=EDGE_CURVE('',#9429,#9430,#5813,.T.);
#11698=EDGE_CURVE('',#9429,#9427,#658,.T.);
#11699=EDGE_CURVE('',#9428,#9430,#659,.T.);
#11700=EDGE_CURVE('',#9431,#9432,#5814,.T.);
#11701=EDGE_CURVE('',#9431,#9429,#660,.T.);
#11702=EDGE_CURVE('',#9430,#9432,#661,.T.);
#11703=EDGE_CURVE('',#9433,#9434,#5815,.T.);
#11704=EDGE_CURVE('',#9433,#9431,#662,.T.);
#11705=EDGE_CURVE('',#9432,#9434,#663,.T.);
#11706=EDGE_CURVE('',#9435,#9436,#5816,.T.);
#11707=EDGE_CURVE('',#9435,#9433,#664,.T.);
#11708=EDGE_CURVE('',#9434,#9436,#665,.T.);
#11709=EDGE_CURVE('',#9437,#9438,#5817,.T.);
#11710=EDGE_CURVE('',#9437,#9435,#666,.T.);
#11711=EDGE_CURVE('',#9436,#9438,#667,.T.);
#11712=EDGE_CURVE('',#9439,#9440,#5818,.T.);
#11713=EDGE_CURVE('',#9439,#9437,#668,.T.);
#11714=EDGE_CURVE('',#9438,#9440,#669,.T.);
#11715=EDGE_CURVE('',#9441,#9442,#5819,.T.);
#11716=EDGE_CURVE('',#9441,#9439,#670,.T.);
#11717=EDGE_CURVE('',#9440,#9442,#671,.T.);
#11718=EDGE_CURVE('',#9443,#9444,#5820,.T.);
#11719=EDGE_CURVE('',#9443,#9441,#672,.T.);
#11720=EDGE_CURVE('',#9442,#9444,#673,.T.);
#11721=EDGE_CURVE('',#9445,#9446,#5821,.T.);
#11722=EDGE_CURVE('',#9445,#9443,#674,.T.);
#11723=EDGE_CURVE('',#9444,#9446,#675,.T.);
#11724=EDGE_CURVE('',#9447,#9448,#5822,.T.);
#11725=EDGE_CURVE('',#9447,#9445,#676,.T.);
#11726=EDGE_CURVE('',#9446,#9448,#677,.T.);
#11727=EDGE_CURVE('',#9449,#9450,#5823,.T.);
#11728=EDGE_CURVE('',#9449,#9447,#678,.T.);
#11729=EDGE_CURVE('',#9448,#9450,#679,.T.);
#11730=EDGE_CURVE('',#9451,#9452,#5824,.T.);
#11731=EDGE_CURVE('',#9451,#9449,#680,.T.);
#11732=EDGE_CURVE('',#9450,#9452,#681,.T.);
#11733=EDGE_CURVE('',#9453,#9454,#5825,.T.);
#11734=EDGE_CURVE('',#9453,#9451,#682,.T.);
#11735=EDGE_CURVE('',#9452,#9454,#683,.T.);
#11736=EDGE_CURVE('',#9455,#9456,#5826,.T.);
#11737=EDGE_CURVE('',#9455,#9453,#684,.T.);
#11738=EDGE_CURVE('',#9454,#9456,#685,.T.);
#11739=EDGE_CURVE('',#9457,#9458,#5827,.T.);
#11740=EDGE_CURVE('',#9457,#9455,#686,.T.);
#11741=EDGE_CURVE('',#9456,#9458,#687,.T.);
#11742=EDGE_CURVE('',#9459,#9460,#5828,.T.);
#11743=EDGE_CURVE('',#9459,#9457,#688,.T.);
#11744=EDGE_CURVE('',#9458,#9460,#689,.T.);
#11745=EDGE_CURVE('',#9461,#9462,#5829,.T.);
#11746=EDGE_CURVE('',#9461,#9459,#690,.T.);
#11747=EDGE_CURVE('',#9460,#9462,#691,.T.);
#11748=EDGE_CURVE('',#9463,#9464,#5830,.T.);
#11749=EDGE_CURVE('',#9463,#9461,#692,.T.);
#11750=EDGE_CURVE('',#9462,#9464,#693,.T.);
#11751=EDGE_CURVE('',#9465,#9466,#5831,.T.);
#11752=EDGE_CURVE('',#9465,#9463,#694,.T.);
#11753=EDGE_CURVE('',#9464,#9466,#695,.T.);
#11754=EDGE_CURVE('',#9467,#9468,#5832,.T.);
#11755=EDGE_CURVE('',#9467,#9465,#696,.T.);
#11756=EDGE_CURVE('',#9466,#9468,#697,.T.);
#11757=EDGE_CURVE('',#9469,#9470,#5833,.T.);
#11758=EDGE_CURVE('',#9469,#9467,#698,.T.);
#11759=EDGE_CURVE('',#9468,#9470,#699,.T.);
#11760=EDGE_CURVE('',#9471,#9472,#5834,.T.);
#11761=EDGE_CURVE('',#9471,#9469,#700,.T.);
#11762=EDGE_CURVE('',#9470,#9472,#701,.T.);
#11763=EDGE_CURVE('',#9473,#9474,#5835,.T.);
#11764=EDGE_CURVE('',#9473,#9471,#702,.T.);
#11765=EDGE_CURVE('',#9472,#9474,#703,.T.);
#11766=EDGE_CURVE('',#9475,#9476,#5836,.T.);
#11767=EDGE_CURVE('',#9475,#9473,#704,.T.);
#11768=EDGE_CURVE('',#9474,#9476,#705,.T.);
#11769=EDGE_CURVE('',#9477,#9478,#5837,.T.);
#11770=EDGE_CURVE('',#9477,#9475,#706,.T.);
#11771=EDGE_CURVE('',#9476,#9478,#707,.T.);
#11772=EDGE_CURVE('',#9479,#9480,#5838,.T.);
#11773=EDGE_CURVE('',#9479,#9477,#708,.T.);
#11774=EDGE_CURVE('',#9478,#9480,#709,.T.);
#11775=EDGE_CURVE('',#9481,#9482,#5839,.T.);
#11776=EDGE_CURVE('',#9481,#9479,#710,.T.);
#11777=EDGE_CURVE('',#9480,#9482,#711,.T.);
#11778=EDGE_CURVE('',#9483,#9484,#5840,.T.);
#11779=EDGE_CURVE('',#9483,#9481,#712,.T.);
#11780=EDGE_CURVE('',#9482,#9484,#713,.T.);
#11781=EDGE_CURVE('',#9485,#9486,#5841,.T.);
#11782=EDGE_CURVE('',#9485,#9483,#714,.T.);
#11783=EDGE_CURVE('',#9484,#9486,#715,.T.);
#11784=EDGE_CURVE('',#9487,#9488,#5842,.T.);
#11785=EDGE_CURVE('',#9487,#9485,#716,.T.);
#11786=EDGE_CURVE('',#9486,#9488,#717,.T.);
#11787=EDGE_CURVE('',#9489,#9490,#5843,.T.);
#11788=EDGE_CURVE('',#9489,#9487,#718,.T.);
#11789=EDGE_CURVE('',#9488,#9490,#719,.T.);
#11790=EDGE_CURVE('',#9491,#9492,#5844,.T.);
#11791=EDGE_CURVE('',#9491,#9489,#720,.T.);
#11792=EDGE_CURVE('',#9490,#9492,#721,.T.);
#11793=EDGE_CURVE('',#9493,#9494,#5845,.T.);
#11794=EDGE_CURVE('',#9493,#9491,#722,.T.);
#11795=EDGE_CURVE('',#9492,#9494,#723,.T.);
#11796=EDGE_CURVE('',#9495,#9496,#5846,.T.);
#11797=EDGE_CURVE('',#9495,#9493,#724,.T.);
#11798=EDGE_CURVE('',#9494,#9496,#725,.T.);
#11799=EDGE_CURVE('',#9497,#9498,#5847,.T.);
#11800=EDGE_CURVE('',#9497,#9495,#726,.T.);
#11801=EDGE_CURVE('',#9496,#9498,#727,.T.);
#11802=EDGE_CURVE('',#9499,#9500,#5848,.T.);
#11803=EDGE_CURVE('',#9499,#9497,#728,.T.);
#11804=EDGE_CURVE('',#9498,#9500,#729,.T.);
#11805=EDGE_CURVE('',#9501,#9502,#5849,.T.);
#11806=EDGE_CURVE('',#9501,#9499,#730,.T.);
#11807=EDGE_CURVE('',#9500,#9502,#731,.T.);
#11808=EDGE_CURVE('',#9503,#9504,#5850,.T.);
#11809=EDGE_CURVE('',#9503,#9501,#732,.T.);
#11810=EDGE_CURVE('',#9502,#9504,#733,.T.);
#11811=EDGE_CURVE('',#9505,#9506,#5851,.T.);
#11812=EDGE_CURVE('',#9505,#9503,#734,.T.);
#11813=EDGE_CURVE('',#9504,#9506,#735,.T.);
#11814=EDGE_CURVE('',#9507,#9508,#5852,.T.);
#11815=EDGE_CURVE('',#9507,#9505,#736,.T.);
#11816=EDGE_CURVE('',#9506,#9508,#737,.T.);
#11817=EDGE_CURVE('',#9509,#9510,#5853,.T.);
#11818=EDGE_CURVE('',#9509,#9507,#738,.T.);
#11819=EDGE_CURVE('',#9508,#9510,#739,.T.);
#11820=EDGE_CURVE('',#9511,#9512,#5854,.T.);
#11821=EDGE_CURVE('',#9511,#9509,#740,.T.);
#11822=EDGE_CURVE('',#9510,#9512,#741,.T.);
#11823=EDGE_CURVE('',#9513,#9514,#5855,.T.);
#11824=EDGE_CURVE('',#9513,#9511,#742,.T.);
#11825=EDGE_CURVE('',#9512,#9514,#743,.T.);
#11826=EDGE_CURVE('',#9515,#9516,#5856,.T.);
#11827=EDGE_CURVE('',#9515,#9513,#744,.T.);
#11828=EDGE_CURVE('',#9514,#9516,#745,.T.);
#11829=EDGE_CURVE('',#9517,#9518,#5857,.T.);
#11830=EDGE_CURVE('',#9517,#9515,#746,.T.);
#11831=EDGE_CURVE('',#9516,#9518,#747,.T.);
#11832=EDGE_CURVE('',#9519,#9520,#5858,.T.);
#11833=EDGE_CURVE('',#9519,#9517,#748,.T.);
#11834=EDGE_CURVE('',#9518,#9520,#749,.T.);
#11835=EDGE_CURVE('',#9521,#9522,#5859,.T.);
#11836=EDGE_CURVE('',#9521,#9519,#750,.T.);
#11837=EDGE_CURVE('',#9520,#9522,#751,.T.);
#11838=EDGE_CURVE('',#9523,#9524,#5860,.T.);
#11839=EDGE_CURVE('',#9523,#9521,#752,.T.);
#11840=EDGE_CURVE('',#9522,#9524,#753,.T.);
#11841=EDGE_CURVE('',#9525,#9526,#5861,.T.);
#11842=EDGE_CURVE('',#9525,#9527,#754,.T.);
#11843=EDGE_CURVE('',#9526,#9527,#8080,.T.);
#11844=EDGE_CURVE('',#9528,#9529,#5862,.T.);
#11845=EDGE_CURVE('',#9528,#9525,#755,.T.);
#11846=EDGE_CURVE('',#9530,#9526,#8081,.T.);
#11847=EDGE_CURVE('',#9529,#9530,#756,.T.);
#11848=EDGE_CURVE('',#9531,#9532,#5863,.T.);
#11849=EDGE_CURVE('',#9531,#9528,#757,.T.);
#11850=EDGE_CURVE('',#9532,#9529,#758,.T.);
#11851=EDGE_CURVE('',#9533,#9534,#5864,.T.);
#11852=EDGE_CURVE('',#9533,#9531,#759,.T.);
#11853=EDGE_CURVE('',#9534,#9532,#760,.T.);
#11854=EDGE_CURVE('',#9535,#9536,#5865,.T.);
#11855=EDGE_CURVE('',#9535,#9533,#761,.T.);
#11856=EDGE_CURVE('',#9536,#9534,#762,.T.);
#11857=EDGE_CURVE('',#9537,#9538,#5866,.T.);
#11858=EDGE_CURVE('',#9537,#9535,#763,.T.);
#11859=EDGE_CURVE('',#9538,#9536,#764,.T.);
#11860=EDGE_CURVE('',#9539,#9540,#5867,.T.);
#11861=EDGE_CURVE('',#9539,#9537,#765,.T.);
#11862=EDGE_CURVE('',#9540,#9538,#766,.T.);
#11863=EDGE_CURVE('',#9541,#9542,#5868,.T.);
#11864=EDGE_CURVE('',#9541,#9539,#767,.T.);
#11865=EDGE_CURVE('',#9542,#9540,#768,.T.);
#11866=EDGE_CURVE('',#9543,#9544,#5869,.T.);
#11867=EDGE_CURVE('',#9543,#9541,#769,.T.);
#11868=EDGE_CURVE('',#9544,#9542,#770,.T.);
#11869=EDGE_CURVE('',#9545,#9546,#5870,.T.);
#11870=EDGE_CURVE('',#9545,#9543,#771,.T.);
#11871=EDGE_CURVE('',#9546,#9544,#772,.T.);
#11872=EDGE_CURVE('',#9547,#9548,#5871,.T.);
#11873=EDGE_CURVE('',#9547,#9545,#773,.T.);
#11874=EDGE_CURVE('',#9548,#9546,#774,.T.);
#11875=EDGE_CURVE('',#9549,#9550,#5872,.T.);
#11876=EDGE_CURVE('',#9549,#9547,#775,.T.);
#11877=EDGE_CURVE('',#9550,#9548,#776,.T.);
#11878=EDGE_CURVE('',#9551,#9552,#5873,.T.);
#11879=EDGE_CURVE('',#9551,#9549,#777,.T.);
#11880=EDGE_CURVE('',#9552,#9550,#778,.T.);
#11881=EDGE_CURVE('',#9553,#9554,#5874,.T.);
#11882=EDGE_CURVE('',#9553,#9551,#779,.T.);
#11883=EDGE_CURVE('',#9554,#9552,#780,.T.);
#11884=EDGE_CURVE('',#9555,#9556,#5875,.T.);
#11885=EDGE_CURVE('',#9555,#9553,#781,.T.);
#11886=EDGE_CURVE('',#9556,#9554,#782,.T.);
#11887=EDGE_CURVE('',#9557,#9558,#5876,.T.);
#11888=EDGE_CURVE('',#9557,#9555,#783,.T.);
#11889=EDGE_CURVE('',#9558,#9556,#784,.T.);
#11890=EDGE_CURVE('',#9559,#9560,#5877,.T.);
#11891=EDGE_CURVE('',#9559,#9557,#785,.T.);
#11892=EDGE_CURVE('',#9560,#9558,#786,.T.);
#11893=EDGE_CURVE('',#9561,#9562,#5878,.T.);
#11894=EDGE_CURVE('',#9561,#9559,#787,.T.);
#11895=EDGE_CURVE('',#9562,#9560,#788,.T.);
#11896=EDGE_CURVE('',#9563,#9564,#5879,.T.);
#11897=EDGE_CURVE('',#9563,#9561,#789,.T.);
#11898=EDGE_CURVE('',#9564,#9562,#790,.T.);
#11899=EDGE_CURVE('',#9565,#9566,#5880,.T.);
#11900=EDGE_CURVE('',#9565,#9563,#791,.T.);
#11901=EDGE_CURVE('',#9566,#9564,#792,.T.);
#11902=EDGE_CURVE('',#9567,#9568,#5881,.T.);
#11903=EDGE_CURVE('',#9567,#9565,#793,.T.);
#11904=EDGE_CURVE('',#9568,#9566,#794,.T.);
#11905=EDGE_CURVE('',#9569,#9570,#5882,.T.);
#11906=EDGE_CURVE('',#9569,#9567,#795,.T.);
#11907=EDGE_CURVE('',#9570,#9568,#796,.T.);
#11908=EDGE_CURVE('',#9571,#9572,#5883,.T.);
#11909=EDGE_CURVE('',#9571,#9569,#797,.T.);
#11910=EDGE_CURVE('',#9572,#9570,#798,.T.);
#11911=EDGE_CURVE('',#9573,#9574,#5884,.T.);
#11912=EDGE_CURVE('',#9573,#9571,#799,.T.);
#11913=EDGE_CURVE('',#9574,#9572,#800,.T.);
#11914=EDGE_CURVE('',#9575,#9576,#5885,.T.);
#11915=EDGE_CURVE('',#9575,#9573,#801,.T.);
#11916=EDGE_CURVE('',#9576,#9574,#802,.T.);
#11917=EDGE_CURVE('',#9577,#9578,#5886,.T.);
#11918=EDGE_CURVE('',#9577,#9575,#803,.T.);
#11919=EDGE_CURVE('',#9578,#9576,#804,.T.);
#11920=EDGE_CURVE('',#9579,#9580,#5887,.T.);
#11921=EDGE_CURVE('',#9579,#9577,#805,.T.);
#11922=EDGE_CURVE('',#9580,#9578,#806,.T.);
#11923=EDGE_CURVE('',#9581,#9582,#5888,.T.);
#11924=EDGE_CURVE('',#9581,#9579,#807,.T.);
#11925=EDGE_CURVE('',#9582,#9580,#808,.T.);
#11926=EDGE_CURVE('',#9583,#9584,#5889,.T.);
#11927=EDGE_CURVE('',#9583,#9581,#809,.T.);
#11928=EDGE_CURVE('',#9584,#9582,#810,.T.);
#11929=EDGE_CURVE('',#9585,#9586,#5890,.T.);
#11930=EDGE_CURVE('',#9585,#9583,#811,.T.);
#11931=EDGE_CURVE('',#9586,#9584,#812,.T.);
#11932=EDGE_CURVE('',#9587,#9588,#5891,.T.);
#11933=EDGE_CURVE('',#9587,#9585,#813,.T.);
#11934=EDGE_CURVE('',#9588,#9586,#814,.T.);
#11935=EDGE_CURVE('',#9589,#9590,#5892,.T.);
#11936=EDGE_CURVE('',#9589,#9587,#815,.T.);
#11937=EDGE_CURVE('',#9590,#9588,#816,.T.);
#11938=EDGE_CURVE('',#9591,#9592,#5893,.T.);
#11939=EDGE_CURVE('',#9591,#9589,#817,.T.);
#11940=EDGE_CURVE('',#9592,#9590,#818,.T.);
#11941=EDGE_CURVE('',#9593,#9594,#5894,.T.);
#11942=EDGE_CURVE('',#9593,#9591,#819,.T.);
#11943=EDGE_CURVE('',#9594,#9592,#820,.T.);
#11944=EDGE_CURVE('',#9595,#9596,#5895,.T.);
#11945=EDGE_CURVE('',#9595,#9593,#821,.T.);
#11946=EDGE_CURVE('',#9596,#9594,#822,.T.);
#11947=EDGE_CURVE('',#9597,#9598,#5896,.T.);
#11948=EDGE_CURVE('',#9597,#9595,#823,.T.);
#11949=EDGE_CURVE('',#9598,#9596,#824,.T.);
#11950=EDGE_CURVE('',#9599,#9600,#5897,.T.);
#11951=EDGE_CURVE('',#9599,#9597,#825,.T.);
#11952=EDGE_CURVE('',#9600,#9598,#826,.T.);
#11953=EDGE_CURVE('',#9601,#9602,#5898,.T.);
#11954=EDGE_CURVE('',#9601,#9599,#827,.T.);
#11955=EDGE_CURVE('',#9602,#9600,#828,.T.);
#11956=EDGE_CURVE('',#9603,#9604,#5899,.T.);
#11957=EDGE_CURVE('',#9603,#9601,#829,.T.);
#11958=EDGE_CURVE('',#9604,#9602,#830,.T.);
#11959=EDGE_CURVE('',#9605,#9606,#5900,.T.);
#11960=EDGE_CURVE('',#9605,#9603,#831,.T.);
#11961=EDGE_CURVE('',#9606,#9604,#832,.T.);
#11962=EDGE_CURVE('',#9607,#9608,#5901,.T.);
#11963=EDGE_CURVE('',#9607,#9605,#833,.T.);
#11964=EDGE_CURVE('',#9608,#9606,#834,.T.);
#11965=EDGE_CURVE('',#9609,#9610,#5902,.T.);
#11966=EDGE_CURVE('',#9609,#9607,#835,.T.);
#11967=EDGE_CURVE('',#9610,#9608,#836,.T.);
#11968=EDGE_CURVE('',#9611,#9612,#5903,.T.);
#11969=EDGE_CURVE('',#9611,#9609,#837,.T.);
#11970=EDGE_CURVE('',#9612,#9610,#838,.T.);
#11971=EDGE_CURVE('',#9613,#9614,#5904,.T.);
#11972=EDGE_CURVE('',#9613,#9611,#839,.T.);
#11973=EDGE_CURVE('',#9614,#9612,#840,.T.);
#11974=EDGE_CURVE('',#9615,#9616,#5905,.T.);
#11975=EDGE_CURVE('',#9615,#9613,#841,.T.);
#11976=EDGE_CURVE('',#9616,#9614,#842,.T.);
#11977=EDGE_CURVE('',#9617,#9618,#5906,.T.);
#11978=EDGE_CURVE('',#9617,#9615,#843,.T.);
#11979=EDGE_CURVE('',#9618,#9616,#844,.T.);
#11980=EDGE_CURVE('',#9619,#9620,#5907,.T.);
#11981=EDGE_CURVE('',#9619,#9617,#845,.T.);
#11982=EDGE_CURVE('',#9620,#9618,#846,.T.);
#11983=EDGE_CURVE('',#9621,#9622,#5908,.T.);
#11984=EDGE_CURVE('',#9621,#9619,#847,.T.);
#11985=EDGE_CURVE('',#9622,#9620,#848,.T.);
#11986=EDGE_CURVE('',#9623,#9624,#5909,.T.);
#11987=EDGE_CURVE('',#9623,#9621,#849,.T.);
#11988=EDGE_CURVE('',#9624,#9622,#850,.T.);
#11989=EDGE_CURVE('',#9625,#9626,#5910,.T.);
#11990=EDGE_CURVE('',#9625,#9623,#851,.T.);
#11991=EDGE_CURVE('',#9626,#9624,#852,.T.);
#11992=EDGE_CURVE('',#9627,#9628,#5911,.T.);
#11993=EDGE_CURVE('',#9627,#9625,#853,.T.);
#11994=EDGE_CURVE('',#9628,#9626,#854,.T.);
#11995=EDGE_CURVE('',#9629,#9630,#5912,.T.);
#11996=EDGE_CURVE('',#9629,#9627,#855,.T.);
#11997=EDGE_CURVE('',#9630,#9628,#856,.T.);
#11998=EDGE_CURVE('',#9631,#9632,#5913,.T.);
#11999=EDGE_CURVE('',#9631,#9629,#857,.T.);
#12000=EDGE_CURVE('',#9632,#9630,#858,.T.);
#12001=EDGE_CURVE('',#9633,#9634,#5914,.T.);
#12002=EDGE_CURVE('',#9633,#9631,#859,.T.);
#12003=EDGE_CURVE('',#9634,#9632,#860,.T.);
#12004=EDGE_CURVE('',#9635,#9636,#5915,.T.);
#12005=EDGE_CURVE('',#9635,#9633,#861,.T.);
#12006=EDGE_CURVE('',#9636,#9634,#862,.T.);
#12007=EDGE_CURVE('',#9637,#9638,#5916,.T.);
#12008=EDGE_CURVE('',#9637,#9635,#863,.T.);
#12009=EDGE_CURVE('',#9638,#9636,#864,.T.);
#12010=EDGE_CURVE('',#9639,#9640,#5917,.T.);
#12011=EDGE_CURVE('',#9639,#9637,#865,.T.);
#12012=EDGE_CURVE('',#9640,#9638,#866,.T.);
#12013=EDGE_CURVE('',#9641,#9642,#5918,.T.);
#12014=EDGE_CURVE('',#9641,#9639,#867,.T.);
#12015=EDGE_CURVE('',#9642,#9640,#868,.T.);
#12016=EDGE_CURVE('',#9643,#9644,#5919,.T.);
#12017=EDGE_CURVE('',#9643,#9641,#869,.T.);
#12018=EDGE_CURVE('',#9644,#9642,#870,.T.);
#12019=EDGE_CURVE('',#9645,#9646,#5920,.T.);
#12020=EDGE_CURVE('',#9645,#9643,#871,.T.);
#12021=EDGE_CURVE('',#9646,#9644,#872,.T.);
#12022=EDGE_CURVE('',#9647,#9648,#5921,.T.);
#12023=EDGE_CURVE('',#9647,#9645,#873,.T.);
#12024=EDGE_CURVE('',#9648,#9646,#874,.T.);
#12025=EDGE_CURVE('',#9649,#9650,#5922,.T.);
#12026=EDGE_CURVE('',#9649,#9647,#875,.T.);
#12027=EDGE_CURVE('',#9650,#9648,#876,.T.);
#12028=EDGE_CURVE('',#9651,#9652,#5923,.T.);
#12029=EDGE_CURVE('',#9651,#9649,#877,.T.);
#12030=EDGE_CURVE('',#9652,#9650,#878,.T.);
#12031=EDGE_CURVE('',#9653,#9653,#8082,.T.);
#12032=EDGE_CURVE('',#9654,#9400,#879,.T.);
#12033=EDGE_CURVE('',#9399,#9655,#880,.T.);
#12034=EDGE_CURVE('',#9655,#9654,#8083,.T.);
#12035=EDGE_CURVE('',#9653,#9656,#5924,.T.);
#12036=EDGE_CURVE('',#9656,#9656,#8084,.T.);
#12037=EDGE_CURVE('',#9657,#9530,#881,.T.);
#12038=EDGE_CURVE('',#9524,#9657,#882,.T.);
#12039=EDGE_CURVE('',#9654,#9652,#883,.T.);
#12040=EDGE_CURVE('',#9655,#9651,#884,.T.);
#12041=EDGE_CURVE('',#9527,#9658,#885,.T.);
#12042=EDGE_CURVE('',#9658,#9523,#886,.T.);
#12043=EDGE_CURVE('',#9659,#9660,#5925,.T.);
#12044=EDGE_CURVE('',#9659,#9661,#5926,.T.);
#12045=EDGE_CURVE('',#9662,#9661,#5927,.T.);
#12046=EDGE_CURVE('',#9660,#9662,#5928,.T.);
#12047=EDGE_CURVE('',#9660,#9663,#8085,.T.);
#12048=EDGE_CURVE('',#9662,#9664,#5929,.T.);
#12049=EDGE_CURVE('',#9664,#9663,#5930,.T.);
#12050=EDGE_CURVE('',#9661,#9665,#5931,.T.);
#12051=EDGE_CURVE('',#9664,#9665,#5932,.T.);
#12052=EDGE_CURVE('',#9663,#9666,#5933,.T.);
#12053=EDGE_CURVE('',#9665,#9666,#5934,.T.);
#12054=EDGE_CURVE('',#9666,#9659,#8086,.T.);
#12055=EDGE_CURVE('',#9667,#9667,#8087,.T.);
#12056=EDGE_CURVE('',#9667,#9668,#5935,.T.);
#12057=EDGE_CURVE('',#9668,#9668,#8088,.T.);
#12058=EDGE_CURVE('',#9669,#9669,#8089,.T.);
#12059=EDGE_CURVE('',#9658,#9657,#8090,.F.);
#12060=EDGE_CURVE('',#9670,#9670,#8091,.T.);
#12061=EDGE_CURVE('',#9670,#9669,#5936,.T.);
#12062=EDGE_CURVE('',#9671,#9671,#8092,.T.);
#12063=EDGE_CURVE('',#9671,#9672,#5937,.T.);
#12064=EDGE_CURVE('',#9672,#9672,#8093,.T.);
#12065=EDGE_CURVE('',#9673,#9673,#8094,.T.);
#12066=EDGE_CURVE('',#9673,#9674,#5938,.T.);
#12067=EDGE_CURVE('',#9674,#9674,#8095,.T.);
#12068=EDGE_CURVE('',#9675,#9676,#5939,.T.);
#12069=EDGE_CURVE('',#9675,#9676,#8096,.T.);
#12070=EDGE_CURVE('',#9677,#9678,#887,.T.);
#12071=EDGE_CURVE('',#9679,#9677,#8097,.T.);
#12072=EDGE_CURVE('',#9676,#9679,#888,.T.);
#12073=EDGE_CURVE('',#9678,#9675,#889,.T.);
#12074=EDGE_CURVE('',#9678,#9680,#5940,.T.);
#12075=EDGE_CURVE('',#9681,#9680,#890,.T.);
#12076=EDGE_CURVE('',#9680,#9681,#891,.T.);
#12077=EDGE_CURVE('',#9679,#9677,#5941,.T.);
#12078=EDGE_CURVE('',#9682,#9682,#8098,.T.);
#12079=EDGE_CURVE('',#9682,#9683,#5942,.T.);
#12080=EDGE_CURVE('',#9683,#9683,#8099,.T.);
#12081=EDGE_CURVE('',#9684,#9684,#8100,.T.);
#12082=EDGE_CURVE('',#9684,#9685,#5943,.T.);
#12083=EDGE_CURVE('',#9685,#9685,#8101,.T.);
#12084=EDGE_CURVE('',#9686,#9686,#8102,.T.);
#12085=EDGE_CURVE('',#9686,#9687,#5944,.T.);
#12086=EDGE_CURVE('',#9687,#9687,#8103,.T.);
#12087=EDGE_CURVE('',#9688,#9689,#5945,.T.);
#12088=EDGE_CURVE('',#9688,#9689,#8104,.T.);
#12089=EDGE_CURVE('',#9690,#9691,#892,.T.);
#12090=EDGE_CURVE('',#9692,#9690,#8105,.T.);
#12091=EDGE_CURVE('',#9689,#9692,#893,.T.);
#12092=EDGE_CURVE('',#9691,#9688,#894,.T.);
#12093=EDGE_CURVE('',#9691,#9693,#5946,.T.);
#12094=EDGE_CURVE('',#9694,#9693,#895,.T.);
#12095=EDGE_CURVE('',#9693,#9694,#896,.T.);
#12096=EDGE_CURVE('',#9692,#9690,#5947,.T.);
#12097=EDGE_CURVE('',#9695,#9696,#5948,.T.);
#12098=EDGE_CURVE('',#9697,#9695,#5949,.T.);
#12099=EDGE_CURVE('',#9698,#9697,#5950,.T.);
#12100=EDGE_CURVE('',#9699,#9698,#5951,.T.);
#12101=EDGE_CURVE('',#9700,#9699,#5952,.T.);
#12102=EDGE_CURVE('',#9696,#9700,#5953,.T.);
#12103=EDGE_CURVE('',#9701,#9695,#5954,.T.);
#12104=EDGE_CURVE('',#9702,#9701,#5955,.T.);
#12105=EDGE_CURVE('',#9697,#9702,#5956,.T.);
#12106=EDGE_CURVE('',#9703,#9701,#5957,.T.);
#12107=EDGE_CURVE('',#9704,#9703,#5958,.T.);
#12108=EDGE_CURVE('',#9705,#9704,#5959,.T.);
#12109=EDGE_CURVE('',#9706,#9705,#5960,.T.);
#12110=EDGE_CURVE('',#9702,#9706,#5961,.T.);
#12111=EDGE_CURVE('',#9707,#9707,#8106,.T.);
#12112=EDGE_CURVE('',#9696,#9703,#8107,.T.);
#12113=EDGE_CURVE('',#9708,#9708,#8108,.T.);
#12114=EDGE_CURVE('',#9706,#9698,#8109,.T.);
#12115=EDGE_CURVE('',#9707,#9708,#5962,.T.);
#12116=EDGE_CURVE('',#9700,#9704,#8110,.T.);
#12117=EDGE_CURVE('',#9705,#9699,#8111,.T.);
#12118=EDGE_CURVE('',#9709,#9709,#8112,.T.);
#12119=EDGE_CURVE('',#9709,#9710,#5963,.T.);
#12120=EDGE_CURVE('',#9710,#9710,#8113,.T.);
#12121=EDGE_CURVE('',#9711,#9711,#8114,.T.);
#12122=EDGE_CURVE('',#9711,#9712,#5964,.T.);
#12123=EDGE_CURVE('',#9712,#9712,#8115,.T.);
#12124=EDGE_CURVE('',#9713,#9713,#8116,.T.);
#12125=EDGE_CURVE('',#9713,#9714,#5965,.T.);
#12126=EDGE_CURVE('',#9714,#9714,#8117,.T.);
#12127=EDGE_CURVE('',#9715,#9715,#8118,.T.);
#12128=EDGE_CURVE('',#9715,#9716,#5966,.T.);
#12129=EDGE_CURVE('',#9716,#9716,#8119,.T.);
#12130=EDGE_CURVE('',#9717,#9718,#5967,.T.);
#12131=EDGE_CURVE('',#9719,#9717,#5968,.T.);
#12132=EDGE_CURVE('',#9720,#9719,#5969,.T.);
#12133=EDGE_CURVE('',#9721,#9720,#5970,.T.);
#12134=EDGE_CURVE('',#9722,#9721,#5971,.T.);
#12135=EDGE_CURVE('',#9723,#9722,#5972,.T.);
#12136=EDGE_CURVE('',#9724,#9723,#5973,.T.);
#12137=EDGE_CURVE('',#9718,#9724,#5974,.T.);
#12138=EDGE_CURVE('',#9721,#9725,#5975,.T.);
#12139=EDGE_CURVE('',#9725,#9726,#5976,.T.);
#12140=EDGE_CURVE('',#9726,#9722,#5977,.T.);
#12141=EDGE_CURVE('',#9727,#9720,#5978,.T.);
#12142=EDGE_CURVE('',#9727,#9725,#5979,.T.);
#12143=EDGE_CURVE('',#9719,#9728,#5980,.T.);
#12144=EDGE_CURVE('',#9728,#9727,#5981,.T.);
#12145=EDGE_CURVE('',#9729,#9717,#5982,.T.);
#12146=EDGE_CURVE('',#9729,#9728,#5983,.T.);
#12147=EDGE_CURVE('',#9730,#9731,#5984,.T.);
#12148=EDGE_CURVE('',#9726,#9730,#5985,.T.);
#12149=EDGE_CURVE('',#9732,#9729,#5986,.T.);
#12150=EDGE_CURVE('',#9731,#9732,#5987,.T.);
#12151=EDGE_CURVE('',#9723,#9730,#5988,.T.);
#12152=EDGE_CURVE('',#9718,#9732,#5989,.T.);
#12153=EDGE_CURVE('',#9731,#9724,#5990,.T.);
#12154=EDGE_CURVE('',#9733,#9734,#5991,.T.);
#12155=EDGE_CURVE('',#9733,#9735,#5992,.T.);
#12156=EDGE_CURVE('',#9735,#9736,#5993,.T.);
#12157=EDGE_CURVE('',#9734,#9736,#5994,.T.);
#12158=EDGE_CURVE('',#9737,#9733,#5995,.T.);
#12159=EDGE_CURVE('',#9737,#9738,#5996,.T.);
#12160=EDGE_CURVE('',#9738,#9735,#5997,.T.);
#12161=EDGE_CURVE('',#9739,#9737,#5998,.T.);
#12162=EDGE_CURVE('',#9739,#9740,#5999,.T.);
#12163=EDGE_CURVE('',#9740,#9738,#6000,.T.);
#12164=EDGE_CURVE('',#9741,#9739,#6001,.T.);
#12165=EDGE_CURVE('',#9741,#9742,#6002,.T.);
#12166=EDGE_CURVE('',#9742,#9740,#6003,.T.);
#12167=EDGE_CURVE('',#9743,#9741,#6004,.T.);
#12168=EDGE_CURVE('',#9743,#9744,#6005,.T.);
#12169=EDGE_CURVE('',#9744,#9742,#6006,.T.);
#12170=EDGE_CURVE('',#9734,#9743,#6007,.T.);
#12171=EDGE_CURVE('',#9736,#9744,#6008,.T.);
#12172=EDGE_CURVE('',#9745,#9745,#8120,.T.);
#12173=EDGE_CURVE('',#9746,#9746,#8121,.T.);
#12174=EDGE_CURVE('',#9746,#9745,#6009,.T.);
#12175=EDGE_CURVE('',#9747,#9747,#8122,.F.);
#12176=EDGE_CURVE('',#9747,#9746,#6010,.T.);
#12177=EDGE_CURVE('',#9748,#9748,#8123,.T.);
#12178=EDGE_CURVE('',#9748,#9747,#6011,.T.);
#12179=EDGE_CURVE('',#9749,#9749,#8124,.T.);
#12180=EDGE_CURVE('',#9749,#9750,#6012,.T.);
#12181=EDGE_CURVE('',#9750,#9750,#8125,.T.);
#12182=EDGE_CURVE('',#9751,#9751,#8126,.T.);
#12183=EDGE_CURVE('',#9751,#9752,#6013,.T.);
#12184=EDGE_CURVE('',#9752,#9752,#8127,.T.);
#12185=EDGE_CURVE('',#9753,#9753,#8128,.T.);
#12186=EDGE_CURVE('',#9754,#9754,#8129,.T.);
#12187=EDGE_CURVE('',#9754,#9753,#6014,.T.);
#12188=EDGE_CURVE('',#9755,#9755,#8130,.T.);
#12189=EDGE_CURVE('',#9755,#9754,#6015,.T.);
#12190=EDGE_CURVE('',#9756,#9756,#8131,.T.);
#12191=EDGE_CURVE('',#9756,#9755,#6016,.T.);
#12192=EDGE_CURVE('',#9757,#9757,#8132,.T.);
#12193=EDGE_CURVE('',#9758,#9758,#8133,.F.);
#12194=EDGE_CURVE('',#9758,#9757,#6017,.T.);
#12195=EDGE_CURVE('',#9759,#9759,#8134,.F.);
#12196=EDGE_CURVE('',#9759,#9758,#6018,.T.);
#12197=EDGE_CURVE('',#9760,#9760,#8135,.T.);
#12198=EDGE_CURVE('',#9760,#9759,#6019,.T.);
#12199=EDGE_CURVE('',#9761,#9762,#6020,.T.);
#12200=EDGE_CURVE('',#9762,#9763,#6021,.T.);
#12201=EDGE_CURVE('',#9763,#9764,#6022,.T.);
#12202=EDGE_CURVE('',#9761,#9764,#6023,.T.);
#12203=EDGE_CURVE('',#9762,#9765,#6024,.T.);
#12204=EDGE_CURVE('',#9765,#9766,#6025,.T.);
#12205=EDGE_CURVE('',#9766,#9763,#6026,.T.);
#12206=EDGE_CURVE('',#9765,#9767,#6027,.T.);
#12207=EDGE_CURVE('',#9767,#9768,#6028,.T.);
#12208=EDGE_CURVE('',#9768,#9766,#6029,.T.);
#12209=EDGE_CURVE('',#9767,#9769,#6030,.T.);
#12210=EDGE_CURVE('',#9769,#9770,#6031,.T.);
#12211=EDGE_CURVE('',#9770,#9768,#6032,.T.);
#12212=EDGE_CURVE('',#9769,#9771,#6033,.T.);
#12213=EDGE_CURVE('',#9771,#9772,#6034,.T.);
#12214=EDGE_CURVE('',#9772,#9770,#6035,.T.);
#12215=EDGE_CURVE('',#9771,#9761,#6036,.T.);
#12216=EDGE_CURVE('',#9764,#9772,#6037,.T.);
#12217=ORIENTED_EDGE('',*,*,#9773,.F.);
#12218=ORIENTED_EDGE('',*,*,#9774,.T.);
#12219=ORIENTED_EDGE('',*,*,#9775,.F.);
#12220=ORIENTED_EDGE('',*,*,#9774,.F.);
#12221=ORIENTED_EDGE('',*,*,#9776,.F.);
#12222=ORIENTED_EDGE('',*,*,#9777,.T.);
#12223=ORIENTED_EDGE('',*,*,#9778,.T.);
#12224=ORIENTED_EDGE('',*,*,#9779,.T.);
#12225=ORIENTED_EDGE('',*,*,#9780,.F.);
#12226=ORIENTED_EDGE('',*,*,#9781,.T.);
#12227=ORIENTED_EDGE('',*,*,#9778,.F.);
#12228=ORIENTED_EDGE('',*,*,#9782,.F.);
#12229=ORIENTED_EDGE('',*,*,#9783,.F.);
#12230=ORIENTED_EDGE('',*,*,#9784,.T.);
#12231=ORIENTED_EDGE('',*,*,#9780,.T.);
#12232=ORIENTED_EDGE('',*,*,#9785,.T.);
#12233=ORIENTED_EDGE('',*,*,#9776,.T.);
#12234=ORIENTED_EDGE('',*,*,#9786,.T.);
#12235=ORIENTED_EDGE('',*,*,#9787,.T.);
#12236=ORIENTED_EDGE('',*,*,#9788,.F.);
#12237=ORIENTED_EDGE('',*,*,#9783,.T.);
#12238=ORIENTED_EDGE('',*,*,#9789,.F.);
#12239=ORIENTED_EDGE('',*,*,#9790,.F.);
#12240=ORIENTED_EDGE('',*,*,#9791,.T.);
#12241=ORIENTED_EDGE('',*,*,#9792,.F.);
#12242=ORIENTED_EDGE('',*,*,#9793,.T.);
#12243=ORIENTED_EDGE('',*,*,#9794,.F.);
#12244=ORIENTED_EDGE('',*,*,#9793,.F.);
#12245=ORIENTED_EDGE('',*,*,#9792,.T.);
#12246=ORIENTED_EDGE('',*,*,#9795,.F.);
#12247=ORIENTED_EDGE('',*,*,#9796,.T.);
#12248=ORIENTED_EDGE('',*,*,#9797,.F.);
#12249=ORIENTED_EDGE('',*,*,#9796,.F.);
#12250=ORIENTED_EDGE('',*,*,#9795,.T.);
#12251=ORIENTED_EDGE('',*,*,#9798,.F.);
#12252=ORIENTED_EDGE('',*,*,#9799,.T.);
#12253=ORIENTED_EDGE('',*,*,#9800,.F.);
#12254=ORIENTED_EDGE('',*,*,#9799,.F.);
#12255=ORIENTED_EDGE('',*,*,#9798,.T.);
#12256=ORIENTED_EDGE('',*,*,#9801,.F.);
#12257=ORIENTED_EDGE('',*,*,#9802,.T.);
#12258=ORIENTED_EDGE('',*,*,#9803,.F.);
#12259=ORIENTED_EDGE('',*,*,#9802,.F.);
#12260=ORIENTED_EDGE('',*,*,#9801,.T.);
#12261=ORIENTED_EDGE('',*,*,#9804,.F.);
#12262=ORIENTED_EDGE('',*,*,#9805,.T.);
#12263=ORIENTED_EDGE('',*,*,#9806,.F.);
#12264=ORIENTED_EDGE('',*,*,#9805,.F.);
#12265=ORIENTED_EDGE('',*,*,#9807,.F.);
#12266=ORIENTED_EDGE('',*,*,#9808,.T.);
#12267=ORIENTED_EDGE('',*,*,#9809,.F.);
#12268=ORIENTED_EDGE('',*,*,#9808,.F.);
#12269=ORIENTED_EDGE('',*,*,#9810,.F.);
#12270=ORIENTED_EDGE('',*,*,#9811,.T.);
#12271=ORIENTED_EDGE('',*,*,#9812,.F.);
#12272=ORIENTED_EDGE('',*,*,#9811,.F.);
#12273=ORIENTED_EDGE('',*,*,#9813,.F.);
#12274=ORIENTED_EDGE('',*,*,#9814,.T.);
#12275=ORIENTED_EDGE('',*,*,#9815,.F.);
#12276=ORIENTED_EDGE('',*,*,#9814,.F.);
#12277=ORIENTED_EDGE('',*,*,#9816,.F.);
#12278=ORIENTED_EDGE('',*,*,#9817,.T.);
#12279=ORIENTED_EDGE('',*,*,#9818,.F.);
#12280=ORIENTED_EDGE('',*,*,#9817,.F.);
#12281=ORIENTED_EDGE('',*,*,#9819,.F.);
#12282=ORIENTED_EDGE('',*,*,#9820,.T.);
#12283=ORIENTED_EDGE('',*,*,#9821,.F.);
#12284=ORIENTED_EDGE('',*,*,#9820,.F.);
#12285=ORIENTED_EDGE('',*,*,#9822,.F.);
#12286=ORIENTED_EDGE('',*,*,#9823,.T.);
#12287=ORIENTED_EDGE('',*,*,#9824,.F.);
#12288=ORIENTED_EDGE('',*,*,#9823,.F.);
#12289=ORIENTED_EDGE('',*,*,#9825,.F.);
#12290=ORIENTED_EDGE('',*,*,#9826,.T.);
#12291=ORIENTED_EDGE('',*,*,#9827,.F.);
#12292=ORIENTED_EDGE('',*,*,#9826,.F.);
#12293=ORIENTED_EDGE('',*,*,#9828,.F.);
#12294=ORIENTED_EDGE('',*,*,#9829,.T.);
#12295=ORIENTED_EDGE('',*,*,#9830,.F.);
#12296=ORIENTED_EDGE('',*,*,#9829,.F.);
#12297=ORIENTED_EDGE('',*,*,#9831,.F.);
#12298=ORIENTED_EDGE('',*,*,#9832,.T.);
#12299=ORIENTED_EDGE('',*,*,#9833,.F.);
#12300=ORIENTED_EDGE('',*,*,#9832,.F.);
#12301=ORIENTED_EDGE('',*,*,#9834,.F.);
#12302=ORIENTED_EDGE('',*,*,#9835,.T.);
#12303=ORIENTED_EDGE('',*,*,#9836,.F.);
#12304=ORIENTED_EDGE('',*,*,#9835,.F.);
#12305=ORIENTED_EDGE('',*,*,#9837,.F.);
#12306=ORIENTED_EDGE('',*,*,#9838,.T.);
#12307=ORIENTED_EDGE('',*,*,#9839,.F.);
#12308=ORIENTED_EDGE('',*,*,#9838,.F.);
#12309=ORIENTED_EDGE('',*,*,#9840,.F.);
#12310=ORIENTED_EDGE('',*,*,#9841,.T.);
#12311=ORIENTED_EDGE('',*,*,#9842,.F.);
#12312=ORIENTED_EDGE('',*,*,#9841,.F.);
#12313=ORIENTED_EDGE('',*,*,#9843,.F.);
#12314=ORIENTED_EDGE('',*,*,#9844,.T.);
#12315=ORIENTED_EDGE('',*,*,#9845,.F.);
#12316=ORIENTED_EDGE('',*,*,#9844,.F.);
#12317=ORIENTED_EDGE('',*,*,#9846,.F.);
#12318=ORIENTED_EDGE('',*,*,#9847,.T.);
#12319=ORIENTED_EDGE('',*,*,#9848,.F.);
#12320=ORIENTED_EDGE('',*,*,#9847,.F.);
#12321=ORIENTED_EDGE('',*,*,#9849,.T.);
#12322=ORIENTED_EDGE('',*,*,#9850,.T.);
#12323=ORIENTED_EDGE('',*,*,#9851,.F.);
#12324=ORIENTED_EDGE('',*,*,#9787,.F.);
#12325=ORIENTED_EDGE('',*,*,#9852,.T.);
#12326=ORIENTED_EDGE('',*,*,#9790,.T.);
#12327=ORIENTED_EDGE('',*,*,#9853,.F.);
#12328=ORIENTED_EDGE('',*,*,#9854,.F.);
#12329=ORIENTED_EDGE('',*,*,#9855,.T.);
#12330=ORIENTED_EDGE('',*,*,#9854,.T.);
#12331=ORIENTED_EDGE('',*,*,#9856,.F.);
#12332=ORIENTED_EDGE('',*,*,#9850,.F.);
#12333=ORIENTED_EDGE('',*,*,#9788,.T.);
#12334=ORIENTED_EDGE('',*,*,#9851,.T.);
#12335=ORIENTED_EDGE('',*,*,#9856,.T.);
#12336=ORIENTED_EDGE('',*,*,#9853,.T.);
#12337=ORIENTED_EDGE('',*,*,#9789,.T.);
#12338=ORIENTED_EDGE('',*,*,#9785,.F.);
#12339=ORIENTED_EDGE('',*,*,#9782,.T.);
#12340=ORIENTED_EDGE('',*,*,#9777,.F.);
#12341=ORIENTED_EDGE('',*,*,#9806,.T.);
#12342=ORIENTED_EDGE('',*,*,#9812,.T.);
#12343=ORIENTED_EDGE('',*,*,#9815,.T.);
#12344=ORIENTED_EDGE('',*,*,#9818,.T.);
#12345=ORIENTED_EDGE('',*,*,#9821,.T.);
#12346=ORIENTED_EDGE('',*,*,#9827,.T.);
#12347=ORIENTED_EDGE('',*,*,#9830,.T.);
#12348=ORIENTED_EDGE('',*,*,#9833,.T.);
#12349=ORIENTED_EDGE('',*,*,#9836,.T.);
#12350=ORIENTED_EDGE('',*,*,#9839,.T.);
#12351=ORIENTED_EDGE('',*,*,#9842,.T.);
#12352=ORIENTED_EDGE('',*,*,#9845,.T.);
#12353=ORIENTED_EDGE('',*,*,#9848,.T.);
#12354=ORIENTED_EDGE('',*,*,#9824,.T.);
#12355=ORIENTED_EDGE('',*,*,#9809,.T.);
#12356=ORIENTED_EDGE('',*,*,#9803,.T.);
#12357=ORIENTED_EDGE('',*,*,#9800,.T.);
#12358=ORIENTED_EDGE('',*,*,#9797,.T.);
#12359=ORIENTED_EDGE('',*,*,#9794,.T.);
#12360=ORIENTED_EDGE('',*,*,#9775,.T.);
#12361=ORIENTED_EDGE('',*,*,#9791,.F.);
#12362=ORIENTED_EDGE('',*,*,#9852,.F.);
#12363=ORIENTED_EDGE('',*,*,#9855,.F.);
#12364=ORIENTED_EDGE('',*,*,#9849,.F.);
#12365=ORIENTED_EDGE('',*,*,#9786,.F.);
#12366=ORIENTED_EDGE('',*,*,#9779,.F.);
#12367=ORIENTED_EDGE('',*,*,#9781,.F.);
#12368=ORIENTED_EDGE('',*,*,#9784,.F.);
#12369=ORIENTED_EDGE('',*,*,#9807,.T.);
#12370=ORIENTED_EDGE('',*,*,#9822,.T.);
#12371=ORIENTED_EDGE('',*,*,#9846,.T.);
#12372=ORIENTED_EDGE('',*,*,#9843,.T.);
#12373=ORIENTED_EDGE('',*,*,#9840,.T.);
#12374=ORIENTED_EDGE('',*,*,#9837,.T.);
#12375=ORIENTED_EDGE('',*,*,#9834,.T.);
#12376=ORIENTED_EDGE('',*,*,#9831,.T.);
#12377=ORIENTED_EDGE('',*,*,#9828,.T.);
#12378=ORIENTED_EDGE('',*,*,#9825,.T.);
#12379=ORIENTED_EDGE('',*,*,#9819,.T.);
#12380=ORIENTED_EDGE('',*,*,#9816,.T.);
#12381=ORIENTED_EDGE('',*,*,#9813,.T.);
#12382=ORIENTED_EDGE('',*,*,#9810,.T.);
#12383=ORIENTED_EDGE('',*,*,#9804,.T.);
#12384=ORIENTED_EDGE('',*,*,#9773,.T.);
#12385=ORIENTED_EDGE('',*,*,#9857,.T.);
#12386=ORIENTED_EDGE('',*,*,#9858,.T.);
#12387=ORIENTED_EDGE('',*,*,#9859,.F.);
#12388=ORIENTED_EDGE('',*,*,#9860,.F.);
#12389=ORIENTED_EDGE('',*,*,#9861,.T.);
#12390=ORIENTED_EDGE('',*,*,#9860,.T.);
#12391=ORIENTED_EDGE('',*,*,#9862,.F.);
#12392=ORIENTED_EDGE('',*,*,#9863,.F.);
#12393=ORIENTED_EDGE('',*,*,#9864,.T.);
#12394=ORIENTED_EDGE('',*,*,#9863,.T.);
#12395=ORIENTED_EDGE('',*,*,#9865,.F.);
#12396=ORIENTED_EDGE('',*,*,#9866,.F.);
#12397=ORIENTED_EDGE('',*,*,#9867,.T.);
#12398=ORIENTED_EDGE('',*,*,#9866,.T.);
#12399=ORIENTED_EDGE('',*,*,#9868,.F.);
#12400=ORIENTED_EDGE('',*,*,#9858,.F.);
#12401=ORIENTED_EDGE('',*,*,#9868,.T.);
#12402=ORIENTED_EDGE('',*,*,#9865,.T.);
#12403=ORIENTED_EDGE('',*,*,#9862,.T.);
#12404=ORIENTED_EDGE('',*,*,#9859,.T.);
#12405=ORIENTED_EDGE('',*,*,#9867,.F.);
#12406=ORIENTED_EDGE('',*,*,#9857,.F.);
#12407=ORIENTED_EDGE('',*,*,#9861,.F.);
#12408=ORIENTED_EDGE('',*,*,#9864,.F.);
#12409=ORIENTED_EDGE('',*,*,#9869,.T.);
#12410=ORIENTED_EDGE('',*,*,#9870,.T.);
#12411=ORIENTED_EDGE('',*,*,#9871,.F.);
#12412=ORIENTED_EDGE('',*,*,#9872,.F.);
#12413=ORIENTED_EDGE('',*,*,#9873,.T.);
#12414=ORIENTED_EDGE('',*,*,#9872,.T.);
#12415=ORIENTED_EDGE('',*,*,#9874,.F.);
#12416=ORIENTED_EDGE('',*,*,#9875,.F.);
#12417=ORIENTED_EDGE('',*,*,#9876,.T.);
#12418=ORIENTED_EDGE('',*,*,#9875,.T.);
#12419=ORIENTED_EDGE('',*,*,#9877,.F.);
#12420=ORIENTED_EDGE('',*,*,#9878,.F.);
#12421=ORIENTED_EDGE('',*,*,#9879,.T.);
#12422=ORIENTED_EDGE('',*,*,#9878,.T.);
#12423=ORIENTED_EDGE('',*,*,#9880,.F.);
#12424=ORIENTED_EDGE('',*,*,#9870,.F.);
#12425=ORIENTED_EDGE('',*,*,#9880,.T.);
#12426=ORIENTED_EDGE('',*,*,#9877,.T.);
#12427=ORIENTED_EDGE('',*,*,#9874,.T.);
#12428=ORIENTED_EDGE('',*,*,#9871,.T.);
#12429=ORIENTED_EDGE('',*,*,#9879,.F.);
#12430=ORIENTED_EDGE('',*,*,#9869,.F.);
#12431=ORIENTED_EDGE('',*,*,#9873,.F.);
#12432=ORIENTED_EDGE('',*,*,#9876,.F.);
#12433=ORIENTED_EDGE('',*,*,#9881,.F.);
#12434=ORIENTED_EDGE('',*,*,#9882,.T.);
#12435=ORIENTED_EDGE('',*,*,#9883,.F.);
#12436=ORIENTED_EDGE('',*,*,#9882,.F.);
#12437=ORIENTED_EDGE('',*,*,#9884,.F.);
#12438=ORIENTED_EDGE('',*,*,#9885,.T.);
#12439=ORIENTED_EDGE('',*,*,#9886,.F.);
#12440=ORIENTED_EDGE('',*,*,#9885,.F.);
#12441=ORIENTED_EDGE('',*,*,#9887,.F.);
#12442=ORIENTED_EDGE('',*,*,#9888,.T.);
#12443=ORIENTED_EDGE('',*,*,#9889,.F.);
#12444=ORIENTED_EDGE('',*,*,#9888,.F.);
#12445=ORIENTED_EDGE('',*,*,#9890,.F.);
#12446=ORIENTED_EDGE('',*,*,#9891,.T.);
#12447=ORIENTED_EDGE('',*,*,#9892,.F.);
#12448=ORIENTED_EDGE('',*,*,#9891,.F.);
#12449=ORIENTED_EDGE('',*,*,#9893,.F.);
#12450=ORIENTED_EDGE('',*,*,#9894,.T.);
#12451=ORIENTED_EDGE('',*,*,#9895,.F.);
#12452=ORIENTED_EDGE('',*,*,#9894,.F.);
#12453=ORIENTED_EDGE('',*,*,#9896,.F.);
#12454=ORIENTED_EDGE('',*,*,#9897,.T.);
#12455=ORIENTED_EDGE('',*,*,#9898,.F.);
#12456=ORIENTED_EDGE('',*,*,#9897,.F.);
#12457=ORIENTED_EDGE('',*,*,#9899,.F.);
#12458=ORIENTED_EDGE('',*,*,#9900,.T.);
#12459=ORIENTED_EDGE('',*,*,#9901,.F.);
#12460=ORIENTED_EDGE('',*,*,#9900,.F.);
#12461=ORIENTED_EDGE('',*,*,#9902,.F.);
#12462=ORIENTED_EDGE('',*,*,#9903,.T.);
#12463=ORIENTED_EDGE('',*,*,#9904,.F.);
#12464=ORIENTED_EDGE('',*,*,#9903,.F.);
#12465=ORIENTED_EDGE('',*,*,#9905,.F.);
#12466=ORIENTED_EDGE('',*,*,#9906,.F.);
#12467=ORIENTED_EDGE('',*,*,#9907,.F.);
#12468=ORIENTED_EDGE('',*,*,#9908,.T.);
#12469=ORIENTED_EDGE('',*,*,#9909,.F.);
#12470=ORIENTED_EDGE('',*,*,#9908,.F.);
#12471=ORIENTED_EDGE('',*,*,#9910,.F.);
#12472=ORIENTED_EDGE('',*,*,#9911,.T.);
#12473=ORIENTED_EDGE('',*,*,#9912,.F.);
#12474=ORIENTED_EDGE('',*,*,#9911,.F.);
#12475=ORIENTED_EDGE('',*,*,#9913,.F.);
#12476=ORIENTED_EDGE('',*,*,#9914,.T.);
#12477=ORIENTED_EDGE('',*,*,#9915,.F.);
#12478=ORIENTED_EDGE('',*,*,#9914,.F.);
#12479=ORIENTED_EDGE('',*,*,#9916,.F.);
#12480=ORIENTED_EDGE('',*,*,#9906,.T.);
#12481=ORIENTED_EDGE('',*,*,#9917,.F.);
#12482=ORIENTED_EDGE('',*,*,#9918,.T.);
#12483=ORIENTED_EDGE('',*,*,#9919,.F.);
#12484=ORIENTED_EDGE('',*,*,#9918,.F.);
#12485=ORIENTED_EDGE('',*,*,#9920,.F.);
#12486=ORIENTED_EDGE('',*,*,#9921,.T.);
#12487=ORIENTED_EDGE('',*,*,#9922,.F.);
#12488=ORIENTED_EDGE('',*,*,#9921,.F.);
#12489=ORIENTED_EDGE('',*,*,#9923,.T.);
#12490=ORIENTED_EDGE('',*,*,#9924,.T.);
#12491=ORIENTED_EDGE('',*,*,#9925,.F.);
#12492=ORIENTED_EDGE('',*,*,#9926,.F.);
#12493=ORIENTED_EDGE('',*,*,#9927,.T.);
#12494=ORIENTED_EDGE('',*,*,#9926,.T.);
#12495=ORIENTED_EDGE('',*,*,#9928,.F.);
#12496=ORIENTED_EDGE('',*,*,#9929,.F.);
#12497=ORIENTED_EDGE('',*,*,#9930,.T.);
#12498=ORIENTED_EDGE('',*,*,#9929,.T.);
#12499=ORIENTED_EDGE('',*,*,#9931,.F.);
#12500=ORIENTED_EDGE('',*,*,#9932,.F.);
#12501=ORIENTED_EDGE('',*,*,#9933,.T.);
#12502=ORIENTED_EDGE('',*,*,#9932,.T.);
#12503=ORIENTED_EDGE('',*,*,#9934,.F.);
#12504=ORIENTED_EDGE('',*,*,#9924,.F.);
#12505=ORIENTED_EDGE('',*,*,#9934,.T.);
#12506=ORIENTED_EDGE('',*,*,#9931,.T.);
#12507=ORIENTED_EDGE('',*,*,#9928,.T.);
#12508=ORIENTED_EDGE('',*,*,#9925,.T.);
#12509=ORIENTED_EDGE('',*,*,#9889,.T.);
#12510=ORIENTED_EDGE('',*,*,#9892,.T.);
#12511=ORIENTED_EDGE('',*,*,#9922,.T.);
#12512=ORIENTED_EDGE('',*,*,#9919,.T.);
#12513=ORIENTED_EDGE('',*,*,#9912,.T.);
#12514=ORIENTED_EDGE('',*,*,#9915,.T.);
#12515=ORIENTED_EDGE('',*,*,#9905,.T.);
#12516=ORIENTED_EDGE('',*,*,#9909,.T.);
#12517=ORIENTED_EDGE('',*,*,#9904,.T.);
#12518=ORIENTED_EDGE('',*,*,#9901,.T.);
#12519=ORIENTED_EDGE('',*,*,#9898,.T.);
#12520=ORIENTED_EDGE('',*,*,#9895,.T.);
#12521=ORIENTED_EDGE('',*,*,#9886,.T.);
#12522=ORIENTED_EDGE('',*,*,#9883,.T.);
#12523=ORIENTED_EDGE('',*,*,#9933,.F.);
#12524=ORIENTED_EDGE('',*,*,#9923,.F.);
#12525=ORIENTED_EDGE('',*,*,#9927,.F.);
#12526=ORIENTED_EDGE('',*,*,#9930,.F.);
#12527=ORIENTED_EDGE('',*,*,#9887,.T.);
#12528=ORIENTED_EDGE('',*,*,#9890,.T.);
#12529=ORIENTED_EDGE('',*,*,#9920,.T.);
#12530=ORIENTED_EDGE('',*,*,#9917,.T.);
#12531=ORIENTED_EDGE('',*,*,#9913,.T.);
#12532=ORIENTED_EDGE('',*,*,#9910,.T.);
#12533=ORIENTED_EDGE('',*,*,#9907,.T.);
#12534=ORIENTED_EDGE('',*,*,#9916,.T.);
#12535=ORIENTED_EDGE('',*,*,#9902,.T.);
#12536=ORIENTED_EDGE('',*,*,#9899,.T.);
#12537=ORIENTED_EDGE('',*,*,#9896,.T.);
#12538=ORIENTED_EDGE('',*,*,#9893,.T.);
#12539=ORIENTED_EDGE('',*,*,#9884,.T.);
#12540=ORIENTED_EDGE('',*,*,#9881,.T.);
#12541=ORIENTED_EDGE('',*,*,#9935,.F.);
#12542=ORIENTED_EDGE('',*,*,#9936,.T.);
#12543=ORIENTED_EDGE('',*,*,#9937,.F.);
#12544=ORIENTED_EDGE('',*,*,#9936,.F.);
#12545=ORIENTED_EDGE('',*,*,#9938,.F.);
#12546=ORIENTED_EDGE('',*,*,#9939,.T.);
#12547=ORIENTED_EDGE('',*,*,#9940,.F.);
#12548=ORIENTED_EDGE('',*,*,#9939,.F.);
#12549=ORIENTED_EDGE('',*,*,#9941,.F.);
#12550=ORIENTED_EDGE('',*,*,#9942,.T.);
#12551=ORIENTED_EDGE('',*,*,#9943,.F.);
#12552=ORIENTED_EDGE('',*,*,#9942,.F.);
#12553=ORIENTED_EDGE('',*,*,#9941,.T.);
#12554=ORIENTED_EDGE('',*,*,#9944,.F.);
#12555=ORIENTED_EDGE('',*,*,#9945,.T.);
#12556=ORIENTED_EDGE('',*,*,#9946,.F.);
#12557=ORIENTED_EDGE('',*,*,#9945,.F.);
#12558=ORIENTED_EDGE('',*,*,#9944,.T.);
#12559=ORIENTED_EDGE('',*,*,#9947,.F.);
#12560=ORIENTED_EDGE('',*,*,#9948,.T.);
#12561=ORIENTED_EDGE('',*,*,#9949,.T.);
#12562=ORIENTED_EDGE('',*,*,#9948,.F.);
#12563=ORIENTED_EDGE('',*,*,#9949,.F.);
#12564=ORIENTED_EDGE('',*,*,#9950,.F.);
#12565=ORIENTED_EDGE('',*,*,#9951,.T.);
#12566=ORIENTED_EDGE('',*,*,#9952,.T.);
#12567=ORIENTED_EDGE('',*,*,#9951,.F.);
#12568=ORIENTED_EDGE('',*,*,#9952,.F.);
#12569=ORIENTED_EDGE('',*,*,#9953,.T.);
#12570=ORIENTED_EDGE('',*,*,#9954,.T.);
#12571=ORIENTED_EDGE('',*,*,#9955,.F.);
#12572=ORIENTED_EDGE('',*,*,#9956,.F.);
#12573=ORIENTED_EDGE('',*,*,#9957,.T.);
#12574=ORIENTED_EDGE('',*,*,#9956,.T.);
#12575=ORIENTED_EDGE('',*,*,#9958,.F.);
#12576=ORIENTED_EDGE('',*,*,#9959,.F.);
#12577=ORIENTED_EDGE('',*,*,#9937,.T.);
#12578=ORIENTED_EDGE('',*,*,#9940,.T.);
#12579=ORIENTED_EDGE('',*,*,#9960,.T.);
#12580=ORIENTED_EDGE('',*,*,#9959,.T.);
#12581=ORIENTED_EDGE('',*,*,#9961,.F.);
#12582=ORIENTED_EDGE('',*,*,#9962,.F.);
#12583=ORIENTED_EDGE('',*,*,#9963,.T.);
#12584=ORIENTED_EDGE('',*,*,#9962,.T.);
#12585=ORIENTED_EDGE('',*,*,#9964,.F.);
#12586=ORIENTED_EDGE('',*,*,#9954,.F.);
#12587=ORIENTED_EDGE('',*,*,#9935,.T.);
#12588=ORIENTED_EDGE('',*,*,#9938,.T.);
#12589=ORIENTED_EDGE('',*,*,#9964,.T.);
#12590=ORIENTED_EDGE('',*,*,#9961,.T.);
#12591=ORIENTED_EDGE('',*,*,#9958,.T.);
#12592=ORIENTED_EDGE('',*,*,#9955,.T.);
#12593=ORIENTED_EDGE('',*,*,#9943,.T.);
#12594=ORIENTED_EDGE('',*,*,#9946,.T.);
#12595=ORIENTED_EDGE('',*,*,#9963,.F.);
#12596=ORIENTED_EDGE('',*,*,#9953,.F.);
#12597=ORIENTED_EDGE('',*,*,#9957,.F.);
#12598=ORIENTED_EDGE('',*,*,#9960,.F.);
#12599=ORIENTED_EDGE('',*,*,#9947,.T.);
#12600=ORIENTED_EDGE('',*,*,#9950,.T.);
#12601=ORIENTED_EDGE('',*,*,#9965,.F.);
#12602=ORIENTED_EDGE('',*,*,#9966,.T.);
#12603=ORIENTED_EDGE('',*,*,#9967,.F.);
#12604=ORIENTED_EDGE('',*,*,#9966,.F.);
#12605=ORIENTED_EDGE('',*,*,#9968,.F.);
#12606=ORIENTED_EDGE('',*,*,#9969,.T.);
#12607=ORIENTED_EDGE('',*,*,#9970,.F.);
#12608=ORIENTED_EDGE('',*,*,#9969,.F.);
#12609=ORIENTED_EDGE('',*,*,#9971,.F.);
#12610=ORIENTED_EDGE('',*,*,#9972,.T.);
#12611=ORIENTED_EDGE('',*,*,#9973,.F.);
#12612=ORIENTED_EDGE('',*,*,#9972,.F.);
#12613=ORIENTED_EDGE('',*,*,#9971,.T.);
#12614=ORIENTED_EDGE('',*,*,#9974,.F.);
#12615=ORIENTED_EDGE('',*,*,#9975,.T.);
#12616=ORIENTED_EDGE('',*,*,#9976,.F.);
#12617=ORIENTED_EDGE('',*,*,#9975,.F.);
#12618=ORIENTED_EDGE('',*,*,#9974,.T.);
#12619=ORIENTED_EDGE('',*,*,#9977,.F.);
#12620=ORIENTED_EDGE('',*,*,#9978,.T.);
#12621=ORIENTED_EDGE('',*,*,#9979,.T.);
#12622=ORIENTED_EDGE('',*,*,#9978,.F.);
#12623=ORIENTED_EDGE('',*,*,#9979,.F.);
#12624=ORIENTED_EDGE('',*,*,#9980,.F.);
#12625=ORIENTED_EDGE('',*,*,#9981,.T.);
#12626=ORIENTED_EDGE('',*,*,#9982,.T.);
#12627=ORIENTED_EDGE('',*,*,#9981,.F.);
#12628=ORIENTED_EDGE('',*,*,#9982,.F.);
#12629=ORIENTED_EDGE('',*,*,#9983,.T.);
#12630=ORIENTED_EDGE('',*,*,#9984,.T.);
#12631=ORIENTED_EDGE('',*,*,#9985,.F.);
#12632=ORIENTED_EDGE('',*,*,#9986,.F.);
#12633=ORIENTED_EDGE('',*,*,#9987,.T.);
#12634=ORIENTED_EDGE('',*,*,#9986,.T.);
#12635=ORIENTED_EDGE('',*,*,#9988,.F.);
#12636=ORIENTED_EDGE('',*,*,#9989,.F.);
#12637=ORIENTED_EDGE('',*,*,#9967,.T.);
#12638=ORIENTED_EDGE('',*,*,#9970,.T.);
#12639=ORIENTED_EDGE('',*,*,#9990,.T.);
#12640=ORIENTED_EDGE('',*,*,#9989,.T.);
#12641=ORIENTED_EDGE('',*,*,#9991,.F.);
#12642=ORIENTED_EDGE('',*,*,#9992,.F.);
#12643=ORIENTED_EDGE('',*,*,#9993,.T.);
#12644=ORIENTED_EDGE('',*,*,#9992,.T.);
#12645=ORIENTED_EDGE('',*,*,#9994,.F.);
#12646=ORIENTED_EDGE('',*,*,#9984,.F.);
#12647=ORIENTED_EDGE('',*,*,#9965,.T.);
#12648=ORIENTED_EDGE('',*,*,#9968,.T.);
#12649=ORIENTED_EDGE('',*,*,#9994,.T.);
#12650=ORIENTED_EDGE('',*,*,#9991,.T.);
#12651=ORIENTED_EDGE('',*,*,#9988,.T.);
#12652=ORIENTED_EDGE('',*,*,#9985,.T.);
#12653=ORIENTED_EDGE('',*,*,#9973,.T.);
#12654=ORIENTED_EDGE('',*,*,#9976,.T.);
#12655=ORIENTED_EDGE('',*,*,#9993,.F.);
#12656=ORIENTED_EDGE('',*,*,#9983,.F.);
#12657=ORIENTED_EDGE('',*,*,#9987,.F.);
#12658=ORIENTED_EDGE('',*,*,#9990,.F.);
#12659=ORIENTED_EDGE('',*,*,#9977,.T.);
#12660=ORIENTED_EDGE('',*,*,#9980,.T.);
#12661=ORIENTED_EDGE('',*,*,#9995,.F.);
#12662=ORIENTED_EDGE('',*,*,#9996,.T.);
#12663=ORIENTED_EDGE('',*,*,#9997,.T.);
#12664=ORIENTED_EDGE('',*,*,#9996,.F.);
#12665=ORIENTED_EDGE('',*,*,#9997,.F.);
#12666=ORIENTED_EDGE('',*,*,#9998,.F.);
#12667=ORIENTED_EDGE('',*,*,#9999,.T.);
#12668=ORIENTED_EDGE('',*,*,#10000,.T.);
#12669=ORIENTED_EDGE('',*,*,#9999,.F.);
#12670=ORIENTED_EDGE('',*,*,#10000,.F.);
#12671=ORIENTED_EDGE('',*,*,#10001,.F.);
#12672=ORIENTED_EDGE('',*,*,#10002,.T.);
#12673=ORIENTED_EDGE('',*,*,#10003,.F.);
#12674=ORIENTED_EDGE('',*,*,#10002,.F.);
#12675=ORIENTED_EDGE('',*,*,#10004,.F.);
#12676=ORIENTED_EDGE('',*,*,#10005,.T.);
#12677=ORIENTED_EDGE('',*,*,#10006,.F.);
#12678=ORIENTED_EDGE('',*,*,#10005,.F.);
#12679=ORIENTED_EDGE('',*,*,#10007,.T.);
#12680=ORIENTED_EDGE('',*,*,#10008,.T.);
#12681=ORIENTED_EDGE('',*,*,#10009,.F.);
#12682=ORIENTED_EDGE('',*,*,#10010,.F.);
#12683=ORIENTED_EDGE('',*,*,#10003,.T.);
#12684=ORIENTED_EDGE('',*,*,#10006,.T.);
#12685=ORIENTED_EDGE('',*,*,#10011,.T.);
#12686=ORIENTED_EDGE('',*,*,#10010,.T.);
#12687=ORIENTED_EDGE('',*,*,#10012,.F.);
#12688=ORIENTED_EDGE('',*,*,#10013,.F.);
#12689=ORIENTED_EDGE('',*,*,#10014,.T.);
#12690=ORIENTED_EDGE('',*,*,#10013,.T.);
#12691=ORIENTED_EDGE('',*,*,#10015,.F.);
#12692=ORIENTED_EDGE('',*,*,#10016,.F.);
#12693=ORIENTED_EDGE('',*,*,#10001,.T.);
#12694=ORIENTED_EDGE('',*,*,#10004,.T.);
#12695=ORIENTED_EDGE('',*,*,#10017,.T.);
#12696=ORIENTED_EDGE('',*,*,#10016,.T.);
#12697=ORIENTED_EDGE('',*,*,#10018,.F.);
#12698=ORIENTED_EDGE('',*,*,#10008,.F.);
#12699=ORIENTED_EDGE('',*,*,#10018,.T.);
#12700=ORIENTED_EDGE('',*,*,#10015,.T.);
#12701=ORIENTED_EDGE('',*,*,#10012,.T.);
#12702=ORIENTED_EDGE('',*,*,#10009,.T.);
#12703=ORIENTED_EDGE('',*,*,#10017,.F.);
#12704=ORIENTED_EDGE('',*,*,#10007,.F.);
#12705=ORIENTED_EDGE('',*,*,#10011,.F.);
#12706=ORIENTED_EDGE('',*,*,#10014,.F.);
#12707=ORIENTED_EDGE('',*,*,#9995,.T.);
#12708=ORIENTED_EDGE('',*,*,#9998,.T.);
#12709=ORIENTED_EDGE('',*,*,#10019,.F.);
#12710=ORIENTED_EDGE('',*,*,#10020,.T.);
#12711=ORIENTED_EDGE('',*,*,#10021,.F.);
#12712=ORIENTED_EDGE('',*,*,#10020,.F.);
#12713=ORIENTED_EDGE('',*,*,#10022,.F.);
#12714=ORIENTED_EDGE('',*,*,#10023,.T.);
#12715=ORIENTED_EDGE('',*,*,#10024,.F.);
#12716=ORIENTED_EDGE('',*,*,#10023,.F.);
#12717=ORIENTED_EDGE('',*,*,#10025,.F.);
#12718=ORIENTED_EDGE('',*,*,#10026,.T.);
#12719=ORIENTED_EDGE('',*,*,#10027,.T.);
#12720=ORIENTED_EDGE('',*,*,#10028,.F.);
#12721=ORIENTED_EDGE('',*,*,#10029,.F.);
#12722=ORIENTED_EDGE('',*,*,#10030,.F.);
#12723=ORIENTED_EDGE('',*,*,#10031,.T.);
#12724=ORIENTED_EDGE('',*,*,#10026,.F.);
#12725=ORIENTED_EDGE('',*,*,#10032,.F.);
#12726=ORIENTED_EDGE('',*,*,#10027,.F.);
#12727=ORIENTED_EDGE('',*,*,#10031,.F.);
#12728=ORIENTED_EDGE('',*,*,#10033,.F.);
#12729=ORIENTED_EDGE('',*,*,#10034,.T.);
#12730=ORIENTED_EDGE('',*,*,#10035,.T.);
#12731=ORIENTED_EDGE('',*,*,#10036,.F.);
#12732=ORIENTED_EDGE('',*,*,#10037,.F.);
#12733=ORIENTED_EDGE('',*,*,#10038,.F.);
#12734=ORIENTED_EDGE('',*,*,#10039,.T.);
#12735=ORIENTED_EDGE('',*,*,#10034,.F.);
#12736=ORIENTED_EDGE('',*,*,#10040,.F.);
#12737=ORIENTED_EDGE('',*,*,#10035,.F.);
#12738=ORIENTED_EDGE('',*,*,#10039,.F.);
#12739=ORIENTED_EDGE('',*,*,#10029,.T.);
#12740=ORIENTED_EDGE('',*,*,#10041,.T.);
#12741=ORIENTED_EDGE('',*,*,#10037,.T.);
#12742=ORIENTED_EDGE('',*,*,#10042,.T.);
#12743=ORIENTED_EDGE('',*,*,#10043,.F.);
#12744=ORIENTED_EDGE('',*,*,#10044,.T.);
#12745=ORIENTED_EDGE('',*,*,#10045,.T.);
#12746=ORIENTED_EDGE('',*,*,#10046,.T.);
#12747=ORIENTED_EDGE('',*,*,#10030,.T.);
#12748=ORIENTED_EDGE('',*,*,#10046,.F.);
#12749=ORIENTED_EDGE('',*,*,#10047,.T.);
#12750=ORIENTED_EDGE('',*,*,#10048,.F.);
#12751=ORIENTED_EDGE('',*,*,#10049,.F.);
#12752=ORIENTED_EDGE('',*,*,#10042,.F.);
#12753=ORIENTED_EDGE('',*,*,#10036,.T.);
#12754=ORIENTED_EDGE('',*,*,#10040,.T.);
#12755=ORIENTED_EDGE('',*,*,#10038,.T.);
#12756=ORIENTED_EDGE('',*,*,#10041,.F.);
#12757=ORIENTED_EDGE('',*,*,#10028,.T.);
#12758=ORIENTED_EDGE('',*,*,#10032,.T.);
#12759=ORIENTED_EDGE('',*,*,#10019,.T.);
#12760=ORIENTED_EDGE('',*,*,#10022,.T.);
#12761=ORIENTED_EDGE('',*,*,#10050,.T.);
#12762=ORIENTED_EDGE('',*,*,#10051,.T.);
#12763=ORIENTED_EDGE('',*,*,#10048,.T.);
#12764=ORIENTED_EDGE('',*,*,#10052,.T.);
#12765=ORIENTED_EDGE('',*,*,#10053,.F.);
#12766=ORIENTED_EDGE('',*,*,#10054,.T.);
#12767=ORIENTED_EDGE('',*,*,#10043,.T.);
#12768=ORIENTED_EDGE('',*,*,#10049,.T.);
#12769=ORIENTED_EDGE('',*,*,#10051,.F.);
#12770=ORIENTED_EDGE('',*,*,#10055,.F.);
#12771=ORIENTED_EDGE('',*,*,#10056,.F.);
#12772=ORIENTED_EDGE('',*,*,#10057,.T.);
#12773=ORIENTED_EDGE('',*,*,#10053,.T.);
#12774=ORIENTED_EDGE('',*,*,#10058,.F.);
#12775=ORIENTED_EDGE('',*,*,#10025,.T.);
#12776=ORIENTED_EDGE('',*,*,#10033,.T.);
#12777=ORIENTED_EDGE('',*,*,#10045,.F.);
#12778=ORIENTED_EDGE('',*,*,#10059,.T.);
#12779=ORIENTED_EDGE('',*,*,#10056,.T.);
#12780=ORIENTED_EDGE('',*,*,#10060,.T.);
#12781=ORIENTED_EDGE('',*,*,#10052,.F.);
#12782=ORIENTED_EDGE('',*,*,#10047,.F.);
#12783=ORIENTED_EDGE('',*,*,#10060,.F.);
#12784=ORIENTED_EDGE('',*,*,#10058,.T.);
#12785=ORIENTED_EDGE('',*,*,#10055,.T.);
#12786=ORIENTED_EDGE('',*,*,#10050,.F.);
#12787=ORIENTED_EDGE('',*,*,#10021,.T.);
#12788=ORIENTED_EDGE('',*,*,#10024,.T.);
#12789=ORIENTED_EDGE('',*,*,#10059,.F.);
#12790=ORIENTED_EDGE('',*,*,#10044,.F.);
#12791=ORIENTED_EDGE('',*,*,#10054,.F.);
#12792=ORIENTED_EDGE('',*,*,#10057,.F.);
#12793=ORIENTED_EDGE('',*,*,#10061,.F.);
#12794=ORIENTED_EDGE('',*,*,#10062,.T.);
#12795=ORIENTED_EDGE('',*,*,#10063,.T.);
#12796=ORIENTED_EDGE('',*,*,#10062,.F.);
#12797=ORIENTED_EDGE('',*,*,#10063,.F.);
#12798=ORIENTED_EDGE('',*,*,#10064,.F.);
#12799=ORIENTED_EDGE('',*,*,#10065,.T.);
#12800=ORIENTED_EDGE('',*,*,#10066,.T.);
#12801=ORIENTED_EDGE('',*,*,#10065,.F.);
#12802=ORIENTED_EDGE('',*,*,#10066,.F.);
#12803=ORIENTED_EDGE('',*,*,#10067,.F.);
#12804=ORIENTED_EDGE('',*,*,#10068,.T.);
#12805=ORIENTED_EDGE('',*,*,#10069,.F.);
#12806=ORIENTED_EDGE('',*,*,#10068,.F.);
#12807=ORIENTED_EDGE('',*,*,#10070,.F.);
#12808=ORIENTED_EDGE('',*,*,#10071,.T.);
#12809=ORIENTED_EDGE('',*,*,#10072,.F.);
#12810=ORIENTED_EDGE('',*,*,#10071,.F.);
#12811=ORIENTED_EDGE('',*,*,#10073,.T.);
#12812=ORIENTED_EDGE('',*,*,#10074,.T.);
#12813=ORIENTED_EDGE('',*,*,#10075,.F.);
#12814=ORIENTED_EDGE('',*,*,#10076,.F.);
#12815=ORIENTED_EDGE('',*,*,#10069,.T.);
#12816=ORIENTED_EDGE('',*,*,#10072,.T.);
#12817=ORIENTED_EDGE('',*,*,#10077,.T.);
#12818=ORIENTED_EDGE('',*,*,#10076,.T.);
#12819=ORIENTED_EDGE('',*,*,#10078,.F.);
#12820=ORIENTED_EDGE('',*,*,#10079,.F.);
#12821=ORIENTED_EDGE('',*,*,#10080,.T.);
#12822=ORIENTED_EDGE('',*,*,#10079,.T.);
#12823=ORIENTED_EDGE('',*,*,#10081,.F.);
#12824=ORIENTED_EDGE('',*,*,#10082,.F.);
#12825=ORIENTED_EDGE('',*,*,#10067,.T.);
#12826=ORIENTED_EDGE('',*,*,#10070,.T.);
#12827=ORIENTED_EDGE('',*,*,#10083,.T.);
#12828=ORIENTED_EDGE('',*,*,#10082,.T.);
#12829=ORIENTED_EDGE('',*,*,#10084,.F.);
#12830=ORIENTED_EDGE('',*,*,#10074,.F.);
#12831=ORIENTED_EDGE('',*,*,#10084,.T.);
#12832=ORIENTED_EDGE('',*,*,#10081,.T.);
#12833=ORIENTED_EDGE('',*,*,#10078,.T.);
#12834=ORIENTED_EDGE('',*,*,#10075,.T.);
#12835=ORIENTED_EDGE('',*,*,#10083,.F.);
#12836=ORIENTED_EDGE('',*,*,#10073,.F.);
#12837=ORIENTED_EDGE('',*,*,#10077,.F.);
#12838=ORIENTED_EDGE('',*,*,#10080,.F.);
#12839=ORIENTED_EDGE('',*,*,#10061,.T.);
#12840=ORIENTED_EDGE('',*,*,#10064,.T.);
#12841=ORIENTED_EDGE('',*,*,#10085,.F.);
#12842=ORIENTED_EDGE('',*,*,#10086,.T.);
#12843=ORIENTED_EDGE('',*,*,#10087,.F.);
#12844=ORIENTED_EDGE('',*,*,#10086,.F.);
#12845=ORIENTED_EDGE('',*,*,#10088,.F.);
#12846=ORIENTED_EDGE('',*,*,#10089,.T.);
#12847=ORIENTED_EDGE('',*,*,#10090,.F.);
#12848=ORIENTED_EDGE('',*,*,#10089,.F.);
#12849=ORIENTED_EDGE('',*,*,#10091,.F.);
#12850=ORIENTED_EDGE('',*,*,#10092,.T.);
#12851=ORIENTED_EDGE('',*,*,#10093,.T.);
#12852=ORIENTED_EDGE('',*,*,#10094,.F.);
#12853=ORIENTED_EDGE('',*,*,#10095,.F.);
#12854=ORIENTED_EDGE('',*,*,#10096,.F.);
#12855=ORIENTED_EDGE('',*,*,#10097,.T.);
#12856=ORIENTED_EDGE('',*,*,#10092,.F.);
#12857=ORIENTED_EDGE('',*,*,#10098,.F.);
#12858=ORIENTED_EDGE('',*,*,#10093,.F.);
#12859=ORIENTED_EDGE('',*,*,#10097,.F.);
#12860=ORIENTED_EDGE('',*,*,#10099,.F.);
#12861=ORIENTED_EDGE('',*,*,#10100,.T.);
#12862=ORIENTED_EDGE('',*,*,#10101,.T.);
#12863=ORIENTED_EDGE('',*,*,#10102,.F.);
#12864=ORIENTED_EDGE('',*,*,#10103,.F.);
#12865=ORIENTED_EDGE('',*,*,#10104,.F.);
#12866=ORIENTED_EDGE('',*,*,#10105,.T.);
#12867=ORIENTED_EDGE('',*,*,#10100,.F.);
#12868=ORIENTED_EDGE('',*,*,#10106,.F.);
#12869=ORIENTED_EDGE('',*,*,#10101,.F.);
#12870=ORIENTED_EDGE('',*,*,#10105,.F.);
#12871=ORIENTED_EDGE('',*,*,#10095,.T.);
#12872=ORIENTED_EDGE('',*,*,#10107,.T.);
#12873=ORIENTED_EDGE('',*,*,#10103,.T.);
#12874=ORIENTED_EDGE('',*,*,#10108,.T.);
#12875=ORIENTED_EDGE('',*,*,#10109,.F.);
#12876=ORIENTED_EDGE('',*,*,#10110,.T.);
#12877=ORIENTED_EDGE('',*,*,#10111,.T.);
#12878=ORIENTED_EDGE('',*,*,#10112,.T.);
#12879=ORIENTED_EDGE('',*,*,#10096,.T.);
#12880=ORIENTED_EDGE('',*,*,#10112,.F.);
#12881=ORIENTED_EDGE('',*,*,#10113,.T.);
#12882=ORIENTED_EDGE('',*,*,#10114,.F.);
#12883=ORIENTED_EDGE('',*,*,#10115,.F.);
#12884=ORIENTED_EDGE('',*,*,#10108,.F.);
#12885=ORIENTED_EDGE('',*,*,#10102,.T.);
#12886=ORIENTED_EDGE('',*,*,#10106,.T.);
#12887=ORIENTED_EDGE('',*,*,#10104,.T.);
#12888=ORIENTED_EDGE('',*,*,#10107,.F.);
#12889=ORIENTED_EDGE('',*,*,#10094,.T.);
#12890=ORIENTED_EDGE('',*,*,#10098,.T.);
#12891=ORIENTED_EDGE('',*,*,#10085,.T.);
#12892=ORIENTED_EDGE('',*,*,#10088,.T.);
#12893=ORIENTED_EDGE('',*,*,#10116,.T.);
#12894=ORIENTED_EDGE('',*,*,#10117,.T.);
#12895=ORIENTED_EDGE('',*,*,#10114,.T.);
#12896=ORIENTED_EDGE('',*,*,#10118,.T.);
#12897=ORIENTED_EDGE('',*,*,#10119,.F.);
#12898=ORIENTED_EDGE('',*,*,#10120,.T.);
#12899=ORIENTED_EDGE('',*,*,#10109,.T.);
#12900=ORIENTED_EDGE('',*,*,#10115,.T.);
#12901=ORIENTED_EDGE('',*,*,#10117,.F.);
#12902=ORIENTED_EDGE('',*,*,#10121,.F.);
#12903=ORIENTED_EDGE('',*,*,#10122,.F.);
#12904=ORIENTED_EDGE('',*,*,#10123,.T.);
#12905=ORIENTED_EDGE('',*,*,#10119,.T.);
#12906=ORIENTED_EDGE('',*,*,#10124,.F.);
#12907=ORIENTED_EDGE('',*,*,#10091,.T.);
#12908=ORIENTED_EDGE('',*,*,#10099,.T.);
#12909=ORIENTED_EDGE('',*,*,#10111,.F.);
#12910=ORIENTED_EDGE('',*,*,#10125,.T.);
#12911=ORIENTED_EDGE('',*,*,#10122,.T.);
#12912=ORIENTED_EDGE('',*,*,#10126,.T.);
#12913=ORIENTED_EDGE('',*,*,#10118,.F.);
#12914=ORIENTED_EDGE('',*,*,#10113,.F.);
#12915=ORIENTED_EDGE('',*,*,#10126,.F.);
#12916=ORIENTED_EDGE('',*,*,#10124,.T.);
#12917=ORIENTED_EDGE('',*,*,#10121,.T.);
#12918=ORIENTED_EDGE('',*,*,#10116,.F.);
#12919=ORIENTED_EDGE('',*,*,#10087,.T.);
#12920=ORIENTED_EDGE('',*,*,#10090,.T.);
#12921=ORIENTED_EDGE('',*,*,#10125,.F.);
#12922=ORIENTED_EDGE('',*,*,#10110,.F.);
#12923=ORIENTED_EDGE('',*,*,#10120,.F.);
#12924=ORIENTED_EDGE('',*,*,#10123,.F.);
#12925=ORIENTED_EDGE('',*,*,#10127,.F.);
#12926=ORIENTED_EDGE('',*,*,#10128,.T.);
#12927=ORIENTED_EDGE('',*,*,#10129,.F.);
#12928=ORIENTED_EDGE('',*,*,#10128,.F.);
#12929=ORIENTED_EDGE('',*,*,#10130,.F.);
#12930=ORIENTED_EDGE('',*,*,#10131,.T.);
#12931=ORIENTED_EDGE('',*,*,#10132,.F.);
#12932=ORIENTED_EDGE('',*,*,#10131,.F.);
#12933=ORIENTED_EDGE('',*,*,#10133,.F.);
#12934=ORIENTED_EDGE('',*,*,#10134,.T.);
#12935=ORIENTED_EDGE('',*,*,#10135,.F.);
#12936=ORIENTED_EDGE('',*,*,#10134,.F.);
#12937=ORIENTED_EDGE('',*,*,#10136,.F.);
#12938=ORIENTED_EDGE('',*,*,#10137,.T.);
#12939=ORIENTED_EDGE('',*,*,#10138,.T.);
#12940=ORIENTED_EDGE('',*,*,#10137,.F.);
#12941=ORIENTED_EDGE('',*,*,#10138,.F.);
#12942=ORIENTED_EDGE('',*,*,#10139,.F.);
#12943=ORIENTED_EDGE('',*,*,#10140,.T.);
#12944=ORIENTED_EDGE('',*,*,#10141,.T.);
#12945=ORIENTED_EDGE('',*,*,#10140,.F.);
#12946=ORIENTED_EDGE('',*,*,#10141,.F.);
#12947=ORIENTED_EDGE('',*,*,#10142,.F.);
#12948=ORIENTED_EDGE('',*,*,#10143,.T.);
#12949=ORIENTED_EDGE('',*,*,#10144,.T.);
#12950=ORIENTED_EDGE('',*,*,#10143,.F.);
#12951=ORIENTED_EDGE('',*,*,#10144,.F.);
#12952=ORIENTED_EDGE('',*,*,#10145,.F.);
#12953=ORIENTED_EDGE('',*,*,#10146,.T.);
#12954=ORIENTED_EDGE('',*,*,#10147,.T.);
#12955=ORIENTED_EDGE('',*,*,#10146,.F.);
#12956=ORIENTED_EDGE('',*,*,#10147,.F.);
#12957=ORIENTED_EDGE('',*,*,#10148,.F.);
#12958=ORIENTED_EDGE('',*,*,#10149,.T.);
#12959=ORIENTED_EDGE('',*,*,#10150,.T.);
#12960=ORIENTED_EDGE('',*,*,#10149,.F.);
#12961=ORIENTED_EDGE('',*,*,#10150,.F.);
#12962=ORIENTED_EDGE('',*,*,#10151,.F.);
#12963=ORIENTED_EDGE('',*,*,#10151,.T.);
#12964=ORIENTED_EDGE('',*,*,#10152,.T.);
#12965=ORIENTED_EDGE('',*,*,#10153,.F.);
#12966=ORIENTED_EDGE('',*,*,#10152,.F.);
#12967=ORIENTED_EDGE('',*,*,#10154,.F.);
#12968=ORIENTED_EDGE('',*,*,#10155,.T.);
#12969=ORIENTED_EDGE('',*,*,#10156,.T.);
#12970=ORIENTED_EDGE('',*,*,#10155,.F.);
#12971=ORIENTED_EDGE('',*,*,#10156,.F.);
#12972=ORIENTED_EDGE('',*,*,#10127,.T.);
#12973=ORIENTED_EDGE('',*,*,#10130,.T.);
#12974=ORIENTED_EDGE('',*,*,#10133,.T.);
#12975=ORIENTED_EDGE('',*,*,#10148,.T.);
#12976=ORIENTED_EDGE('',*,*,#10157,.T.);
#12977=ORIENTED_EDGE('',*,*,#10158,.T.);
#12978=ORIENTED_EDGE('',*,*,#10159,.F.);
#12979=ORIENTED_EDGE('',*,*,#10160,.F.);
#12980=ORIENTED_EDGE('',*,*,#10161,.T.);
#12981=ORIENTED_EDGE('',*,*,#10160,.T.);
#12982=ORIENTED_EDGE('',*,*,#10162,.F.);
#12983=ORIENTED_EDGE('',*,*,#10163,.F.);
#12984=ORIENTED_EDGE('',*,*,#10164,.T.);
#12985=ORIENTED_EDGE('',*,*,#10163,.T.);
#12986=ORIENTED_EDGE('',*,*,#10165,.F.);
#12987=ORIENTED_EDGE('',*,*,#10166,.F.);
#12988=ORIENTED_EDGE('',*,*,#10167,.T.);
#12989=ORIENTED_EDGE('',*,*,#10166,.T.);
#12990=ORIENTED_EDGE('',*,*,#10168,.F.);
#12991=ORIENTED_EDGE('',*,*,#10158,.F.);
#12992=ORIENTED_EDGE('',*,*,#10168,.T.);
#12993=ORIENTED_EDGE('',*,*,#10165,.T.);
#12994=ORIENTED_EDGE('',*,*,#10162,.T.);
#12995=ORIENTED_EDGE('',*,*,#10159,.T.);
#12996=ORIENTED_EDGE('',*,*,#10129,.T.);
#12997=ORIENTED_EDGE('',*,*,#10132,.T.);
#12998=ORIENTED_EDGE('',*,*,#10135,.T.);
#12999=ORIENTED_EDGE('',*,*,#10153,.T.);
#13000=ORIENTED_EDGE('',*,*,#10167,.F.);
#13001=ORIENTED_EDGE('',*,*,#10157,.F.);
#13002=ORIENTED_EDGE('',*,*,#10161,.F.);
#13003=ORIENTED_EDGE('',*,*,#10164,.F.);
#13004=ORIENTED_EDGE('',*,*,#10154,.T.);
#13005=ORIENTED_EDGE('',*,*,#10145,.T.);
#13006=ORIENTED_EDGE('',*,*,#10142,.T.);
#13007=ORIENTED_EDGE('',*,*,#10139,.T.);
#13008=ORIENTED_EDGE('',*,*,#10136,.T.);
#13009=ORIENTED_EDGE('',*,*,#10169,.F.);
#13010=ORIENTED_EDGE('',*,*,#10170,.T.);
#13011=ORIENTED_EDGE('',*,*,#10171,.F.);
#13012=ORIENTED_EDGE('',*,*,#10170,.F.);
#13013=ORIENTED_EDGE('',*,*,#10172,.F.);
#13014=ORIENTED_EDGE('',*,*,#10173,.T.);
#13015=ORIENTED_EDGE('',*,*,#10174,.F.);
#13016=ORIENTED_EDGE('',*,*,#10173,.F.);
#13017=ORIENTED_EDGE('',*,*,#10175,.F.);
#13018=ORIENTED_EDGE('',*,*,#10176,.T.);
#13019=ORIENTED_EDGE('',*,*,#10177,.F.);
#13020=ORIENTED_EDGE('',*,*,#10176,.F.);
#13021=ORIENTED_EDGE('',*,*,#10178,.F.);
#13022=ORIENTED_EDGE('',*,*,#10179,.T.);
#13023=ORIENTED_EDGE('',*,*,#10180,.F.);
#13024=ORIENTED_EDGE('',*,*,#10179,.F.);
#13025=ORIENTED_EDGE('',*,*,#10181,.F.);
#13026=ORIENTED_EDGE('',*,*,#10182,.T.);
#13027=ORIENTED_EDGE('',*,*,#10183,.F.);
#13028=ORIENTED_EDGE('',*,*,#10182,.F.);
#13029=ORIENTED_EDGE('',*,*,#10184,.F.);
#13030=ORIENTED_EDGE('',*,*,#10185,.T.);
#13031=ORIENTED_EDGE('',*,*,#10186,.F.);
#13032=ORIENTED_EDGE('',*,*,#10185,.F.);
#13033=ORIENTED_EDGE('',*,*,#10184,.T.);
#13034=ORIENTED_EDGE('',*,*,#10187,.F.);
#13035=ORIENTED_EDGE('',*,*,#10188,.T.);
#13036=ORIENTED_EDGE('',*,*,#10189,.F.);
#13037=ORIENTED_EDGE('',*,*,#10188,.F.);
#13038=ORIENTED_EDGE('',*,*,#10187,.T.);
#13039=ORIENTED_EDGE('',*,*,#10190,.F.);
#13040=ORIENTED_EDGE('',*,*,#10191,.T.);
#13041=ORIENTED_EDGE('',*,*,#10192,.T.);
#13042=ORIENTED_EDGE('',*,*,#10191,.F.);
#13043=ORIENTED_EDGE('',*,*,#10192,.F.);
#13044=ORIENTED_EDGE('',*,*,#10193,.F.);
#13045=ORIENTED_EDGE('',*,*,#10194,.T.);
#13046=ORIENTED_EDGE('',*,*,#10195,.T.);
#13047=ORIENTED_EDGE('',*,*,#10194,.F.);
#13048=ORIENTED_EDGE('',*,*,#10195,.F.);
#13049=ORIENTED_EDGE('',*,*,#10196,.F.);
#13050=ORIENTED_EDGE('',*,*,#10197,.T.);
#13051=ORIENTED_EDGE('',*,*,#10198,.F.);
#13052=ORIENTED_EDGE('',*,*,#10197,.F.);
#13053=ORIENTED_EDGE('',*,*,#10196,.T.);
#13054=ORIENTED_EDGE('',*,*,#10199,.F.);
#13055=ORIENTED_EDGE('',*,*,#10200,.F.);
#13056=ORIENTED_EDGE('',*,*,#10201,.T.);
#13057=ORIENTED_EDGE('',*,*,#10199,.T.);
#13058=ORIENTED_EDGE('',*,*,#10201,.F.);
#13059=ORIENTED_EDGE('',*,*,#10202,.F.);
#13060=ORIENTED_EDGE('',*,*,#10203,.F.);
#13061=ORIENTED_EDGE('',*,*,#10204,.F.);
#13062=ORIENTED_EDGE('',*,*,#10205,.F.);
#13063=ORIENTED_EDGE('',*,*,#10206,.F.);
#13064=ORIENTED_EDGE('',*,*,#10207,.F.);
#13065=ORIENTED_EDGE('',*,*,#10208,.F.);
#13066=ORIENTED_EDGE('',*,*,#10209,.F.);
#13067=ORIENTED_EDGE('',*,*,#10208,.T.);
#13068=ORIENTED_EDGE('',*,*,#10210,.T.);
#13069=ORIENTED_EDGE('',*,*,#10211,.T.);
#13070=ORIENTED_EDGE('',*,*,#10212,.F.);
#13071=ORIENTED_EDGE('',*,*,#10186,.T.);
#13072=ORIENTED_EDGE('',*,*,#10189,.T.);
#13073=ORIENTED_EDGE('',*,*,#10203,.T.);
#13074=ORIENTED_EDGE('',*,*,#10213,.F.);
#13075=ORIENTED_EDGE('',*,*,#10214,.F.);
#13076=ORIENTED_EDGE('',*,*,#10210,.F.);
#13077=ORIENTED_EDGE('',*,*,#10207,.T.);
#13078=ORIENTED_EDGE('',*,*,#10215,.F.);
#13079=ORIENTED_EDGE('',*,*,#10169,.T.);
#13080=ORIENTED_EDGE('',*,*,#10172,.T.);
#13081=ORIENTED_EDGE('',*,*,#10175,.T.);
#13082=ORIENTED_EDGE('',*,*,#10178,.T.);
#13083=ORIENTED_EDGE('',*,*,#10181,.T.);
#13084=ORIENTED_EDGE('',*,*,#10200,.T.);
#13085=ORIENTED_EDGE('',*,*,#10204,.T.);
#13086=ORIENTED_EDGE('',*,*,#10215,.T.);
#13087=ORIENTED_EDGE('',*,*,#10206,.T.);
#13088=ORIENTED_EDGE('',*,*,#10216,.F.);
#13089=ORIENTED_EDGE('',*,*,#10214,.T.);
#13090=ORIENTED_EDGE('',*,*,#10217,.T.);
#13091=ORIENTED_EDGE('',*,*,#10218,.F.);
#13092=ORIENTED_EDGE('',*,*,#10211,.F.);
#13093=ORIENTED_EDGE('',*,*,#10202,.T.);
#13094=ORIENTED_EDGE('',*,*,#10219,.F.);
#13095=ORIENTED_EDGE('',*,*,#10217,.F.);
#13096=ORIENTED_EDGE('',*,*,#10213,.T.);
#13097=ORIENTED_EDGE('',*,*,#10190,.T.);
#13098=ORIENTED_EDGE('',*,*,#10193,.T.);
#13099=ORIENTED_EDGE('',*,*,#10205,.T.);
#13100=ORIENTED_EDGE('',*,*,#10216,.T.);
#13101=ORIENTED_EDGE('',*,*,#10209,.T.);
#13102=ORIENTED_EDGE('',*,*,#10212,.T.);
#13103=ORIENTED_EDGE('',*,*,#10218,.T.);
#13104=ORIENTED_EDGE('',*,*,#10219,.T.);
#13105=ORIENTED_EDGE('',*,*,#10171,.T.);
#13106=ORIENTED_EDGE('',*,*,#10174,.T.);
#13107=ORIENTED_EDGE('',*,*,#10177,.T.);
#13108=ORIENTED_EDGE('',*,*,#10180,.T.);
#13109=ORIENTED_EDGE('',*,*,#10183,.T.);
#13110=ORIENTED_EDGE('',*,*,#10198,.T.);
#13111=ORIENTED_EDGE('',*,*,#10220,.F.);
#13112=ORIENTED_EDGE('',*,*,#10221,.T.);
#13113=ORIENTED_EDGE('',*,*,#10222,.F.);
#13114=ORIENTED_EDGE('',*,*,#10221,.F.);
#13115=ORIENTED_EDGE('',*,*,#10223,.F.);
#13116=ORIENTED_EDGE('',*,*,#10224,.T.);
#13117=ORIENTED_EDGE('',*,*,#10225,.F.);
#13118=ORIENTED_EDGE('',*,*,#10224,.F.);
#13119=ORIENTED_EDGE('',*,*,#10226,.F.);
#13120=ORIENTED_EDGE('',*,*,#10227,.T.);
#13121=ORIENTED_EDGE('',*,*,#10228,.F.);
#13122=ORIENTED_EDGE('',*,*,#10227,.F.);
#13123=ORIENTED_EDGE('',*,*,#10229,.F.);
#13124=ORIENTED_EDGE('',*,*,#10230,.T.);
#13125=ORIENTED_EDGE('',*,*,#10231,.F.);
#13126=ORIENTED_EDGE('',*,*,#10230,.F.);
#13127=ORIENTED_EDGE('',*,*,#10229,.T.);
#13128=ORIENTED_EDGE('',*,*,#10232,.T.);
#13129=ORIENTED_EDGE('',*,*,#10232,.F.);
#13130=ORIENTED_EDGE('',*,*,#10233,.T.);
#13131=ORIENTED_EDGE('',*,*,#10234,.T.);
#13132=ORIENTED_EDGE('',*,*,#10233,.F.);
#13133=ORIENTED_EDGE('',*,*,#10235,.F.);
#13134=ORIENTED_EDGE('',*,*,#10236,.T.);
#13135=ORIENTED_EDGE('',*,*,#10237,.T.);
#13136=ORIENTED_EDGE('',*,*,#10236,.F.);
#13137=ORIENTED_EDGE('',*,*,#10235,.T.);
#13138=ORIENTED_EDGE('',*,*,#10222,.T.);
#13139=ORIENTED_EDGE('',*,*,#10225,.T.);
#13140=ORIENTED_EDGE('',*,*,#10228,.T.);
#13141=ORIENTED_EDGE('',*,*,#10231,.T.);
#13142=ORIENTED_EDGE('',*,*,#10237,.F.);
#13143=ORIENTED_EDGE('',*,*,#10220,.T.);
#13144=ORIENTED_EDGE('',*,*,#10223,.T.);
#13145=ORIENTED_EDGE('',*,*,#10226,.T.);
#13146=ORIENTED_EDGE('',*,*,#10234,.F.);
#13147=ORIENTED_EDGE('',*,*,#10238,.F.);
#13148=ORIENTED_EDGE('',*,*,#10239,.T.);
#13149=ORIENTED_EDGE('',*,*,#10240,.F.);
#13150=ORIENTED_EDGE('',*,*,#10239,.F.);
#13151=ORIENTED_EDGE('',*,*,#10241,.F.);
#13152=ORIENTED_EDGE('',*,*,#10242,.T.);
#13153=ORIENTED_EDGE('',*,*,#10243,.F.);
#13154=ORIENTED_EDGE('',*,*,#10242,.F.);
#13155=ORIENTED_EDGE('',*,*,#10244,.F.);
#13156=ORIENTED_EDGE('',*,*,#10245,.T.);
#13157=ORIENTED_EDGE('',*,*,#10246,.F.);
#13158=ORIENTED_EDGE('',*,*,#10245,.F.);
#13159=ORIENTED_EDGE('',*,*,#10247,.F.);
#13160=ORIENTED_EDGE('',*,*,#10248,.T.);
#13161=ORIENTED_EDGE('',*,*,#10249,.T.);
#13162=ORIENTED_EDGE('',*,*,#10248,.F.);
#13163=ORIENTED_EDGE('',*,*,#10249,.F.);
#13164=ORIENTED_EDGE('',*,*,#10250,.F.);
#13165=ORIENTED_EDGE('',*,*,#10251,.F.);
#13166=ORIENTED_EDGE('',*,*,#10252,.T.);
#13167=ORIENTED_EDGE('',*,*,#10250,.T.);
#13168=ORIENTED_EDGE('',*,*,#10252,.F.);
#13169=ORIENTED_EDGE('',*,*,#10253,.F.);
#13170=ORIENTED_EDGE('',*,*,#10254,.T.);
#13171=ORIENTED_EDGE('',*,*,#10255,.T.);
#13172=ORIENTED_EDGE('',*,*,#10254,.F.);
#13173=ORIENTED_EDGE('',*,*,#10253,.T.);
#13174=ORIENTED_EDGE('',*,*,#10240,.T.);
#13175=ORIENTED_EDGE('',*,*,#10243,.T.);
#13176=ORIENTED_EDGE('',*,*,#10246,.T.);
#13177=ORIENTED_EDGE('',*,*,#10251,.T.);
#13178=ORIENTED_EDGE('',*,*,#10255,.F.);
#13179=ORIENTED_EDGE('',*,*,#10238,.T.);
#13180=ORIENTED_EDGE('',*,*,#10241,.T.);
#13181=ORIENTED_EDGE('',*,*,#10244,.T.);
#13182=ORIENTED_EDGE('',*,*,#10247,.T.);
#13183=ORIENTED_EDGE('',*,*,#10256,.F.);
#13184=ORIENTED_EDGE('',*,*,#10257,.T.);
#13185=ORIENTED_EDGE('',*,*,#10258,.T.);
#13186=ORIENTED_EDGE('',*,*,#10257,.F.);
#13187=ORIENTED_EDGE('',*,*,#10258,.F.);
#13188=ORIENTED_EDGE('',*,*,#10259,.F.);
#13189=ORIENTED_EDGE('',*,*,#10260,.T.);
#13190=ORIENTED_EDGE('',*,*,#10261,.T.);
#13191=ORIENTED_EDGE('',*,*,#10260,.F.);
#13192=ORIENTED_EDGE('',*,*,#10259,.T.);
#13193=ORIENTED_EDGE('',*,*,#10261,.F.);
#13194=ORIENTED_EDGE('',*,*,#10256,.T.);
#13195=ORIENTED_EDGE('',*,*,#10262,.F.);
#13196=ORIENTED_EDGE('',*,*,#10263,.T.);
#13197=ORIENTED_EDGE('',*,*,#10264,.F.);
#13198=ORIENTED_EDGE('',*,*,#10263,.F.);
#13199=ORIENTED_EDGE('',*,*,#10262,.T.);
#13200=ORIENTED_EDGE('',*,*,#10265,.F.);
#13201=ORIENTED_EDGE('',*,*,#10266,.T.);
#13202=ORIENTED_EDGE('',*,*,#10267,.T.);
#13203=ORIENTED_EDGE('',*,*,#10266,.F.);
#13204=ORIENTED_EDGE('',*,*,#10265,.T.);
#13205=ORIENTED_EDGE('',*,*,#10264,.T.);
#13206=ORIENTED_EDGE('',*,*,#10267,.F.);
#13207=ORIENTED_EDGE('',*,*,#10268,.F.);
#13208=ORIENTED_EDGE('',*,*,#10269,.T.);
#13209=ORIENTED_EDGE('',*,*,#10270,.T.);
#13210=ORIENTED_EDGE('',*,*,#10269,.F.);
#13211=ORIENTED_EDGE('',*,*,#10270,.F.);
#13212=ORIENTED_EDGE('',*,*,#10271,.F.);
#13213=ORIENTED_EDGE('',*,*,#10272,.T.);
#13214=ORIENTED_EDGE('',*,*,#10273,.T.);
#13215=ORIENTED_EDGE('',*,*,#10272,.F.);
#13216=ORIENTED_EDGE('',*,*,#10271,.T.);
#13217=ORIENTED_EDGE('',*,*,#10273,.F.);
#13218=ORIENTED_EDGE('',*,*,#10268,.T.);
#13219=ORIENTED_EDGE('',*,*,#10274,.F.);
#13220=ORIENTED_EDGE('',*,*,#10275,.T.);
#13221=ORIENTED_EDGE('',*,*,#10276,.F.);
#13222=ORIENTED_EDGE('',*,*,#10275,.F.);
#13223=ORIENTED_EDGE('',*,*,#10274,.T.);
#13224=ORIENTED_EDGE('',*,*,#10277,.F.);
#13225=ORIENTED_EDGE('',*,*,#10278,.T.);
#13226=ORIENTED_EDGE('',*,*,#10279,.T.);
#13227=ORIENTED_EDGE('',*,*,#10278,.F.);
#13228=ORIENTED_EDGE('',*,*,#10277,.T.);
#13229=ORIENTED_EDGE('',*,*,#10276,.T.);
#13230=ORIENTED_EDGE('',*,*,#10279,.F.);
#13231=ORIENTED_EDGE('',*,*,#10280,.F.);
#13232=ORIENTED_EDGE('',*,*,#10281,.T.);
#13233=ORIENTED_EDGE('',*,*,#10282,.F.);
#13234=ORIENTED_EDGE('',*,*,#10281,.F.);
#13235=ORIENTED_EDGE('',*,*,#10280,.T.);
#13236=ORIENTED_EDGE('',*,*,#10283,.F.);
#13237=ORIENTED_EDGE('',*,*,#10284,.F.);
#13238=ORIENTED_EDGE('',*,*,#10285,.T.);
#13239=ORIENTED_EDGE('',*,*,#10286,.F.);
#13240=ORIENTED_EDGE('',*,*,#10285,.F.);
#13241=ORIENTED_EDGE('',*,*,#10284,.T.);
#13242=ORIENTED_EDGE('',*,*,#10287,.F.);
#13243=ORIENTED_EDGE('',*,*,#10288,.F.);
#13244=ORIENTED_EDGE('',*,*,#10289,.T.);
#13245=ORIENTED_EDGE('',*,*,#10290,.F.);
#13246=ORIENTED_EDGE('',*,*,#10289,.F.);
#13247=ORIENTED_EDGE('',*,*,#10288,.T.);
#13248=ORIENTED_EDGE('',*,*,#10291,.F.);
#13249=ORIENTED_EDGE('',*,*,#10292,.F.);
#13250=ORIENTED_EDGE('',*,*,#10293,.T.);
#13251=ORIENTED_EDGE('',*,*,#10294,.F.);
#13252=ORIENTED_EDGE('',*,*,#10293,.F.);
#13253=ORIENTED_EDGE('',*,*,#10292,.T.);
#13254=ORIENTED_EDGE('',*,*,#10295,.F.);
#13255=ORIENTED_EDGE('',*,*,#10296,.F.);
#13256=ORIENTED_EDGE('',*,*,#10297,.T.);
#13257=ORIENTED_EDGE('',*,*,#10283,.T.);
#13258=ORIENTED_EDGE('',*,*,#10297,.F.);
#13259=ORIENTED_EDGE('',*,*,#10298,.F.);
#13260=ORIENTED_EDGE('',*,*,#10299,.T.);
#13261=ORIENTED_EDGE('',*,*,#10287,.T.);
#13262=ORIENTED_EDGE('',*,*,#10299,.F.);
#13263=ORIENTED_EDGE('',*,*,#10300,.F.);
#13264=ORIENTED_EDGE('',*,*,#10301,.T.);
#13265=ORIENTED_EDGE('',*,*,#10291,.T.);
#13266=ORIENTED_EDGE('',*,*,#10301,.F.);
#13267=ORIENTED_EDGE('',*,*,#10302,.F.);
#13268=ORIENTED_EDGE('',*,*,#10303,.T.);
#13269=ORIENTED_EDGE('',*,*,#10295,.T.);
#13270=ORIENTED_EDGE('',*,*,#10303,.F.);
#13271=ORIENTED_EDGE('',*,*,#10304,.F.);
#13272=ORIENTED_EDGE('',*,*,#10305,.T.);
#13273=ORIENTED_EDGE('',*,*,#10306,.T.);
#13274=ORIENTED_EDGE('',*,*,#10305,.F.);
#13275=ORIENTED_EDGE('',*,*,#10304,.T.);
#13276=ORIENTED_EDGE('',*,*,#10294,.T.);
#13277=ORIENTED_EDGE('',*,*,#10290,.T.);
#13278=ORIENTED_EDGE('',*,*,#10286,.T.);
#13279=ORIENTED_EDGE('',*,*,#10282,.T.);
#13280=ORIENTED_EDGE('',*,*,#10306,.F.);
#13281=ORIENTED_EDGE('',*,*,#10296,.T.);
#13282=ORIENTED_EDGE('',*,*,#10298,.T.);
#13283=ORIENTED_EDGE('',*,*,#10300,.T.);
#13284=ORIENTED_EDGE('',*,*,#10302,.T.);
#13285=ORIENTED_EDGE('',*,*,#10307,.F.);
#13286=ORIENTED_EDGE('',*,*,#10308,.T.);
#13287=ORIENTED_EDGE('',*,*,#10309,.T.);
#13288=ORIENTED_EDGE('',*,*,#10310,.F.);
#13289=ORIENTED_EDGE('',*,*,#10311,.F.);
#13290=ORIENTED_EDGE('',*,*,#10310,.T.);
#13291=ORIENTED_EDGE('',*,*,#10312,.T.);
#13292=ORIENTED_EDGE('',*,*,#10313,.F.);
#13293=ORIENTED_EDGE('',*,*,#10314,.F.);
#13294=ORIENTED_EDGE('',*,*,#10313,.T.);
#13295=ORIENTED_EDGE('',*,*,#10315,.T.);
#13296=ORIENTED_EDGE('',*,*,#10316,.F.);
#13297=ORIENTED_EDGE('',*,*,#10317,.F.);
#13298=ORIENTED_EDGE('',*,*,#10316,.T.);
#13299=ORIENTED_EDGE('',*,*,#10318,.T.);
#13300=ORIENTED_EDGE('',*,*,#10308,.F.);
#13301=ORIENTED_EDGE('',*,*,#10318,.F.);
#13302=ORIENTED_EDGE('',*,*,#10315,.F.);
#13303=ORIENTED_EDGE('',*,*,#10312,.F.);
#13304=ORIENTED_EDGE('',*,*,#10309,.F.);
#13305=ORIENTED_EDGE('',*,*,#10319,.F.);
#13306=ORIENTED_EDGE('',*,*,#10320,.T.);
#13307=ORIENTED_EDGE('',*,*,#10321,.T.);
#13308=ORIENTED_EDGE('',*,*,#10322,.F.);
#13309=ORIENTED_EDGE('',*,*,#10323,.F.);
#13310=ORIENTED_EDGE('',*,*,#10322,.T.);
#13311=ORIENTED_EDGE('',*,*,#10324,.T.);
#13312=ORIENTED_EDGE('',*,*,#10325,.F.);
#13313=ORIENTED_EDGE('',*,*,#10326,.F.);
#13314=ORIENTED_EDGE('',*,*,#10325,.T.);
#13315=ORIENTED_EDGE('',*,*,#10327,.T.);
#13316=ORIENTED_EDGE('',*,*,#10328,.F.);
#13317=ORIENTED_EDGE('',*,*,#10329,.F.);
#13318=ORIENTED_EDGE('',*,*,#10328,.T.);
#13319=ORIENTED_EDGE('',*,*,#10330,.T.);
#13320=ORIENTED_EDGE('',*,*,#10320,.F.);
#13321=ORIENTED_EDGE('',*,*,#10330,.F.);
#13322=ORIENTED_EDGE('',*,*,#10327,.F.);
#13323=ORIENTED_EDGE('',*,*,#10324,.F.);
#13324=ORIENTED_EDGE('',*,*,#10321,.F.);
#13325=ORIENTED_EDGE('',*,*,#10331,.F.);
#13326=ORIENTED_EDGE('',*,*,#10332,.T.);
#13327=ORIENTED_EDGE('',*,*,#10333,.T.);
#13328=ORIENTED_EDGE('',*,*,#10334,.F.);
#13329=ORIENTED_EDGE('',*,*,#10335,.F.);
#13330=ORIENTED_EDGE('',*,*,#10334,.T.);
#13331=ORIENTED_EDGE('',*,*,#10336,.T.);
#13332=ORIENTED_EDGE('',*,*,#10337,.F.);
#13333=ORIENTED_EDGE('',*,*,#10338,.F.);
#13334=ORIENTED_EDGE('',*,*,#10337,.T.);
#13335=ORIENTED_EDGE('',*,*,#10339,.T.);
#13336=ORIENTED_EDGE('',*,*,#10340,.F.);
#13337=ORIENTED_EDGE('',*,*,#10341,.F.);
#13338=ORIENTED_EDGE('',*,*,#10340,.T.);
#13339=ORIENTED_EDGE('',*,*,#10342,.T.);
#13340=ORIENTED_EDGE('',*,*,#10332,.F.);
#13341=ORIENTED_EDGE('',*,*,#10342,.F.);
#13342=ORIENTED_EDGE('',*,*,#10339,.F.);
#13343=ORIENTED_EDGE('',*,*,#10336,.F.);
#13344=ORIENTED_EDGE('',*,*,#10333,.F.);
#13345=ORIENTED_EDGE('',*,*,#10343,.F.);
#13346=ORIENTED_EDGE('',*,*,#10344,.T.);
#13347=ORIENTED_EDGE('',*,*,#10345,.T.);
#13348=ORIENTED_EDGE('',*,*,#10346,.F.);
#13349=ORIENTED_EDGE('',*,*,#10347,.F.);
#13350=ORIENTED_EDGE('',*,*,#10346,.T.);
#13351=ORIENTED_EDGE('',*,*,#10348,.T.);
#13352=ORIENTED_EDGE('',*,*,#10349,.F.);
#13353=ORIENTED_EDGE('',*,*,#10350,.F.);
#13354=ORIENTED_EDGE('',*,*,#10349,.T.);
#13355=ORIENTED_EDGE('',*,*,#10351,.T.);
#13356=ORIENTED_EDGE('',*,*,#10352,.F.);
#13357=ORIENTED_EDGE('',*,*,#10353,.F.);
#13358=ORIENTED_EDGE('',*,*,#10352,.T.);
#13359=ORIENTED_EDGE('',*,*,#10354,.T.);
#13360=ORIENTED_EDGE('',*,*,#10344,.F.);
#13361=ORIENTED_EDGE('',*,*,#10354,.F.);
#13362=ORIENTED_EDGE('',*,*,#10351,.F.);
#13363=ORIENTED_EDGE('',*,*,#10348,.F.);
#13364=ORIENTED_EDGE('',*,*,#10345,.F.);
#13365=ORIENTED_EDGE('',*,*,#10355,.F.);
#13366=ORIENTED_EDGE('',*,*,#10356,.T.);
#13367=ORIENTED_EDGE('',*,*,#10357,.T.);
#13368=ORIENTED_EDGE('',*,*,#10358,.F.);
#13369=ORIENTED_EDGE('',*,*,#10359,.F.);
#13370=ORIENTED_EDGE('',*,*,#10358,.T.);
#13371=ORIENTED_EDGE('',*,*,#10360,.T.);
#13372=ORIENTED_EDGE('',*,*,#10361,.F.);
#13373=ORIENTED_EDGE('',*,*,#10362,.F.);
#13374=ORIENTED_EDGE('',*,*,#10361,.T.);
#13375=ORIENTED_EDGE('',*,*,#10363,.T.);
#13376=ORIENTED_EDGE('',*,*,#10364,.F.);
#13377=ORIENTED_EDGE('',*,*,#10365,.F.);
#13378=ORIENTED_EDGE('',*,*,#10364,.T.);
#13379=ORIENTED_EDGE('',*,*,#10366,.T.);
#13380=ORIENTED_EDGE('',*,*,#10356,.F.);
#13381=ORIENTED_EDGE('',*,*,#10366,.F.);
#13382=ORIENTED_EDGE('',*,*,#10363,.F.);
#13383=ORIENTED_EDGE('',*,*,#10360,.F.);
#13384=ORIENTED_EDGE('',*,*,#10357,.F.);
#13385=ORIENTED_EDGE('',*,*,#10367,.F.);
#13386=ORIENTED_EDGE('',*,*,#10368,.T.);
#13387=ORIENTED_EDGE('',*,*,#10369,.T.);
#13388=ORIENTED_EDGE('',*,*,#10370,.F.);
#13389=ORIENTED_EDGE('',*,*,#10371,.F.);
#13390=ORIENTED_EDGE('',*,*,#10370,.T.);
#13391=ORIENTED_EDGE('',*,*,#10372,.T.);
#13392=ORIENTED_EDGE('',*,*,#10373,.F.);
#13393=ORIENTED_EDGE('',*,*,#10374,.F.);
#13394=ORIENTED_EDGE('',*,*,#10373,.T.);
#13395=ORIENTED_EDGE('',*,*,#10375,.T.);
#13396=ORIENTED_EDGE('',*,*,#10376,.F.);
#13397=ORIENTED_EDGE('',*,*,#10377,.F.);
#13398=ORIENTED_EDGE('',*,*,#10376,.T.);
#13399=ORIENTED_EDGE('',*,*,#10378,.T.);
#13400=ORIENTED_EDGE('',*,*,#10368,.F.);
#13401=ORIENTED_EDGE('',*,*,#10378,.F.);
#13402=ORIENTED_EDGE('',*,*,#10375,.F.);
#13403=ORIENTED_EDGE('',*,*,#10372,.F.);
#13404=ORIENTED_EDGE('',*,*,#10369,.F.);
#13405=ORIENTED_EDGE('',*,*,#10379,.F.);
#13406=ORIENTED_EDGE('',*,*,#10380,.T.);
#13407=ORIENTED_EDGE('',*,*,#10381,.T.);
#13408=ORIENTED_EDGE('',*,*,#10382,.F.);
#13409=ORIENTED_EDGE('',*,*,#10383,.F.);
#13410=ORIENTED_EDGE('',*,*,#10382,.T.);
#13411=ORIENTED_EDGE('',*,*,#10384,.T.);
#13412=ORIENTED_EDGE('',*,*,#10385,.F.);
#13413=ORIENTED_EDGE('',*,*,#10386,.F.);
#13414=ORIENTED_EDGE('',*,*,#10385,.T.);
#13415=ORIENTED_EDGE('',*,*,#10387,.T.);
#13416=ORIENTED_EDGE('',*,*,#10388,.F.);
#13417=ORIENTED_EDGE('',*,*,#10389,.F.);
#13418=ORIENTED_EDGE('',*,*,#10388,.T.);
#13419=ORIENTED_EDGE('',*,*,#10390,.T.);
#13420=ORIENTED_EDGE('',*,*,#10380,.F.);
#13421=ORIENTED_EDGE('',*,*,#10390,.F.);
#13422=ORIENTED_EDGE('',*,*,#10387,.F.);
#13423=ORIENTED_EDGE('',*,*,#10384,.F.);
#13424=ORIENTED_EDGE('',*,*,#10381,.F.);
#13425=ORIENTED_EDGE('',*,*,#10391,.F.);
#13426=ORIENTED_EDGE('',*,*,#10392,.T.);
#13427=ORIENTED_EDGE('',*,*,#10393,.T.);
#13428=ORIENTED_EDGE('',*,*,#10394,.F.);
#13429=ORIENTED_EDGE('',*,*,#10395,.F.);
#13430=ORIENTED_EDGE('',*,*,#10394,.T.);
#13431=ORIENTED_EDGE('',*,*,#10396,.T.);
#13432=ORIENTED_EDGE('',*,*,#10397,.F.);
#13433=ORIENTED_EDGE('',*,*,#10398,.F.);
#13434=ORIENTED_EDGE('',*,*,#10397,.T.);
#13435=ORIENTED_EDGE('',*,*,#10399,.T.);
#13436=ORIENTED_EDGE('',*,*,#10400,.F.);
#13437=ORIENTED_EDGE('',*,*,#10401,.F.);
#13438=ORIENTED_EDGE('',*,*,#10400,.T.);
#13439=ORIENTED_EDGE('',*,*,#10402,.T.);
#13440=ORIENTED_EDGE('',*,*,#10392,.F.);
#13441=ORIENTED_EDGE('',*,*,#10402,.F.);
#13442=ORIENTED_EDGE('',*,*,#10399,.F.);
#13443=ORIENTED_EDGE('',*,*,#10396,.F.);
#13444=ORIENTED_EDGE('',*,*,#10393,.F.);
#13445=ORIENTED_EDGE('',*,*,#10403,.F.);
#13446=ORIENTED_EDGE('',*,*,#10404,.T.);
#13447=ORIENTED_EDGE('',*,*,#10405,.T.);
#13448=ORIENTED_EDGE('',*,*,#10406,.F.);
#13449=ORIENTED_EDGE('',*,*,#10407,.F.);
#13450=ORIENTED_EDGE('',*,*,#10406,.T.);
#13451=ORIENTED_EDGE('',*,*,#10408,.T.);
#13452=ORIENTED_EDGE('',*,*,#10409,.F.);
#13453=ORIENTED_EDGE('',*,*,#10410,.F.);
#13454=ORIENTED_EDGE('',*,*,#10409,.T.);
#13455=ORIENTED_EDGE('',*,*,#10411,.T.);
#13456=ORIENTED_EDGE('',*,*,#10412,.F.);
#13457=ORIENTED_EDGE('',*,*,#10413,.F.);
#13458=ORIENTED_EDGE('',*,*,#10412,.T.);
#13459=ORIENTED_EDGE('',*,*,#10414,.T.);
#13460=ORIENTED_EDGE('',*,*,#10404,.F.);
#13461=ORIENTED_EDGE('',*,*,#10414,.F.);
#13462=ORIENTED_EDGE('',*,*,#10411,.F.);
#13463=ORIENTED_EDGE('',*,*,#10408,.F.);
#13464=ORIENTED_EDGE('',*,*,#10405,.F.);
#13465=ORIENTED_EDGE('',*,*,#10415,.F.);
#13466=ORIENTED_EDGE('',*,*,#10416,.T.);
#13467=ORIENTED_EDGE('',*,*,#10417,.T.);
#13468=ORIENTED_EDGE('',*,*,#10418,.F.);
#13469=ORIENTED_EDGE('',*,*,#10419,.F.);
#13470=ORIENTED_EDGE('',*,*,#10418,.T.);
#13471=ORIENTED_EDGE('',*,*,#10420,.T.);
#13472=ORIENTED_EDGE('',*,*,#10421,.F.);
#13473=ORIENTED_EDGE('',*,*,#10422,.F.);
#13474=ORIENTED_EDGE('',*,*,#10421,.T.);
#13475=ORIENTED_EDGE('',*,*,#10423,.T.);
#13476=ORIENTED_EDGE('',*,*,#10424,.F.);
#13477=ORIENTED_EDGE('',*,*,#10425,.F.);
#13478=ORIENTED_EDGE('',*,*,#10424,.T.);
#13479=ORIENTED_EDGE('',*,*,#10426,.T.);
#13480=ORIENTED_EDGE('',*,*,#10416,.F.);
#13481=ORIENTED_EDGE('',*,*,#10426,.F.);
#13482=ORIENTED_EDGE('',*,*,#10423,.F.);
#13483=ORIENTED_EDGE('',*,*,#10420,.F.);
#13484=ORIENTED_EDGE('',*,*,#10417,.F.);
#13485=ORIENTED_EDGE('',*,*,#10427,.F.);
#13486=ORIENTED_EDGE('',*,*,#10428,.T.);
#13487=ORIENTED_EDGE('',*,*,#10429,.T.);
#13488=ORIENTED_EDGE('',*,*,#10430,.F.);
#13489=ORIENTED_EDGE('',*,*,#10431,.F.);
#13490=ORIENTED_EDGE('',*,*,#10430,.T.);
#13491=ORIENTED_EDGE('',*,*,#10432,.T.);
#13492=ORIENTED_EDGE('',*,*,#10433,.F.);
#13493=ORIENTED_EDGE('',*,*,#10434,.F.);
#13494=ORIENTED_EDGE('',*,*,#10433,.T.);
#13495=ORIENTED_EDGE('',*,*,#10435,.T.);
#13496=ORIENTED_EDGE('',*,*,#10436,.F.);
#13497=ORIENTED_EDGE('',*,*,#10437,.F.);
#13498=ORIENTED_EDGE('',*,*,#10436,.T.);
#13499=ORIENTED_EDGE('',*,*,#10438,.T.);
#13500=ORIENTED_EDGE('',*,*,#10428,.F.);
#13501=ORIENTED_EDGE('',*,*,#10438,.F.);
#13502=ORIENTED_EDGE('',*,*,#10435,.F.);
#13503=ORIENTED_EDGE('',*,*,#10432,.F.);
#13504=ORIENTED_EDGE('',*,*,#10429,.F.);
#13505=ORIENTED_EDGE('',*,*,#10439,.F.);
#13506=ORIENTED_EDGE('',*,*,#10440,.T.);
#13507=ORIENTED_EDGE('',*,*,#10441,.T.);
#13508=ORIENTED_EDGE('',*,*,#10442,.F.);
#13509=ORIENTED_EDGE('',*,*,#10443,.F.);
#13510=ORIENTED_EDGE('',*,*,#10442,.T.);
#13511=ORIENTED_EDGE('',*,*,#10444,.T.);
#13512=ORIENTED_EDGE('',*,*,#10445,.F.);
#13513=ORIENTED_EDGE('',*,*,#10446,.F.);
#13514=ORIENTED_EDGE('',*,*,#10445,.T.);
#13515=ORIENTED_EDGE('',*,*,#10447,.T.);
#13516=ORIENTED_EDGE('',*,*,#10448,.F.);
#13517=ORIENTED_EDGE('',*,*,#10449,.F.);
#13518=ORIENTED_EDGE('',*,*,#10448,.T.);
#13519=ORIENTED_EDGE('',*,*,#10450,.T.);
#13520=ORIENTED_EDGE('',*,*,#10440,.F.);
#13521=ORIENTED_EDGE('',*,*,#10450,.F.);
#13522=ORIENTED_EDGE('',*,*,#10447,.F.);
#13523=ORIENTED_EDGE('',*,*,#10444,.F.);
#13524=ORIENTED_EDGE('',*,*,#10441,.F.);
#13525=ORIENTED_EDGE('',*,*,#10451,.F.);
#13526=ORIENTED_EDGE('',*,*,#10452,.T.);
#13527=ORIENTED_EDGE('',*,*,#10453,.T.);
#13528=ORIENTED_EDGE('',*,*,#10454,.F.);
#13529=ORIENTED_EDGE('',*,*,#10455,.F.);
#13530=ORIENTED_EDGE('',*,*,#10454,.T.);
#13531=ORIENTED_EDGE('',*,*,#10456,.T.);
#13532=ORIENTED_EDGE('',*,*,#10457,.F.);
#13533=ORIENTED_EDGE('',*,*,#10458,.F.);
#13534=ORIENTED_EDGE('',*,*,#10457,.T.);
#13535=ORIENTED_EDGE('',*,*,#10459,.T.);
#13536=ORIENTED_EDGE('',*,*,#10460,.F.);
#13537=ORIENTED_EDGE('',*,*,#10461,.F.);
#13538=ORIENTED_EDGE('',*,*,#10460,.T.);
#13539=ORIENTED_EDGE('',*,*,#10462,.T.);
#13540=ORIENTED_EDGE('',*,*,#10452,.F.);
#13541=ORIENTED_EDGE('',*,*,#10462,.F.);
#13542=ORIENTED_EDGE('',*,*,#10459,.F.);
#13543=ORIENTED_EDGE('',*,*,#10456,.F.);
#13544=ORIENTED_EDGE('',*,*,#10453,.F.);
#13545=ORIENTED_EDGE('',*,*,#10463,.F.);
#13546=ORIENTED_EDGE('',*,*,#10464,.T.);
#13547=ORIENTED_EDGE('',*,*,#10465,.T.);
#13548=ORIENTED_EDGE('',*,*,#10466,.F.);
#13549=ORIENTED_EDGE('',*,*,#10467,.F.);
#13550=ORIENTED_EDGE('',*,*,#10466,.T.);
#13551=ORIENTED_EDGE('',*,*,#10468,.T.);
#13552=ORIENTED_EDGE('',*,*,#10469,.F.);
#13553=ORIENTED_EDGE('',*,*,#10470,.F.);
#13554=ORIENTED_EDGE('',*,*,#10469,.T.);
#13555=ORIENTED_EDGE('',*,*,#10471,.T.);
#13556=ORIENTED_EDGE('',*,*,#10472,.F.);
#13557=ORIENTED_EDGE('',*,*,#10473,.F.);
#13558=ORIENTED_EDGE('',*,*,#10472,.T.);
#13559=ORIENTED_EDGE('',*,*,#10474,.T.);
#13560=ORIENTED_EDGE('',*,*,#10464,.F.);
#13561=ORIENTED_EDGE('',*,*,#10474,.F.);
#13562=ORIENTED_EDGE('',*,*,#10471,.F.);
#13563=ORIENTED_EDGE('',*,*,#10468,.F.);
#13564=ORIENTED_EDGE('',*,*,#10465,.F.);
#13565=ORIENTED_EDGE('',*,*,#10475,.F.);
#13566=ORIENTED_EDGE('',*,*,#10476,.T.);
#13567=ORIENTED_EDGE('',*,*,#10477,.T.);
#13568=ORIENTED_EDGE('',*,*,#10478,.F.);
#13569=ORIENTED_EDGE('',*,*,#10479,.F.);
#13570=ORIENTED_EDGE('',*,*,#10478,.T.);
#13571=ORIENTED_EDGE('',*,*,#10480,.T.);
#13572=ORIENTED_EDGE('',*,*,#10481,.F.);
#13573=ORIENTED_EDGE('',*,*,#10482,.F.);
#13574=ORIENTED_EDGE('',*,*,#10481,.T.);
#13575=ORIENTED_EDGE('',*,*,#10483,.T.);
#13576=ORIENTED_EDGE('',*,*,#10484,.F.);
#13577=ORIENTED_EDGE('',*,*,#10485,.F.);
#13578=ORIENTED_EDGE('',*,*,#10484,.T.);
#13579=ORIENTED_EDGE('',*,*,#10486,.T.);
#13580=ORIENTED_EDGE('',*,*,#10476,.F.);
#13581=ORIENTED_EDGE('',*,*,#10486,.F.);
#13582=ORIENTED_EDGE('',*,*,#10483,.F.);
#13583=ORIENTED_EDGE('',*,*,#10480,.F.);
#13584=ORIENTED_EDGE('',*,*,#10477,.F.);
#13585=ORIENTED_EDGE('',*,*,#10487,.F.);
#13586=ORIENTED_EDGE('',*,*,#10488,.T.);
#13587=ORIENTED_EDGE('',*,*,#10489,.T.);
#13588=ORIENTED_EDGE('',*,*,#10490,.F.);
#13589=ORIENTED_EDGE('',*,*,#10491,.F.);
#13590=ORIENTED_EDGE('',*,*,#10490,.T.);
#13591=ORIENTED_EDGE('',*,*,#10492,.T.);
#13592=ORIENTED_EDGE('',*,*,#10493,.F.);
#13593=ORIENTED_EDGE('',*,*,#10494,.F.);
#13594=ORIENTED_EDGE('',*,*,#10493,.T.);
#13595=ORIENTED_EDGE('',*,*,#10495,.T.);
#13596=ORIENTED_EDGE('',*,*,#10496,.F.);
#13597=ORIENTED_EDGE('',*,*,#10497,.F.);
#13598=ORIENTED_EDGE('',*,*,#10496,.T.);
#13599=ORIENTED_EDGE('',*,*,#10498,.T.);
#13600=ORIENTED_EDGE('',*,*,#10488,.F.);
#13601=ORIENTED_EDGE('',*,*,#10498,.F.);
#13602=ORIENTED_EDGE('',*,*,#10495,.F.);
#13603=ORIENTED_EDGE('',*,*,#10492,.F.);
#13604=ORIENTED_EDGE('',*,*,#10489,.F.);
#13605=ORIENTED_EDGE('',*,*,#10499,.F.);
#13606=ORIENTED_EDGE('',*,*,#10500,.T.);
#13607=ORIENTED_EDGE('',*,*,#10501,.T.);
#13608=ORIENTED_EDGE('',*,*,#10502,.F.);
#13609=ORIENTED_EDGE('',*,*,#10503,.F.);
#13610=ORIENTED_EDGE('',*,*,#10502,.T.);
#13611=ORIENTED_EDGE('',*,*,#10504,.T.);
#13612=ORIENTED_EDGE('',*,*,#10505,.F.);
#13613=ORIENTED_EDGE('',*,*,#10506,.F.);
#13614=ORIENTED_EDGE('',*,*,#10505,.T.);
#13615=ORIENTED_EDGE('',*,*,#10507,.T.);
#13616=ORIENTED_EDGE('',*,*,#10508,.F.);
#13617=ORIENTED_EDGE('',*,*,#10509,.F.);
#13618=ORIENTED_EDGE('',*,*,#10508,.T.);
#13619=ORIENTED_EDGE('',*,*,#10510,.T.);
#13620=ORIENTED_EDGE('',*,*,#10500,.F.);
#13621=ORIENTED_EDGE('',*,*,#10510,.F.);
#13622=ORIENTED_EDGE('',*,*,#10507,.F.);
#13623=ORIENTED_EDGE('',*,*,#10504,.F.);
#13624=ORIENTED_EDGE('',*,*,#10501,.F.);
#13625=ORIENTED_EDGE('',*,*,#10511,.F.);
#13626=ORIENTED_EDGE('',*,*,#10512,.T.);
#13627=ORIENTED_EDGE('',*,*,#10513,.T.);
#13628=ORIENTED_EDGE('',*,*,#10514,.F.);
#13629=ORIENTED_EDGE('',*,*,#10515,.F.);
#13630=ORIENTED_EDGE('',*,*,#10514,.T.);
#13631=ORIENTED_EDGE('',*,*,#10516,.T.);
#13632=ORIENTED_EDGE('',*,*,#10517,.F.);
#13633=ORIENTED_EDGE('',*,*,#10518,.F.);
#13634=ORIENTED_EDGE('',*,*,#10517,.T.);
#13635=ORIENTED_EDGE('',*,*,#10519,.T.);
#13636=ORIENTED_EDGE('',*,*,#10520,.F.);
#13637=ORIENTED_EDGE('',*,*,#10521,.F.);
#13638=ORIENTED_EDGE('',*,*,#10520,.T.);
#13639=ORIENTED_EDGE('',*,*,#10522,.T.);
#13640=ORIENTED_EDGE('',*,*,#10512,.F.);
#13641=ORIENTED_EDGE('',*,*,#10522,.F.);
#13642=ORIENTED_EDGE('',*,*,#10519,.F.);
#13643=ORIENTED_EDGE('',*,*,#10516,.F.);
#13644=ORIENTED_EDGE('',*,*,#10513,.F.);
#13645=ORIENTED_EDGE('',*,*,#10523,.F.);
#13646=ORIENTED_EDGE('',*,*,#10524,.T.);
#13647=ORIENTED_EDGE('',*,*,#10525,.T.);
#13648=ORIENTED_EDGE('',*,*,#10526,.F.);
#13649=ORIENTED_EDGE('',*,*,#10527,.F.);
#13650=ORIENTED_EDGE('',*,*,#10526,.T.);
#13651=ORIENTED_EDGE('',*,*,#10528,.T.);
#13652=ORIENTED_EDGE('',*,*,#10529,.F.);
#13653=ORIENTED_EDGE('',*,*,#10530,.F.);
#13654=ORIENTED_EDGE('',*,*,#10529,.T.);
#13655=ORIENTED_EDGE('',*,*,#10531,.T.);
#13656=ORIENTED_EDGE('',*,*,#10532,.F.);
#13657=ORIENTED_EDGE('',*,*,#10533,.F.);
#13658=ORIENTED_EDGE('',*,*,#10532,.T.);
#13659=ORIENTED_EDGE('',*,*,#10534,.T.);
#13660=ORIENTED_EDGE('',*,*,#10524,.F.);
#13661=ORIENTED_EDGE('',*,*,#10534,.F.);
#13662=ORIENTED_EDGE('',*,*,#10531,.F.);
#13663=ORIENTED_EDGE('',*,*,#10528,.F.);
#13664=ORIENTED_EDGE('',*,*,#10525,.F.);
#13665=ORIENTED_EDGE('',*,*,#10535,.F.);
#13666=ORIENTED_EDGE('',*,*,#10536,.T.);
#13667=ORIENTED_EDGE('',*,*,#10537,.T.);
#13668=ORIENTED_EDGE('',*,*,#10538,.F.);
#13669=ORIENTED_EDGE('',*,*,#10539,.F.);
#13670=ORIENTED_EDGE('',*,*,#10538,.T.);
#13671=ORIENTED_EDGE('',*,*,#10540,.T.);
#13672=ORIENTED_EDGE('',*,*,#10541,.F.);
#13673=ORIENTED_EDGE('',*,*,#10542,.F.);
#13674=ORIENTED_EDGE('',*,*,#10541,.T.);
#13675=ORIENTED_EDGE('',*,*,#10543,.T.);
#13676=ORIENTED_EDGE('',*,*,#10544,.F.);
#13677=ORIENTED_EDGE('',*,*,#10545,.F.);
#13678=ORIENTED_EDGE('',*,*,#10544,.T.);
#13679=ORIENTED_EDGE('',*,*,#10546,.T.);
#13680=ORIENTED_EDGE('',*,*,#10536,.F.);
#13681=ORIENTED_EDGE('',*,*,#10546,.F.);
#13682=ORIENTED_EDGE('',*,*,#10543,.F.);
#13683=ORIENTED_EDGE('',*,*,#10540,.F.);
#13684=ORIENTED_EDGE('',*,*,#10537,.F.);
#13685=ORIENTED_EDGE('',*,*,#10547,.F.);
#13686=ORIENTED_EDGE('',*,*,#10548,.T.);
#13687=ORIENTED_EDGE('',*,*,#10549,.T.);
#13688=ORIENTED_EDGE('',*,*,#10550,.F.);
#13689=ORIENTED_EDGE('',*,*,#10551,.F.);
#13690=ORIENTED_EDGE('',*,*,#10550,.T.);
#13691=ORIENTED_EDGE('',*,*,#10552,.T.);
#13692=ORIENTED_EDGE('',*,*,#10553,.F.);
#13693=ORIENTED_EDGE('',*,*,#10554,.F.);
#13694=ORIENTED_EDGE('',*,*,#10553,.T.);
#13695=ORIENTED_EDGE('',*,*,#10555,.T.);
#13696=ORIENTED_EDGE('',*,*,#10556,.F.);
#13697=ORIENTED_EDGE('',*,*,#10557,.F.);
#13698=ORIENTED_EDGE('',*,*,#10556,.T.);
#13699=ORIENTED_EDGE('',*,*,#10558,.T.);
#13700=ORIENTED_EDGE('',*,*,#10548,.F.);
#13701=ORIENTED_EDGE('',*,*,#10558,.F.);
#13702=ORIENTED_EDGE('',*,*,#10555,.F.);
#13703=ORIENTED_EDGE('',*,*,#10552,.F.);
#13704=ORIENTED_EDGE('',*,*,#10549,.F.);
#13705=ORIENTED_EDGE('',*,*,#10559,.F.);
#13706=ORIENTED_EDGE('',*,*,#10560,.T.);
#13707=ORIENTED_EDGE('',*,*,#10561,.T.);
#13708=ORIENTED_EDGE('',*,*,#10562,.F.);
#13709=ORIENTED_EDGE('',*,*,#10563,.F.);
#13710=ORIENTED_EDGE('',*,*,#10562,.T.);
#13711=ORIENTED_EDGE('',*,*,#10564,.T.);
#13712=ORIENTED_EDGE('',*,*,#10565,.F.);
#13713=ORIENTED_EDGE('',*,*,#10566,.F.);
#13714=ORIENTED_EDGE('',*,*,#10565,.T.);
#13715=ORIENTED_EDGE('',*,*,#10567,.T.);
#13716=ORIENTED_EDGE('',*,*,#10568,.F.);
#13717=ORIENTED_EDGE('',*,*,#10569,.F.);
#13718=ORIENTED_EDGE('',*,*,#10568,.T.);
#13719=ORIENTED_EDGE('',*,*,#10570,.T.);
#13720=ORIENTED_EDGE('',*,*,#10560,.F.);
#13721=ORIENTED_EDGE('',*,*,#10570,.F.);
#13722=ORIENTED_EDGE('',*,*,#10567,.F.);
#13723=ORIENTED_EDGE('',*,*,#10564,.F.);
#13724=ORIENTED_EDGE('',*,*,#10561,.F.);
#13725=ORIENTED_EDGE('',*,*,#10571,.F.);
#13726=ORIENTED_EDGE('',*,*,#10572,.T.);
#13727=ORIENTED_EDGE('',*,*,#10573,.T.);
#13728=ORIENTED_EDGE('',*,*,#10574,.F.);
#13729=ORIENTED_EDGE('',*,*,#10575,.F.);
#13730=ORIENTED_EDGE('',*,*,#10574,.T.);
#13731=ORIENTED_EDGE('',*,*,#10576,.T.);
#13732=ORIENTED_EDGE('',*,*,#10577,.F.);
#13733=ORIENTED_EDGE('',*,*,#10578,.F.);
#13734=ORIENTED_EDGE('',*,*,#10577,.T.);
#13735=ORIENTED_EDGE('',*,*,#10579,.T.);
#13736=ORIENTED_EDGE('',*,*,#10580,.F.);
#13737=ORIENTED_EDGE('',*,*,#10581,.F.);
#13738=ORIENTED_EDGE('',*,*,#10580,.T.);
#13739=ORIENTED_EDGE('',*,*,#10582,.T.);
#13740=ORIENTED_EDGE('',*,*,#10572,.F.);
#13741=ORIENTED_EDGE('',*,*,#10582,.F.);
#13742=ORIENTED_EDGE('',*,*,#10579,.F.);
#13743=ORIENTED_EDGE('',*,*,#10576,.F.);
#13744=ORIENTED_EDGE('',*,*,#10573,.F.);
#13745=ORIENTED_EDGE('',*,*,#10583,.F.);
#13746=ORIENTED_EDGE('',*,*,#10584,.T.);
#13747=ORIENTED_EDGE('',*,*,#10585,.T.);
#13748=ORIENTED_EDGE('',*,*,#10586,.F.);
#13749=ORIENTED_EDGE('',*,*,#10587,.F.);
#13750=ORIENTED_EDGE('',*,*,#10586,.T.);
#13751=ORIENTED_EDGE('',*,*,#10588,.T.);
#13752=ORIENTED_EDGE('',*,*,#10589,.F.);
#13753=ORIENTED_EDGE('',*,*,#10590,.F.);
#13754=ORIENTED_EDGE('',*,*,#10589,.T.);
#13755=ORIENTED_EDGE('',*,*,#10591,.T.);
#13756=ORIENTED_EDGE('',*,*,#10592,.F.);
#13757=ORIENTED_EDGE('',*,*,#10593,.F.);
#13758=ORIENTED_EDGE('',*,*,#10592,.T.);
#13759=ORIENTED_EDGE('',*,*,#10594,.T.);
#13760=ORIENTED_EDGE('',*,*,#10584,.F.);
#13761=ORIENTED_EDGE('',*,*,#10594,.F.);
#13762=ORIENTED_EDGE('',*,*,#10591,.F.);
#13763=ORIENTED_EDGE('',*,*,#10588,.F.);
#13764=ORIENTED_EDGE('',*,*,#10585,.F.);
#13765=ORIENTED_EDGE('',*,*,#10595,.F.);
#13766=ORIENTED_EDGE('',*,*,#10596,.T.);
#13767=ORIENTED_EDGE('',*,*,#10597,.T.);
#13768=ORIENTED_EDGE('',*,*,#10598,.F.);
#13769=ORIENTED_EDGE('',*,*,#10599,.F.);
#13770=ORIENTED_EDGE('',*,*,#10598,.T.);
#13771=ORIENTED_EDGE('',*,*,#10600,.T.);
#13772=ORIENTED_EDGE('',*,*,#10601,.F.);
#13773=ORIENTED_EDGE('',*,*,#10602,.F.);
#13774=ORIENTED_EDGE('',*,*,#10601,.T.);
#13775=ORIENTED_EDGE('',*,*,#10603,.T.);
#13776=ORIENTED_EDGE('',*,*,#10604,.F.);
#13777=ORIENTED_EDGE('',*,*,#10605,.F.);
#13778=ORIENTED_EDGE('',*,*,#10604,.T.);
#13779=ORIENTED_EDGE('',*,*,#10606,.T.);
#13780=ORIENTED_EDGE('',*,*,#10596,.F.);
#13781=ORIENTED_EDGE('',*,*,#10606,.F.);
#13782=ORIENTED_EDGE('',*,*,#10603,.F.);
#13783=ORIENTED_EDGE('',*,*,#10600,.F.);
#13784=ORIENTED_EDGE('',*,*,#10597,.F.);
#13785=ORIENTED_EDGE('',*,*,#10607,.F.);
#13786=ORIENTED_EDGE('',*,*,#10608,.T.);
#13787=ORIENTED_EDGE('',*,*,#10609,.F.);
#13788=ORIENTED_EDGE('',*,*,#10608,.F.);
#13789=ORIENTED_EDGE('',*,*,#10610,.F.);
#13790=ORIENTED_EDGE('',*,*,#10611,.T.);
#13791=ORIENTED_EDGE('',*,*,#10612,.F.);
#13792=ORIENTED_EDGE('',*,*,#10611,.F.);
#13793=ORIENTED_EDGE('',*,*,#10613,.T.);
#13794=ORIENTED_EDGE('',*,*,#10614,.T.);
#13795=ORIENTED_EDGE('',*,*,#10615,.F.);
#13796=ORIENTED_EDGE('',*,*,#10616,.F.);
#13797=ORIENTED_EDGE('',*,*,#10617,.T.);
#13798=ORIENTED_EDGE('',*,*,#10616,.T.);
#13799=ORIENTED_EDGE('',*,*,#10618,.F.);
#13800=ORIENTED_EDGE('',*,*,#10619,.F.);
#13801=ORIENTED_EDGE('',*,*,#10609,.T.);
#13802=ORIENTED_EDGE('',*,*,#10612,.T.);
#13803=ORIENTED_EDGE('',*,*,#10620,.T.);
#13804=ORIENTED_EDGE('',*,*,#10619,.T.);
#13805=ORIENTED_EDGE('',*,*,#10621,.F.);
#13806=ORIENTED_EDGE('',*,*,#10622,.F.);
#13807=ORIENTED_EDGE('',*,*,#10623,.T.);
#13808=ORIENTED_EDGE('',*,*,#10622,.T.);
#13809=ORIENTED_EDGE('',*,*,#10624,.F.);
#13810=ORIENTED_EDGE('',*,*,#10614,.F.);
#13811=ORIENTED_EDGE('',*,*,#10326,.T.);
#13812=ORIENTED_EDGE('',*,*,#10329,.T.);
#13813=ORIENTED_EDGE('',*,*,#10319,.T.);
#13814=ORIENTED_EDGE('',*,*,#10323,.T.);
#13815=ORIENTED_EDGE('',*,*,#10350,.T.);
#13816=ORIENTED_EDGE('',*,*,#10353,.T.);
#13817=ORIENTED_EDGE('',*,*,#10343,.T.);
#13818=ORIENTED_EDGE('',*,*,#10347,.T.);
#13819=ORIENTED_EDGE('',*,*,#10374,.T.);
#13820=ORIENTED_EDGE('',*,*,#10377,.T.);
#13821=ORIENTED_EDGE('',*,*,#10367,.T.);
#13822=ORIENTED_EDGE('',*,*,#10371,.T.);
#13823=ORIENTED_EDGE('',*,*,#10398,.T.);
#13824=ORIENTED_EDGE('',*,*,#10401,.T.);
#13825=ORIENTED_EDGE('',*,*,#10391,.T.);
#13826=ORIENTED_EDGE('',*,*,#10395,.T.);
#13827=ORIENTED_EDGE('',*,*,#10422,.T.);
#13828=ORIENTED_EDGE('',*,*,#10425,.T.);
#13829=ORIENTED_EDGE('',*,*,#10415,.T.);
#13830=ORIENTED_EDGE('',*,*,#10419,.T.);
#13831=ORIENTED_EDGE('',*,*,#10446,.T.);
#13832=ORIENTED_EDGE('',*,*,#10449,.T.);
#13833=ORIENTED_EDGE('',*,*,#10439,.T.);
#13834=ORIENTED_EDGE('',*,*,#10443,.T.);
#13835=ORIENTED_EDGE('',*,*,#10470,.T.);
#13836=ORIENTED_EDGE('',*,*,#10473,.T.);
#13837=ORIENTED_EDGE('',*,*,#10463,.T.);
#13838=ORIENTED_EDGE('',*,*,#10467,.T.);
#13839=ORIENTED_EDGE('',*,*,#10494,.T.);
#13840=ORIENTED_EDGE('',*,*,#10497,.T.);
#13841=ORIENTED_EDGE('',*,*,#10487,.T.);
#13842=ORIENTED_EDGE('',*,*,#10491,.T.);
#13843=ORIENTED_EDGE('',*,*,#10518,.T.);
#13844=ORIENTED_EDGE('',*,*,#10521,.T.);
#13845=ORIENTED_EDGE('',*,*,#10511,.T.);
#13846=ORIENTED_EDGE('',*,*,#10515,.T.);
#13847=ORIENTED_EDGE('',*,*,#10542,.T.);
#13848=ORIENTED_EDGE('',*,*,#10545,.T.);
#13849=ORIENTED_EDGE('',*,*,#10535,.T.);
#13850=ORIENTED_EDGE('',*,*,#10539,.T.);
#13851=ORIENTED_EDGE('',*,*,#10554,.T.);
#13852=ORIENTED_EDGE('',*,*,#10557,.T.);
#13853=ORIENTED_EDGE('',*,*,#10547,.T.);
#13854=ORIENTED_EDGE('',*,*,#10551,.T.);
#13855=ORIENTED_EDGE('',*,*,#10566,.T.);
#13856=ORIENTED_EDGE('',*,*,#10569,.T.);
#13857=ORIENTED_EDGE('',*,*,#10559,.T.);
#13858=ORIENTED_EDGE('',*,*,#10563,.T.);
#13859=ORIENTED_EDGE('',*,*,#10578,.T.);
#13860=ORIENTED_EDGE('',*,*,#10581,.T.);
#13861=ORIENTED_EDGE('',*,*,#10571,.T.);
#13862=ORIENTED_EDGE('',*,*,#10575,.T.);
#13863=ORIENTED_EDGE('',*,*,#10590,.T.);
#13864=ORIENTED_EDGE('',*,*,#10593,.T.);
#13865=ORIENTED_EDGE('',*,*,#10583,.T.);
#13866=ORIENTED_EDGE('',*,*,#10587,.T.);
#13867=ORIENTED_EDGE('',*,*,#10602,.T.);
#13868=ORIENTED_EDGE('',*,*,#10605,.T.);
#13869=ORIENTED_EDGE('',*,*,#10595,.T.);
#13870=ORIENTED_EDGE('',*,*,#10599,.T.);
#13871=ORIENTED_EDGE('',*,*,#10607,.T.);
#13872=ORIENTED_EDGE('',*,*,#10610,.T.);
#13873=ORIENTED_EDGE('',*,*,#10530,.T.);
#13874=ORIENTED_EDGE('',*,*,#10533,.T.);
#13875=ORIENTED_EDGE('',*,*,#10523,.T.);
#13876=ORIENTED_EDGE('',*,*,#10527,.T.);
#13877=ORIENTED_EDGE('',*,*,#10506,.T.);
#13878=ORIENTED_EDGE('',*,*,#10509,.T.);
#13879=ORIENTED_EDGE('',*,*,#10499,.T.);
#13880=ORIENTED_EDGE('',*,*,#10503,.T.);
#13881=ORIENTED_EDGE('',*,*,#10482,.T.);
#13882=ORIENTED_EDGE('',*,*,#10485,.T.);
#13883=ORIENTED_EDGE('',*,*,#10475,.T.);
#13884=ORIENTED_EDGE('',*,*,#10479,.T.);
#13885=ORIENTED_EDGE('',*,*,#10458,.T.);
#13886=ORIENTED_EDGE('',*,*,#10461,.T.);
#13887=ORIENTED_EDGE('',*,*,#10451,.T.);
#13888=ORIENTED_EDGE('',*,*,#10455,.T.);
#13889=ORIENTED_EDGE('',*,*,#10434,.T.);
#13890=ORIENTED_EDGE('',*,*,#10437,.T.);
#13891=ORIENTED_EDGE('',*,*,#10427,.T.);
#13892=ORIENTED_EDGE('',*,*,#10431,.T.);
#13893=ORIENTED_EDGE('',*,*,#10410,.T.);
#13894=ORIENTED_EDGE('',*,*,#10413,.T.);
#13895=ORIENTED_EDGE('',*,*,#10403,.T.);
#13896=ORIENTED_EDGE('',*,*,#10407,.T.);
#13897=ORIENTED_EDGE('',*,*,#10386,.T.);
#13898=ORIENTED_EDGE('',*,*,#10389,.T.);
#13899=ORIENTED_EDGE('',*,*,#10379,.T.);
#13900=ORIENTED_EDGE('',*,*,#10383,.T.);
#13901=ORIENTED_EDGE('',*,*,#10362,.T.);
#13902=ORIENTED_EDGE('',*,*,#10365,.T.);
#13903=ORIENTED_EDGE('',*,*,#10355,.T.);
#13904=ORIENTED_EDGE('',*,*,#10359,.T.);
#13905=ORIENTED_EDGE('',*,*,#10338,.T.);
#13906=ORIENTED_EDGE('',*,*,#10341,.T.);
#13907=ORIENTED_EDGE('',*,*,#10331,.T.);
#13908=ORIENTED_EDGE('',*,*,#10335,.T.);
#13909=ORIENTED_EDGE('',*,*,#10314,.T.);
#13910=ORIENTED_EDGE('',*,*,#10317,.T.);
#13911=ORIENTED_EDGE('',*,*,#10307,.T.);
#13912=ORIENTED_EDGE('',*,*,#10311,.T.);
#13913=ORIENTED_EDGE('',*,*,#10624,.T.);
#13914=ORIENTED_EDGE('',*,*,#10621,.T.);
#13915=ORIENTED_EDGE('',*,*,#10618,.T.);
#13916=ORIENTED_EDGE('',*,*,#10615,.T.);
#13917=ORIENTED_EDGE('',*,*,#10623,.F.);
#13918=ORIENTED_EDGE('',*,*,#10613,.F.);
#13919=ORIENTED_EDGE('',*,*,#10617,.F.);
#13920=ORIENTED_EDGE('',*,*,#10620,.F.);
#13921=ORIENTED_EDGE('',*,*,#10625,.T.);
#13922=ORIENTED_EDGE('',*,*,#10626,.T.);
#13923=ORIENTED_EDGE('',*,*,#10627,.T.);
#13924=ORIENTED_EDGE('',*,*,#10626,.F.);
#13925=ORIENTED_EDGE('',*,*,#10628,.F.);
#13926=ORIENTED_EDGE('',*,*,#10629,.T.);
#13927=ORIENTED_EDGE('',*,*,#10625,.F.);
#13928=ORIENTED_EDGE('',*,*,#10629,.F.);
#13929=ORIENTED_EDGE('',*,*,#10627,.F.);
#13930=ORIENTED_EDGE('',*,*,#10630,.T.);
#13931=ORIENTED_EDGE('',*,*,#10631,.T.);
#13932=ORIENTED_EDGE('',*,*,#10628,.T.);
#13933=ORIENTED_EDGE('',*,*,#10631,.F.);
#13934=ORIENTED_EDGE('',*,*,#10630,.F.);
#13935=ORIENTED_EDGE('',*,*,#10632,.F.);
#13936=ORIENTED_EDGE('',*,*,#10633,.F.);
#13937=ORIENTED_EDGE('',*,*,#10634,.F.);
#13938=ORIENTED_EDGE('',*,*,#10635,.F.);
#13939=ORIENTED_EDGE('',*,*,#10636,.F.);
#13940=ORIENTED_EDGE('',*,*,#10633,.T.);
#13941=ORIENTED_EDGE('',*,*,#10637,.F.);
#13942=ORIENTED_EDGE('',*,*,#10638,.T.);
#13943=ORIENTED_EDGE('',*,*,#10639,.F.);
#13944=ORIENTED_EDGE('',*,*,#10640,.F.);
#13945=ORIENTED_EDGE('',*,*,#10641,.F.);
#13946=ORIENTED_EDGE('',*,*,#10638,.F.);
#13947=ORIENTED_EDGE('',*,*,#10642,.T.);
#13948=ORIENTED_EDGE('',*,*,#10643,.F.);
#13949=ORIENTED_EDGE('',*,*,#10644,.T.);
#13950=ORIENTED_EDGE('',*,*,#10645,.F.);
#13951=ORIENTED_EDGE('',*,*,#10646,.T.);
#13952=ORIENTED_EDGE('',*,*,#10635,.T.);
#13953=ORIENTED_EDGE('',*,*,#10647,.T.);
#13954=ORIENTED_EDGE('',*,*,#10634,.T.);
#13955=ORIENTED_EDGE('',*,*,#10632,.T.);
#13956=ORIENTED_EDGE('',*,*,#10636,.T.);
#13957=ORIENTED_EDGE('',*,*,#10646,.F.);
#13958=ORIENTED_EDGE('',*,*,#10648,.F.);
#13959=ORIENTED_EDGE('',*,*,#10649,.T.);
#13960=ORIENTED_EDGE('',*,*,#10650,.F.);
#13961=ORIENTED_EDGE('',*,*,#10642,.F.);
#13962=ORIENTED_EDGE('',*,*,#10651,.T.);
#13963=ORIENTED_EDGE('',*,*,#10652,.T.);
#13964=ORIENTED_EDGE('',*,*,#10653,.F.);
#13965=ORIENTED_EDGE('',*,*,#10654,.F.);
#13966=ORIENTED_EDGE('',*,*,#10640,.T.);
#13967=ORIENTED_EDGE('',*,*,#10655,.F.);
#13968=ORIENTED_EDGE('',*,*,#10656,.F.);
#13969=ORIENTED_EDGE('',*,*,#10657,.T.);
#13970=ORIENTED_EDGE('',*,*,#10658,.F.);
#13971=ORIENTED_EDGE('',*,*,#10659,.T.);
#13972=ORIENTED_EDGE('',*,*,#10660,.F.);
#13973=ORIENTED_EDGE('',*,*,#10659,.F.);
#13974=ORIENTED_EDGE('',*,*,#10651,.F.);
#13975=ORIENTED_EDGE('',*,*,#10661,.T.);
#13976=ORIENTED_EDGE('',*,*,#10662,.F.);
#13977=ORIENTED_EDGE('',*,*,#10661,.F.);
#13978=ORIENTED_EDGE('',*,*,#10663,.F.);
#13979=ORIENTED_EDGE('',*,*,#10664,.T.);
#13980=ORIENTED_EDGE('',*,*,#10647,.F.);
#13981=ORIENTED_EDGE('',*,*,#10664,.F.);
#13982=ORIENTED_EDGE('',*,*,#10665,.F.);
#13983=ORIENTED_EDGE('',*,*,#10666,.T.);
#13984=ORIENTED_EDGE('',*,*,#10657,.F.);
#13985=ORIENTED_EDGE('',*,*,#10666,.F.);
#13986=ORIENTED_EDGE('',*,*,#10667,.F.);
#13987=ORIENTED_EDGE('',*,*,#10668,.T.);
#13988=ORIENTED_EDGE('',*,*,#10669,.F.);
#13989=ORIENTED_EDGE('',*,*,#10668,.F.);
#13990=ORIENTED_EDGE('',*,*,#10645,.T.);
#13991=ORIENTED_EDGE('',*,*,#10670,.T.);
#13992=ORIENTED_EDGE('',*,*,#10671,.T.);
#13993=ORIENTED_EDGE('',*,*,#10672,.T.);
#13994=ORIENTED_EDGE('',*,*,#10656,.T.);
#13995=ORIENTED_EDGE('',*,*,#10673,.T.);
#13996=ORIENTED_EDGE('',*,*,#10674,.T.);
#13997=ORIENTED_EDGE('',*,*,#10675,.T.);
#13998=ORIENTED_EDGE('',*,*,#10676,.T.);
#13999=ORIENTED_EDGE('',*,*,#10677,.T.);
#14000=ORIENTED_EDGE('',*,*,#10678,.T.);
#14001=ORIENTED_EDGE('',*,*,#10648,.T.);
#14002=ORIENTED_EDGE('',*,*,#10667,.T.);
#14003=ORIENTED_EDGE('',*,*,#10644,.F.);
#14004=ORIENTED_EDGE('',*,*,#10679,.F.);
#14005=ORIENTED_EDGE('',*,*,#10680,.F.);
#14006=ORIENTED_EDGE('',*,*,#10670,.F.);
#14007=ORIENTED_EDGE('',*,*,#10680,.T.);
#14008=ORIENTED_EDGE('',*,*,#10681,.F.);
#14009=ORIENTED_EDGE('',*,*,#10682,.F.);
#14010=ORIENTED_EDGE('',*,*,#10671,.F.);
#14011=ORIENTED_EDGE('',*,*,#10663,.T.);
#14012=ORIENTED_EDGE('',*,*,#10665,.T.);
#14013=ORIENTED_EDGE('',*,*,#10682,.T.);
#14014=ORIENTED_EDGE('',*,*,#10683,.F.);
#14015=ORIENTED_EDGE('',*,*,#10652,.F.);
#14016=ORIENTED_EDGE('',*,*,#10672,.F.);
#14017=ORIENTED_EDGE('',*,*,#10637,.T.);
#14018=ORIENTED_EDGE('',*,*,#10654,.T.);
#14019=ORIENTED_EDGE('',*,*,#10684,.F.);
#14020=ORIENTED_EDGE('',*,*,#10685,.F.);
#14021=ORIENTED_EDGE('',*,*,#10673,.F.);
#14022=ORIENTED_EDGE('',*,*,#10655,.T.);
#14023=ORIENTED_EDGE('',*,*,#10639,.T.);
#14024=ORIENTED_EDGE('',*,*,#10641,.T.);
#14025=ORIENTED_EDGE('',*,*,#10660,.T.);
#14026=ORIENTED_EDGE('',*,*,#10685,.T.);
#14027=ORIENTED_EDGE('',*,*,#10686,.F.);
#14028=ORIENTED_EDGE('',*,*,#10687,.F.);
#14029=ORIENTED_EDGE('',*,*,#10674,.F.);
#14030=ORIENTED_EDGE('',*,*,#10687,.T.);
#14031=ORIENTED_EDGE('',*,*,#10688,.F.);
#14032=ORIENTED_EDGE('',*,*,#10689,.F.);
#14033=ORIENTED_EDGE('',*,*,#10675,.F.);
#14034=ORIENTED_EDGE('',*,*,#10658,.T.);
#14035=ORIENTED_EDGE('',*,*,#10689,.T.);
#14036=ORIENTED_EDGE('',*,*,#10690,.F.);
#14037=ORIENTED_EDGE('',*,*,#10691,.F.);
#14038=ORIENTED_EDGE('',*,*,#10676,.F.);
#14039=ORIENTED_EDGE('',*,*,#10691,.T.);
#14040=ORIENTED_EDGE('',*,*,#10692,.F.);
#14041=ORIENTED_EDGE('',*,*,#10693,.F.);
#14042=ORIENTED_EDGE('',*,*,#10677,.F.);
#14043=ORIENTED_EDGE('',*,*,#10662,.T.);
#14044=ORIENTED_EDGE('',*,*,#10693,.T.);
#14045=ORIENTED_EDGE('',*,*,#10694,.F.);
#14046=ORIENTED_EDGE('',*,*,#10649,.F.);
#14047=ORIENTED_EDGE('',*,*,#10678,.F.);
#14048=ORIENTED_EDGE('',*,*,#10643,.T.);
#14049=ORIENTED_EDGE('',*,*,#10650,.T.);
#14050=ORIENTED_EDGE('',*,*,#10694,.T.);
#14051=ORIENTED_EDGE('',*,*,#10692,.T.);
#14052=ORIENTED_EDGE('',*,*,#10690,.T.);
#14053=ORIENTED_EDGE('',*,*,#10688,.T.);
#14054=ORIENTED_EDGE('',*,*,#10686,.T.);
#14055=ORIENTED_EDGE('',*,*,#10684,.T.);
#14056=ORIENTED_EDGE('',*,*,#10653,.T.);
#14057=ORIENTED_EDGE('',*,*,#10683,.T.);
#14058=ORIENTED_EDGE('',*,*,#10681,.T.);
#14059=ORIENTED_EDGE('',*,*,#10679,.T.);
#14060=ORIENTED_EDGE('',*,*,#10669,.T.);
#14061=ORIENTED_EDGE('',*,*,#10695,.T.);
#14062=ORIENTED_EDGE('',*,*,#10696,.T.);
#14063=ORIENTED_EDGE('',*,*,#10697,.T.);
#14064=ORIENTED_EDGE('',*,*,#10698,.F.);
#14065=ORIENTED_EDGE('',*,*,#10699,.T.);
#14066=ORIENTED_EDGE('',*,*,#10700,.T.);
#14067=ORIENTED_EDGE('',*,*,#10701,.T.);
#14068=ORIENTED_EDGE('',*,*,#10696,.F.);
#14069=ORIENTED_EDGE('',*,*,#10702,.T.);
#14070=ORIENTED_EDGE('',*,*,#10703,.T.);
#14071=ORIENTED_EDGE('',*,*,#10704,.T.);
#14072=ORIENTED_EDGE('',*,*,#10700,.F.);
#14073=ORIENTED_EDGE('',*,*,#10705,.T.);
#14074=ORIENTED_EDGE('',*,*,#10706,.T.);
#14075=ORIENTED_EDGE('',*,*,#10707,.T.);
#14076=ORIENTED_EDGE('',*,*,#10703,.F.);
#14077=ORIENTED_EDGE('',*,*,#10708,.T.);
#14078=ORIENTED_EDGE('',*,*,#10709,.T.);
#14079=ORIENTED_EDGE('',*,*,#10710,.T.);
#14080=ORIENTED_EDGE('',*,*,#10706,.F.);
#14081=ORIENTED_EDGE('',*,*,#10711,.T.);
#14082=ORIENTED_EDGE('',*,*,#10698,.T.);
#14083=ORIENTED_EDGE('',*,*,#10712,.T.);
#14084=ORIENTED_EDGE('',*,*,#10709,.F.);
#14085=ORIENTED_EDGE('',*,*,#10711,.F.);
#14086=ORIENTED_EDGE('',*,*,#10708,.F.);
#14087=ORIENTED_EDGE('',*,*,#10705,.F.);
#14088=ORIENTED_EDGE('',*,*,#10702,.F.);
#14089=ORIENTED_EDGE('',*,*,#10699,.F.);
#14090=ORIENTED_EDGE('',*,*,#10695,.F.);
#14091=ORIENTED_EDGE('',*,*,#10712,.F.);
#14092=ORIENTED_EDGE('',*,*,#10697,.F.);
#14093=ORIENTED_EDGE('',*,*,#10701,.F.);
#14094=ORIENTED_EDGE('',*,*,#10704,.F.);
#14095=ORIENTED_EDGE('',*,*,#10707,.F.);
#14096=ORIENTED_EDGE('',*,*,#10710,.F.);
#14097=ORIENTED_EDGE('',*,*,#10713,.F.);
#14098=ORIENTED_EDGE('',*,*,#10714,.F.);
#14099=ORIENTED_EDGE('',*,*,#10715,.F.);
#14100=ORIENTED_EDGE('',*,*,#10716,.T.);
#14101=ORIENTED_EDGE('',*,*,#10714,.T.);
#14102=ORIENTED_EDGE('',*,*,#10716,.F.);
#14103=ORIENTED_EDGE('',*,*,#10717,.F.);
#14104=ORIENTED_EDGE('',*,*,#10718,.T.);
#14105=ORIENTED_EDGE('',*,*,#10715,.T.);
#14106=ORIENTED_EDGE('',*,*,#10718,.F.);
#14107=ORIENTED_EDGE('',*,*,#10719,.F.);
#14108=ORIENTED_EDGE('',*,*,#10720,.T.);
#14109=ORIENTED_EDGE('',*,*,#10717,.T.);
#14110=ORIENTED_EDGE('',*,*,#10720,.F.);
#14111=ORIENTED_EDGE('',*,*,#10719,.T.);
#14112=ORIENTED_EDGE('',*,*,#10721,.F.);
#14113=ORIENTED_EDGE('',*,*,#10722,.F.);
#14114=ORIENTED_EDGE('',*,*,#10723,.T.);
#14115=ORIENTED_EDGE('',*,*,#10721,.T.);
#14116=ORIENTED_EDGE('',*,*,#10723,.F.);
#14117=ORIENTED_EDGE('',*,*,#10713,.T.);
#14118=ORIENTED_EDGE('',*,*,#10724,.T.);
#14119=ORIENTED_EDGE('',*,*,#10722,.T.);
#14120=ORIENTED_EDGE('',*,*,#10724,.F.);
#14121=ORIENTED_EDGE('',*,*,#10725,.F.);
#14122=ORIENTED_EDGE('',*,*,#10726,.F.);
#14123=ORIENTED_EDGE('',*,*,#10727,.T.);
#14124=ORIENTED_EDGE('',*,*,#10728,.F.);
#14125=ORIENTED_EDGE('',*,*,#10729,.F.);
#14126=ORIENTED_EDGE('',*,*,#10727,.F.);
#14127=ORIENTED_EDGE('',*,*,#10728,.T.);
#14128=ORIENTED_EDGE('',*,*,#10729,.T.);
#14129=ORIENTED_EDGE('',*,*,#10730,.T.);
#14130=ORIENTED_EDGE('',*,*,#10731,.T.);
#14131=ORIENTED_EDGE('',*,*,#10730,.F.);
#14132=ORIENTED_EDGE('',*,*,#10732,.T.);
#14133=ORIENTED_EDGE('',*,*,#10733,.T.);
#14134=ORIENTED_EDGE('',*,*,#10734,.F.);
#14135=ORIENTED_EDGE('',*,*,#10733,.F.);
#14136=ORIENTED_EDGE('',*,*,#10734,.T.);
#14137=ORIENTED_EDGE('',*,*,#10735,.T.);
#14138=ORIENTED_EDGE('',*,*,#10736,.F.);
#14139=ORIENTED_EDGE('',*,*,#10735,.F.);
#14140=ORIENTED_EDGE('',*,*,#10731,.F.);
#14141=ORIENTED_EDGE('',*,*,#10736,.T.);
#14142=ORIENTED_EDGE('',*,*,#10737,.F.);
#14143=ORIENTED_EDGE('',*,*,#10738,.T.);
#14144=ORIENTED_EDGE('',*,*,#10725,.T.);
#14145=ORIENTED_EDGE('',*,*,#10726,.T.);
#14146=ORIENTED_EDGE('',*,*,#10738,.F.);
#14147=ORIENTED_EDGE('',*,*,#10737,.T.);
#14148=ORIENTED_EDGE('',*,*,#10739,.F.);
#14149=ORIENTED_EDGE('',*,*,#10739,.T.);
#14150=ORIENTED_EDGE('',*,*,#10740,.T.);
#14151=ORIENTED_EDGE('',*,*,#10732,.F.);
#14152=ORIENTED_EDGE('',*,*,#10740,.F.);
#14153=ORIENTED_EDGE('',*,*,#10741,.F.);
#14154=ORIENTED_EDGE('',*,*,#10742,.F.);
#14155=ORIENTED_EDGE('',*,*,#10743,.T.);
#14156=ORIENTED_EDGE('',*,*,#10744,.F.);
#14157=ORIENTED_EDGE('',*,*,#10745,.F.);
#14158=ORIENTED_EDGE('',*,*,#10743,.F.);
#14159=ORIENTED_EDGE('',*,*,#10746,.T.);
#14160=ORIENTED_EDGE('',*,*,#10747,.T.);
#14161=ORIENTED_EDGE('',*,*,#10744,.T.);
#14162=ORIENTED_EDGE('',*,*,#10745,.T.);
#14163=ORIENTED_EDGE('',*,*,#10747,.F.);
#14164=ORIENTED_EDGE('',*,*,#10748,.F.);
#14165=ORIENTED_EDGE('',*,*,#10749,.T.);
#14166=ORIENTED_EDGE('',*,*,#10750,.F.);
#14167=ORIENTED_EDGE('',*,*,#10751,.T.);
#14168=ORIENTED_EDGE('',*,*,#10748,.T.);
#14169=ORIENTED_EDGE('',*,*,#10751,.F.);
#14170=ORIENTED_EDGE('',*,*,#10752,.F.);
#14171=ORIENTED_EDGE('',*,*,#10753,.T.);
#14172=ORIENTED_EDGE('',*,*,#10750,.T.);
#14173=ORIENTED_EDGE('',*,*,#10753,.F.);
#14174=ORIENTED_EDGE('',*,*,#10754,.F.);
#14175=ORIENTED_EDGE('',*,*,#10755,.T.);
#14176=ORIENTED_EDGE('',*,*,#10752,.T.);
#14177=ORIENTED_EDGE('',*,*,#10755,.F.);
#14178=ORIENTED_EDGE('',*,*,#10754,.T.);
#14179=ORIENTED_EDGE('',*,*,#10746,.F.);
#14180=ORIENTED_EDGE('',*,*,#10741,.T.);
#14181=ORIENTED_EDGE('',*,*,#10742,.T.);
#14182=ORIENTED_EDGE('',*,*,#10756,.T.);
#14183=ORIENTED_EDGE('',*,*,#10749,.F.);
#14184=ORIENTED_EDGE('',*,*,#10756,.F.);
#14185=ORIENTED_EDGE('',*,*,#10757,.T.);
#14186=ORIENTED_EDGE('',*,*,#10757,.F.);
#14187=ORIENTED_EDGE('',*,*,#10758,.T.);
#14188=ORIENTED_EDGE('',*,*,#10758,.F.);
#14189=ORIENTED_EDGE('',*,*,#10759,.T.);
#14190=ORIENTED_EDGE('',*,*,#10759,.F.);
#14191=ORIENTED_EDGE('',*,*,#10760,.T.);
#14192=ORIENTED_EDGE('',*,*,#10760,.F.);
#14193=ORIENTED_EDGE('',*,*,#10761,.T.);
#14194=ORIENTED_EDGE('',*,*,#10761,.F.);
#14195=ORIENTED_EDGE('',*,*,#10762,.T.);
#14196=ORIENTED_EDGE('',*,*,#10762,.F.);
#14197=ORIENTED_EDGE('',*,*,#10763,.T.);
#14198=ORIENTED_EDGE('',*,*,#10763,.F.);
#14199=ORIENTED_EDGE('',*,*,#10764,.F.);
#14200=ORIENTED_EDGE('',*,*,#10765,.F.);
#14201=ORIENTED_EDGE('',*,*,#10766,.F.);
#14202=ORIENTED_EDGE('',*,*,#10767,.F.);
#14203=ORIENTED_EDGE('',*,*,#10766,.T.);
#14204=ORIENTED_EDGE('',*,*,#10768,.F.);
#14205=ORIENTED_EDGE('',*,*,#10769,.T.);
#14206=ORIENTED_EDGE('',*,*,#10770,.F.);
#14207=ORIENTED_EDGE('',*,*,#10771,.T.);
#14208=ORIENTED_EDGE('',*,*,#10772,.F.);
#14209=ORIENTED_EDGE('',*,*,#10773,.T.);
#14210=ORIENTED_EDGE('',*,*,#10774,.F.);
#14211=ORIENTED_EDGE('',*,*,#10773,.F.);
#14212=ORIENTED_EDGE('',*,*,#10775,.F.);
#14213=ORIENTED_EDGE('',*,*,#10776,.T.);
#14214=ORIENTED_EDGE('',*,*,#10777,.F.);
#14215=ORIENTED_EDGE('',*,*,#10778,.T.);
#14216=ORIENTED_EDGE('',*,*,#10779,.F.);
#14217=ORIENTED_EDGE('',*,*,#10780,.T.);
#14218=ORIENTED_EDGE('',*,*,#10781,.F.);
#14219=ORIENTED_EDGE('',*,*,#10782,.T.);
#14220=ORIENTED_EDGE('',*,*,#10783,.F.);
#14221=ORIENTED_EDGE('',*,*,#10765,.T.);
#14222=ORIENTED_EDGE('',*,*,#10784,.T.);
#14223=ORIENTED_EDGE('',*,*,#10785,.T.);
#14224=ORIENTED_EDGE('',*,*,#10768,.T.);
#14225=ORIENTED_EDGE('',*,*,#10786,.F.);
#14226=ORIENTED_EDGE('',*,*,#10787,.F.);
#14227=ORIENTED_EDGE('',*,*,#10769,.F.);
#14228=ORIENTED_EDGE('',*,*,#10785,.F.);
#14229=ORIENTED_EDGE('',*,*,#10787,.T.);
#14230=ORIENTED_EDGE('',*,*,#10788,.T.);
#14231=ORIENTED_EDGE('',*,*,#10789,.T.);
#14232=ORIENTED_EDGE('',*,*,#10770,.T.);
#14233=ORIENTED_EDGE('',*,*,#10790,.F.);
#14234=ORIENTED_EDGE('',*,*,#10791,.F.);
#14235=ORIENTED_EDGE('',*,*,#10771,.F.);
#14236=ORIENTED_EDGE('',*,*,#10789,.F.);
#14237=ORIENTED_EDGE('',*,*,#10791,.T.);
#14238=ORIENTED_EDGE('',*,*,#10792,.T.);
#14239=ORIENTED_EDGE('',*,*,#10793,.T.);
#14240=ORIENTED_EDGE('',*,*,#10794,.T.);
#14241=ORIENTED_EDGE('',*,*,#10775,.T.);
#14242=ORIENTED_EDGE('',*,*,#10772,.T.);
#14243=ORIENTED_EDGE('',*,*,#10795,.F.);
#14244=ORIENTED_EDGE('',*,*,#10796,.F.);
#14245=ORIENTED_EDGE('',*,*,#10776,.F.);
#14246=ORIENTED_EDGE('',*,*,#10794,.F.);
#14247=ORIENTED_EDGE('',*,*,#10796,.T.);
#14248=ORIENTED_EDGE('',*,*,#10797,.T.);
#14249=ORIENTED_EDGE('',*,*,#10798,.T.);
#14250=ORIENTED_EDGE('',*,*,#10777,.T.);
#14251=ORIENTED_EDGE('',*,*,#10799,.F.);
#14252=ORIENTED_EDGE('',*,*,#10800,.F.);
#14253=ORIENTED_EDGE('',*,*,#10778,.F.);
#14254=ORIENTED_EDGE('',*,*,#10798,.F.);
#14255=ORIENTED_EDGE('',*,*,#10800,.T.);
#14256=ORIENTED_EDGE('',*,*,#10801,.T.);
#14257=ORIENTED_EDGE('',*,*,#10802,.T.);
#14258=ORIENTED_EDGE('',*,*,#10779,.T.);
#14259=ORIENTED_EDGE('',*,*,#10780,.F.);
#14260=ORIENTED_EDGE('',*,*,#10802,.F.);
#14261=ORIENTED_EDGE('',*,*,#10803,.F.);
#14262=ORIENTED_EDGE('',*,*,#10804,.F.);
#14263=ORIENTED_EDGE('',*,*,#10805,.F.);
#14264=ORIENTED_EDGE('',*,*,#10806,.T.);
#14265=ORIENTED_EDGE('',*,*,#10792,.F.);
#14266=ORIENTED_EDGE('',*,*,#10790,.T.);
#14267=ORIENTED_EDGE('',*,*,#10788,.F.);
#14268=ORIENTED_EDGE('',*,*,#10786,.T.);
#14269=ORIENTED_EDGE('',*,*,#10784,.F.);
#14270=ORIENTED_EDGE('',*,*,#10764,.T.);
#14271=ORIENTED_EDGE('',*,*,#10807,.F.);
#14272=ORIENTED_EDGE('',*,*,#10808,.T.);
#14273=ORIENTED_EDGE('',*,*,#10809,.F.);
#14274=ORIENTED_EDGE('',*,*,#10803,.T.);
#14275=ORIENTED_EDGE('',*,*,#10801,.F.);
#14276=ORIENTED_EDGE('',*,*,#10799,.T.);
#14277=ORIENTED_EDGE('',*,*,#10797,.F.);
#14278=ORIENTED_EDGE('',*,*,#10795,.T.);
#14279=ORIENTED_EDGE('',*,*,#10793,.F.);
#14280=ORIENTED_EDGE('',*,*,#10806,.F.);
#14281=ORIENTED_EDGE('',*,*,#10767,.T.);
#14282=ORIENTED_EDGE('',*,*,#10783,.T.);
#14283=ORIENTED_EDGE('',*,*,#10810,.T.);
#14284=ORIENTED_EDGE('',*,*,#10807,.T.);
#14285=ORIENTED_EDGE('',*,*,#10782,.F.);
#14286=ORIENTED_EDGE('',*,*,#10811,.F.);
#14287=ORIENTED_EDGE('',*,*,#10808,.F.);
#14288=ORIENTED_EDGE('',*,*,#10810,.F.);
#14289=ORIENTED_EDGE('',*,*,#10774,.T.);
#14290=ORIENTED_EDGE('',*,*,#10805,.T.);
#14291=ORIENTED_EDGE('',*,*,#10804,.T.);
#14292=ORIENTED_EDGE('',*,*,#10809,.T.);
#14293=ORIENTED_EDGE('',*,*,#10811,.T.);
#14294=ORIENTED_EDGE('',*,*,#10781,.T.);
#14295=ORIENTED_EDGE('',*,*,#10812,.F.);
#14296=ORIENTED_EDGE('',*,*,#10813,.T.);
#14297=ORIENTED_EDGE('',*,*,#10814,.F.);
#14298=ORIENTED_EDGE('',*,*,#10815,.T.);
#14299=ORIENTED_EDGE('',*,*,#10812,.T.);
#14300=ORIENTED_EDGE('',*,*,#10815,.F.);
#14301=ORIENTED_EDGE('',*,*,#10814,.T.);
#14302=ORIENTED_EDGE('',*,*,#10816,.F.);
#14303=ORIENTED_EDGE('',*,*,#10816,.T.);
#14304=ORIENTED_EDGE('',*,*,#10817,.T.);
#14305=ORIENTED_EDGE('',*,*,#10813,.F.);
#14306=ORIENTED_EDGE('',*,*,#10817,.F.);
#14307=ORIENTED_EDGE('',*,*,#10818,.F.);
#14308=ORIENTED_EDGE('',*,*,#10819,.T.);
#14309=ORIENTED_EDGE('',*,*,#10820,.F.);
#14310=ORIENTED_EDGE('',*,*,#10821,.T.);
#14311=ORIENTED_EDGE('',*,*,#10818,.T.);
#14312=ORIENTED_EDGE('',*,*,#10821,.F.);
#14313=ORIENTED_EDGE('',*,*,#10820,.T.);
#14314=ORIENTED_EDGE('',*,*,#10822,.F.);
#14315=ORIENTED_EDGE('',*,*,#10822,.T.);
#14316=ORIENTED_EDGE('',*,*,#10823,.T.);
#14317=ORIENTED_EDGE('',*,*,#10819,.F.);
#14318=ORIENTED_EDGE('',*,*,#10823,.F.);
#14319=ORIENTED_EDGE('',*,*,#10824,.F.);
#14320=ORIENTED_EDGE('',*,*,#10825,.F.);
#14321=ORIENTED_EDGE('',*,*,#10826,.T.);
#14322=ORIENTED_EDGE('',*,*,#10827,.F.);
#14323=ORIENTED_EDGE('',*,*,#10828,.F.);
#14324=ORIENTED_EDGE('',*,*,#10826,.F.);
#14325=ORIENTED_EDGE('',*,*,#10827,.T.);
#14326=ORIENTED_EDGE('',*,*,#10828,.T.);
#14327=ORIENTED_EDGE('',*,*,#10829,.T.);
#14328=ORIENTED_EDGE('',*,*,#10830,.T.);
#14329=ORIENTED_EDGE('',*,*,#10829,.F.);
#14330=ORIENTED_EDGE('',*,*,#10831,.T.);
#14331=ORIENTED_EDGE('',*,*,#10832,.T.);
#14332=ORIENTED_EDGE('',*,*,#10833,.F.);
#14333=ORIENTED_EDGE('',*,*,#10832,.F.);
#14334=ORIENTED_EDGE('',*,*,#10833,.T.);
#14335=ORIENTED_EDGE('',*,*,#10834,.T.);
#14336=ORIENTED_EDGE('',*,*,#10835,.F.);
#14337=ORIENTED_EDGE('',*,*,#10834,.F.);
#14338=ORIENTED_EDGE('',*,*,#10830,.F.);
#14339=ORIENTED_EDGE('',*,*,#10835,.T.);
#14340=ORIENTED_EDGE('',*,*,#10836,.F.);
#14341=ORIENTED_EDGE('',*,*,#10837,.T.);
#14342=ORIENTED_EDGE('',*,*,#10824,.T.);
#14343=ORIENTED_EDGE('',*,*,#10825,.T.);
#14344=ORIENTED_EDGE('',*,*,#10837,.F.);
#14345=ORIENTED_EDGE('',*,*,#10836,.T.);
#14346=ORIENTED_EDGE('',*,*,#10838,.F.);
#14347=ORIENTED_EDGE('',*,*,#10838,.T.);
#14348=ORIENTED_EDGE('',*,*,#10839,.T.);
#14349=ORIENTED_EDGE('',*,*,#10831,.F.);
#14350=ORIENTED_EDGE('',*,*,#10839,.F.);
#14351=ORIENTED_EDGE('',*,*,#10840,.F.);
#14352=ORIENTED_EDGE('',*,*,#10841,.F.);
#14353=ORIENTED_EDGE('',*,*,#10842,.T.);
#14354=ORIENTED_EDGE('',*,*,#10843,.F.);
#14355=ORIENTED_EDGE('',*,*,#10844,.F.);
#14356=ORIENTED_EDGE('',*,*,#10842,.F.);
#14357=ORIENTED_EDGE('',*,*,#10845,.T.);
#14358=ORIENTED_EDGE('',*,*,#10846,.T.);
#14359=ORIENTED_EDGE('',*,*,#10843,.T.);
#14360=ORIENTED_EDGE('',*,*,#10844,.T.);
#14361=ORIENTED_EDGE('',*,*,#10846,.F.);
#14362=ORIENTED_EDGE('',*,*,#10847,.F.);
#14363=ORIENTED_EDGE('',*,*,#10848,.T.);
#14364=ORIENTED_EDGE('',*,*,#10849,.F.);
#14365=ORIENTED_EDGE('',*,*,#10850,.T.);
#14366=ORIENTED_EDGE('',*,*,#10847,.T.);
#14367=ORIENTED_EDGE('',*,*,#10850,.F.);
#14368=ORIENTED_EDGE('',*,*,#10851,.F.);
#14369=ORIENTED_EDGE('',*,*,#10852,.T.);
#14370=ORIENTED_EDGE('',*,*,#10849,.T.);
#14371=ORIENTED_EDGE('',*,*,#10852,.F.);
#14372=ORIENTED_EDGE('',*,*,#10853,.F.);
#14373=ORIENTED_EDGE('',*,*,#10854,.T.);
#14374=ORIENTED_EDGE('',*,*,#10851,.T.);
#14375=ORIENTED_EDGE('',*,*,#10854,.F.);
#14376=ORIENTED_EDGE('',*,*,#10853,.T.);
#14377=ORIENTED_EDGE('',*,*,#10845,.F.);
#14378=ORIENTED_EDGE('',*,*,#10840,.T.);
#14379=ORIENTED_EDGE('',*,*,#10841,.T.);
#14380=ORIENTED_EDGE('',*,*,#10855,.T.);
#14381=ORIENTED_EDGE('',*,*,#10848,.F.);
#14382=ORIENTED_EDGE('',*,*,#10855,.F.);
#14383=ORIENTED_EDGE('',*,*,#10856,.T.);
#14384=ORIENTED_EDGE('',*,*,#10856,.F.);
#14385=ORIENTED_EDGE('',*,*,#10857,.T.);
#14386=ORIENTED_EDGE('',*,*,#10857,.F.);
#14387=ORIENTED_EDGE('',*,*,#10858,.T.);
#14388=ORIENTED_EDGE('',*,*,#10858,.F.);
#14389=ORIENTED_EDGE('',*,*,#10859,.T.);
#14390=ORIENTED_EDGE('',*,*,#10859,.F.);
#14391=ORIENTED_EDGE('',*,*,#10860,.T.);
#14392=ORIENTED_EDGE('',*,*,#10860,.F.);
#14393=ORIENTED_EDGE('',*,*,#10861,.T.);
#14394=ORIENTED_EDGE('',*,*,#10861,.F.);
#14395=ORIENTED_EDGE('',*,*,#10862,.T.);
#14396=ORIENTED_EDGE('',*,*,#10862,.F.);
#14397=ORIENTED_EDGE('',*,*,#10863,.T.);
#14398=ORIENTED_EDGE('',*,*,#10863,.F.);
#14399=ORIENTED_EDGE('',*,*,#10864,.F.);
#14400=ORIENTED_EDGE('',*,*,#10865,.F.);
#14401=ORIENTED_EDGE('',*,*,#10866,.F.);
#14402=ORIENTED_EDGE('',*,*,#10867,.F.);
#14403=ORIENTED_EDGE('',*,*,#10866,.T.);
#14404=ORIENTED_EDGE('',*,*,#10868,.F.);
#14405=ORIENTED_EDGE('',*,*,#10869,.T.);
#14406=ORIENTED_EDGE('',*,*,#10870,.F.);
#14407=ORIENTED_EDGE('',*,*,#10871,.T.);
#14408=ORIENTED_EDGE('',*,*,#10872,.F.);
#14409=ORIENTED_EDGE('',*,*,#10873,.T.);
#14410=ORIENTED_EDGE('',*,*,#10874,.T.);
#14411=ORIENTED_EDGE('',*,*,#10875,.F.);
#14412=ORIENTED_EDGE('',*,*,#10874,.F.);
#14413=ORIENTED_EDGE('',*,*,#10876,.T.);
#14414=ORIENTED_EDGE('',*,*,#10877,.F.);
#14415=ORIENTED_EDGE('',*,*,#10878,.T.);
#14416=ORIENTED_EDGE('',*,*,#10879,.F.);
#14417=ORIENTED_EDGE('',*,*,#10880,.T.);
#14418=ORIENTED_EDGE('',*,*,#10881,.F.);
#14419=ORIENTED_EDGE('',*,*,#10882,.T.);
#14420=ORIENTED_EDGE('',*,*,#10883,.F.);
#14421=ORIENTED_EDGE('',*,*,#10884,.T.);
#14422=ORIENTED_EDGE('',*,*,#10885,.F.);
#14423=ORIENTED_EDGE('',*,*,#10865,.T.);
#14424=ORIENTED_EDGE('',*,*,#10886,.T.);
#14425=ORIENTED_EDGE('',*,*,#10887,.T.);
#14426=ORIENTED_EDGE('',*,*,#10868,.T.);
#14427=ORIENTED_EDGE('',*,*,#10888,.F.);
#14428=ORIENTED_EDGE('',*,*,#10889,.F.);
#14429=ORIENTED_EDGE('',*,*,#10869,.F.);
#14430=ORIENTED_EDGE('',*,*,#10887,.F.);
#14431=ORIENTED_EDGE('',*,*,#10889,.T.);
#14432=ORIENTED_EDGE('',*,*,#10890,.T.);
#14433=ORIENTED_EDGE('',*,*,#10891,.T.);
#14434=ORIENTED_EDGE('',*,*,#10870,.T.);
#14435=ORIENTED_EDGE('',*,*,#10892,.F.);
#14436=ORIENTED_EDGE('',*,*,#10893,.F.);
#14437=ORIENTED_EDGE('',*,*,#10871,.F.);
#14438=ORIENTED_EDGE('',*,*,#10891,.F.);
#14439=ORIENTED_EDGE('',*,*,#10893,.T.);
#14440=ORIENTED_EDGE('',*,*,#10894,.T.);
#14441=ORIENTED_EDGE('',*,*,#10895,.T.);
#14442=ORIENTED_EDGE('',*,*,#10872,.T.);
#14443=ORIENTED_EDGE('',*,*,#10896,.F.);
#14444=ORIENTED_EDGE('',*,*,#10897,.F.);
#14445=ORIENTED_EDGE('',*,*,#10876,.F.);
#14446=ORIENTED_EDGE('',*,*,#10873,.F.);
#14447=ORIENTED_EDGE('',*,*,#10895,.F.);
#14448=ORIENTED_EDGE('',*,*,#10898,.F.);
#14449=ORIENTED_EDGE('',*,*,#10897,.T.);
#14450=ORIENTED_EDGE('',*,*,#10899,.T.);
#14451=ORIENTED_EDGE('',*,*,#10900,.T.);
#14452=ORIENTED_EDGE('',*,*,#10877,.T.);
#14453=ORIENTED_EDGE('',*,*,#10901,.F.);
#14454=ORIENTED_EDGE('',*,*,#10902,.F.);
#14455=ORIENTED_EDGE('',*,*,#10878,.F.);
#14456=ORIENTED_EDGE('',*,*,#10900,.F.);
#14457=ORIENTED_EDGE('',*,*,#10902,.T.);
#14458=ORIENTED_EDGE('',*,*,#10903,.T.);
#14459=ORIENTED_EDGE('',*,*,#10904,.T.);
#14460=ORIENTED_EDGE('',*,*,#10879,.T.);
#14461=ORIENTED_EDGE('',*,*,#10905,.F.);
#14462=ORIENTED_EDGE('',*,*,#10906,.F.);
#14463=ORIENTED_EDGE('',*,*,#10880,.F.);
#14464=ORIENTED_EDGE('',*,*,#10904,.F.);
#14465=ORIENTED_EDGE('',*,*,#10906,.T.);
#14466=ORIENTED_EDGE('',*,*,#10907,.T.);
#14467=ORIENTED_EDGE('',*,*,#10908,.T.);
#14468=ORIENTED_EDGE('',*,*,#10881,.T.);
#14469=ORIENTED_EDGE('',*,*,#10882,.F.);
#14470=ORIENTED_EDGE('',*,*,#10908,.F.);
#14471=ORIENTED_EDGE('',*,*,#10909,.F.);
#14472=ORIENTED_EDGE('',*,*,#10910,.F.);
#14473=ORIENTED_EDGE('',*,*,#10911,.F.);
#14474=ORIENTED_EDGE('',*,*,#10912,.T.);
#14475=ORIENTED_EDGE('',*,*,#10898,.T.);
#14476=ORIENTED_EDGE('',*,*,#10894,.F.);
#14477=ORIENTED_EDGE('',*,*,#10892,.T.);
#14478=ORIENTED_EDGE('',*,*,#10890,.F.);
#14479=ORIENTED_EDGE('',*,*,#10888,.T.);
#14480=ORIENTED_EDGE('',*,*,#10886,.F.);
#14481=ORIENTED_EDGE('',*,*,#10864,.T.);
#14482=ORIENTED_EDGE('',*,*,#10913,.F.);
#14483=ORIENTED_EDGE('',*,*,#10914,.T.);
#14484=ORIENTED_EDGE('',*,*,#10915,.F.);
#14485=ORIENTED_EDGE('',*,*,#10909,.T.);
#14486=ORIENTED_EDGE('',*,*,#10907,.F.);
#14487=ORIENTED_EDGE('',*,*,#10905,.T.);
#14488=ORIENTED_EDGE('',*,*,#10903,.F.);
#14489=ORIENTED_EDGE('',*,*,#10901,.T.);
#14490=ORIENTED_EDGE('',*,*,#10899,.F.);
#14491=ORIENTED_EDGE('',*,*,#10896,.T.);
#14492=ORIENTED_EDGE('',*,*,#10912,.F.);
#14493=ORIENTED_EDGE('',*,*,#10867,.T.);
#14494=ORIENTED_EDGE('',*,*,#10885,.T.);
#14495=ORIENTED_EDGE('',*,*,#10916,.T.);
#14496=ORIENTED_EDGE('',*,*,#10913,.T.);
#14497=ORIENTED_EDGE('',*,*,#10884,.F.);
#14498=ORIENTED_EDGE('',*,*,#10917,.F.);
#14499=ORIENTED_EDGE('',*,*,#10914,.F.);
#14500=ORIENTED_EDGE('',*,*,#10916,.F.);
#14501=ORIENTED_EDGE('',*,*,#10875,.T.);
#14502=ORIENTED_EDGE('',*,*,#10911,.T.);
#14503=ORIENTED_EDGE('',*,*,#10910,.T.);
#14504=ORIENTED_EDGE('',*,*,#10915,.T.);
#14505=ORIENTED_EDGE('',*,*,#10917,.T.);
#14506=ORIENTED_EDGE('',*,*,#10883,.T.);
#14507=ORIENTED_EDGE('',*,*,#10918,.F.);
#14508=ORIENTED_EDGE('',*,*,#10919,.T.);
#14509=ORIENTED_EDGE('',*,*,#10920,.F.);
#14510=ORIENTED_EDGE('',*,*,#10921,.T.);
#14511=ORIENTED_EDGE('',*,*,#10918,.T.);
#14512=ORIENTED_EDGE('',*,*,#10921,.F.);
#14513=ORIENTED_EDGE('',*,*,#10920,.T.);
#14514=ORIENTED_EDGE('',*,*,#10922,.F.);
#14515=ORIENTED_EDGE('',*,*,#10922,.T.);
#14516=ORIENTED_EDGE('',*,*,#10923,.T.);
#14517=ORIENTED_EDGE('',*,*,#10919,.F.);
#14518=ORIENTED_EDGE('',*,*,#10923,.F.);
#14519=ORIENTED_EDGE('',*,*,#10924,.F.);
#14520=ORIENTED_EDGE('',*,*,#10925,.T.);
#14521=ORIENTED_EDGE('',*,*,#10926,.F.);
#14522=ORIENTED_EDGE('',*,*,#10927,.T.);
#14523=ORIENTED_EDGE('',*,*,#10924,.T.);
#14524=ORIENTED_EDGE('',*,*,#10927,.F.);
#14525=ORIENTED_EDGE('',*,*,#10926,.T.);
#14526=ORIENTED_EDGE('',*,*,#10928,.F.);
#14527=ORIENTED_EDGE('',*,*,#10928,.T.);
#14528=ORIENTED_EDGE('',*,*,#10929,.T.);
#14529=ORIENTED_EDGE('',*,*,#10925,.F.);
#14530=ORIENTED_EDGE('',*,*,#10929,.F.);
#14531=ORIENTED_EDGE('',*,*,#10930,.F.);
#14532=ORIENTED_EDGE('',*,*,#10931,.T.);
#14533=ORIENTED_EDGE('',*,*,#10932,.F.);
#14534=ORIENTED_EDGE('',*,*,#10931,.F.);
#14535=ORIENTED_EDGE('',*,*,#10933,.T.);
#14536=ORIENTED_EDGE('',*,*,#10930,.T.);
#14537=ORIENTED_EDGE('',*,*,#10933,.F.);
#14538=ORIENTED_EDGE('',*,*,#10934,.F.);
#14539=ORIENTED_EDGE('',*,*,#10935,.F.);
#14540=ORIENTED_EDGE('',*,*,#10936,.T.);
#14541=ORIENTED_EDGE('',*,*,#10934,.T.);
#14542=ORIENTED_EDGE('',*,*,#10936,.F.);
#14543=ORIENTED_EDGE('',*,*,#10937,.F.);
#14544=ORIENTED_EDGE('',*,*,#10938,.T.);
#14545=ORIENTED_EDGE('',*,*,#10935,.T.);
#14546=ORIENTED_EDGE('',*,*,#10938,.F.);
#14547=ORIENTED_EDGE('',*,*,#10939,.F.);
#14548=ORIENTED_EDGE('',*,*,#10940,.T.);
#14549=ORIENTED_EDGE('',*,*,#10937,.T.);
#14550=ORIENTED_EDGE('',*,*,#10940,.F.);
#14551=ORIENTED_EDGE('',*,*,#10939,.T.);
#14552=ORIENTED_EDGE('',*,*,#10941,.F.);
#14553=ORIENTED_EDGE('',*,*,#10942,.F.);
#14554=ORIENTED_EDGE('',*,*,#10943,.T.);
#14555=ORIENTED_EDGE('',*,*,#10941,.T.);
#14556=ORIENTED_EDGE('',*,*,#10943,.F.);
#14557=ORIENTED_EDGE('',*,*,#10932,.T.);
#14558=ORIENTED_EDGE('',*,*,#10944,.T.);
#14559=ORIENTED_EDGE('',*,*,#10942,.T.);
#14560=ORIENTED_EDGE('',*,*,#10944,.F.);
#14561=ORIENTED_EDGE('',*,*,#10945,.T.);
#14562=ORIENTED_EDGE('',*,*,#10946,.T.);
#14563=ORIENTED_EDGE('',*,*,#10947,.T.);
#14564=ORIENTED_EDGE('',*,*,#10948,.F.);
#14565=ORIENTED_EDGE('',*,*,#10949,.T.);
#14566=ORIENTED_EDGE('',*,*,#10950,.T.);
#14567=ORIENTED_EDGE('',*,*,#10951,.T.);
#14568=ORIENTED_EDGE('',*,*,#10946,.F.);
#14569=ORIENTED_EDGE('',*,*,#10952,.T.);
#14570=ORIENTED_EDGE('',*,*,#10953,.T.);
#14571=ORIENTED_EDGE('',*,*,#10954,.T.);
#14572=ORIENTED_EDGE('',*,*,#10950,.F.);
#14573=ORIENTED_EDGE('',*,*,#10955,.T.);
#14574=ORIENTED_EDGE('',*,*,#10956,.T.);
#14575=ORIENTED_EDGE('',*,*,#10957,.T.);
#14576=ORIENTED_EDGE('',*,*,#10953,.F.);
#14577=ORIENTED_EDGE('',*,*,#10958,.T.);
#14578=ORIENTED_EDGE('',*,*,#10959,.T.);
#14579=ORIENTED_EDGE('',*,*,#10960,.T.);
#14580=ORIENTED_EDGE('',*,*,#10956,.F.);
#14581=ORIENTED_EDGE('',*,*,#10961,.T.);
#14582=ORIENTED_EDGE('',*,*,#10948,.T.);
#14583=ORIENTED_EDGE('',*,*,#10962,.T.);
#14584=ORIENTED_EDGE('',*,*,#10959,.F.);
#14585=ORIENTED_EDGE('',*,*,#10961,.F.);
#14586=ORIENTED_EDGE('',*,*,#10958,.F.);
#14587=ORIENTED_EDGE('',*,*,#10955,.F.);
#14588=ORIENTED_EDGE('',*,*,#10952,.F.);
#14589=ORIENTED_EDGE('',*,*,#10949,.F.);
#14590=ORIENTED_EDGE('',*,*,#10945,.F.);
#14591=ORIENTED_EDGE('',*,*,#10962,.F.);
#14592=ORIENTED_EDGE('',*,*,#10947,.F.);
#14593=ORIENTED_EDGE('',*,*,#10951,.F.);
#14594=ORIENTED_EDGE('',*,*,#10954,.F.);
#14595=ORIENTED_EDGE('',*,*,#10957,.F.);
#14596=ORIENTED_EDGE('',*,*,#10960,.F.);
#14597=ORIENTED_EDGE('',*,*,#10963,.T.);
#14598=ORIENTED_EDGE('',*,*,#10964,.T.);
#14599=ORIENTED_EDGE('',*,*,#10965,.T.);
#14600=ORIENTED_EDGE('',*,*,#10966,.F.);
#14601=ORIENTED_EDGE('',*,*,#10967,.T.);
#14602=ORIENTED_EDGE('',*,*,#10968,.T.);
#14603=ORIENTED_EDGE('',*,*,#10969,.T.);
#14604=ORIENTED_EDGE('',*,*,#10964,.F.);
#14605=ORIENTED_EDGE('',*,*,#10970,.T.);
#14606=ORIENTED_EDGE('',*,*,#10971,.T.);
#14607=ORIENTED_EDGE('',*,*,#10972,.T.);
#14608=ORIENTED_EDGE('',*,*,#10968,.F.);
#14609=ORIENTED_EDGE('',*,*,#10973,.T.);
#14610=ORIENTED_EDGE('',*,*,#10974,.T.);
#14611=ORIENTED_EDGE('',*,*,#10975,.T.);
#14612=ORIENTED_EDGE('',*,*,#10971,.F.);
#14613=ORIENTED_EDGE('',*,*,#10976,.T.);
#14614=ORIENTED_EDGE('',*,*,#10977,.T.);
#14615=ORIENTED_EDGE('',*,*,#10978,.T.);
#14616=ORIENTED_EDGE('',*,*,#10974,.F.);
#14617=ORIENTED_EDGE('',*,*,#10979,.T.);
#14618=ORIENTED_EDGE('',*,*,#10966,.T.);
#14619=ORIENTED_EDGE('',*,*,#10980,.T.);
#14620=ORIENTED_EDGE('',*,*,#10977,.F.);
#14621=ORIENTED_EDGE('',*,*,#10979,.F.);
#14622=ORIENTED_EDGE('',*,*,#10976,.F.);
#14623=ORIENTED_EDGE('',*,*,#10973,.F.);
#14624=ORIENTED_EDGE('',*,*,#10970,.F.);
#14625=ORIENTED_EDGE('',*,*,#10967,.F.);
#14626=ORIENTED_EDGE('',*,*,#10963,.F.);
#14627=ORIENTED_EDGE('',*,*,#10980,.F.);
#14628=ORIENTED_EDGE('',*,*,#10965,.F.);
#14629=ORIENTED_EDGE('',*,*,#10969,.F.);
#14630=ORIENTED_EDGE('',*,*,#10972,.F.);
#14631=ORIENTED_EDGE('',*,*,#10975,.F.);
#14632=ORIENTED_EDGE('',*,*,#10978,.F.);
#14633=ORIENTED_EDGE('',*,*,#10981,.F.);
#14634=ORIENTED_EDGE('',*,*,#10982,.F.);
#14635=ORIENTED_EDGE('',*,*,#10983,.F.);
#14636=ORIENTED_EDGE('',*,*,#10984,.T.);
#14637=ORIENTED_EDGE('',*,*,#10982,.T.);
#14638=ORIENTED_EDGE('',*,*,#10984,.F.);
#14639=ORIENTED_EDGE('',*,*,#10985,.F.);
#14640=ORIENTED_EDGE('',*,*,#10986,.T.);
#14641=ORIENTED_EDGE('',*,*,#10983,.T.);
#14642=ORIENTED_EDGE('',*,*,#10986,.F.);
#14643=ORIENTED_EDGE('',*,*,#10987,.F.);
#14644=ORIENTED_EDGE('',*,*,#10988,.T.);
#14645=ORIENTED_EDGE('',*,*,#10985,.T.);
#14646=ORIENTED_EDGE('',*,*,#10988,.F.);
#14647=ORIENTED_EDGE('',*,*,#10987,.T.);
#14648=ORIENTED_EDGE('',*,*,#10989,.F.);
#14649=ORIENTED_EDGE('',*,*,#10990,.F.);
#14650=ORIENTED_EDGE('',*,*,#10991,.T.);
#14651=ORIENTED_EDGE('',*,*,#10989,.T.);
#14652=ORIENTED_EDGE('',*,*,#10991,.F.);
#14653=ORIENTED_EDGE('',*,*,#10981,.T.);
#14654=ORIENTED_EDGE('',*,*,#10992,.T.);
#14655=ORIENTED_EDGE('',*,*,#10990,.T.);
#14656=ORIENTED_EDGE('',*,*,#10992,.F.);
#14657=ORIENTED_EDGE('',*,*,#10993,.F.);
#14658=ORIENTED_EDGE('',*,*,#10994,.T.);
#14659=ORIENTED_EDGE('',*,*,#10995,.F.);
#14660=ORIENTED_EDGE('',*,*,#10996,.F.);
#14661=ORIENTED_EDGE('',*,*,#10997,.F.);
#14662=ORIENTED_EDGE('',*,*,#10998,.T.);
#14663=ORIENTED_EDGE('',*,*,#10999,.F.);
#14664=ORIENTED_EDGE('',*,*,#10994,.F.);
#14665=ORIENTED_EDGE('',*,*,#11000,.F.);
#14666=ORIENTED_EDGE('',*,*,#11001,.T.);
#14667=ORIENTED_EDGE('',*,*,#11002,.F.);
#14668=ORIENTED_EDGE('',*,*,#10998,.F.);
#14669=ORIENTED_EDGE('',*,*,#11003,.F.);
#14670=ORIENTED_EDGE('',*,*,#11004,.T.);
#14671=ORIENTED_EDGE('',*,*,#11005,.F.);
#14672=ORIENTED_EDGE('',*,*,#11001,.F.);
#14673=ORIENTED_EDGE('',*,*,#11006,.F.);
#14674=ORIENTED_EDGE('',*,*,#11007,.T.);
#14675=ORIENTED_EDGE('',*,*,#11008,.F.);
#14676=ORIENTED_EDGE('',*,*,#11004,.F.);
#14677=ORIENTED_EDGE('',*,*,#11009,.F.);
#14678=ORIENTED_EDGE('',*,*,#11010,.T.);
#14679=ORIENTED_EDGE('',*,*,#11011,.F.);
#14680=ORIENTED_EDGE('',*,*,#11007,.F.);
#14681=ORIENTED_EDGE('',*,*,#11012,.F.);
#14682=ORIENTED_EDGE('',*,*,#11013,.T.);
#14683=ORIENTED_EDGE('',*,*,#11014,.F.);
#14684=ORIENTED_EDGE('',*,*,#11010,.F.);
#14685=ORIENTED_EDGE('',*,*,#11015,.F.);
#14686=ORIENTED_EDGE('',*,*,#11016,.T.);
#14687=ORIENTED_EDGE('',*,*,#11017,.F.);
#14688=ORIENTED_EDGE('',*,*,#11013,.F.);
#14689=ORIENTED_EDGE('',*,*,#11018,.F.);
#14690=ORIENTED_EDGE('',*,*,#11019,.F.);
#14691=ORIENTED_EDGE('',*,*,#11020,.F.);
#14692=ORIENTED_EDGE('',*,*,#11016,.F.);
#14693=ORIENTED_EDGE('',*,*,#11021,.F.);
#14694=ORIENTED_EDGE('',*,*,#11022,.T.);
#14695=ORIENTED_EDGE('',*,*,#11023,.F.);
#14696=ORIENTED_EDGE('',*,*,#11024,.F.);
#14697=ORIENTED_EDGE('',*,*,#11025,.F.);
#14698=ORIENTED_EDGE('',*,*,#11026,.T.);
#14699=ORIENTED_EDGE('',*,*,#11027,.F.);
#14700=ORIENTED_EDGE('',*,*,#11022,.F.);
#14701=ORIENTED_EDGE('',*,*,#11028,.F.);
#14702=ORIENTED_EDGE('',*,*,#11029,.T.);
#14703=ORIENTED_EDGE('',*,*,#11030,.F.);
#14704=ORIENTED_EDGE('',*,*,#11026,.F.);
#14705=ORIENTED_EDGE('',*,*,#11031,.F.);
#14706=ORIENTED_EDGE('',*,*,#11032,.T.);
#14707=ORIENTED_EDGE('',*,*,#11033,.F.);
#14708=ORIENTED_EDGE('',*,*,#11029,.F.);
#14709=ORIENTED_EDGE('',*,*,#11034,.F.);
#14710=ORIENTED_EDGE('',*,*,#11035,.T.);
#14711=ORIENTED_EDGE('',*,*,#11036,.F.);
#14712=ORIENTED_EDGE('',*,*,#11032,.F.);
#14713=ORIENTED_EDGE('',*,*,#11037,.F.);
#14714=ORIENTED_EDGE('',*,*,#11038,.T.);
#14715=ORIENTED_EDGE('',*,*,#11039,.F.);
#14716=ORIENTED_EDGE('',*,*,#11035,.F.);
#14717=ORIENTED_EDGE('',*,*,#11040,.F.);
#14718=ORIENTED_EDGE('',*,*,#11041,.T.);
#14719=ORIENTED_EDGE('',*,*,#11042,.F.);
#14720=ORIENTED_EDGE('',*,*,#11038,.F.);
#14721=ORIENTED_EDGE('',*,*,#11043,.F.);
#14722=ORIENTED_EDGE('',*,*,#11044,.T.);
#14723=ORIENTED_EDGE('',*,*,#11045,.F.);
#14724=ORIENTED_EDGE('',*,*,#11041,.F.);
#14725=ORIENTED_EDGE('',*,*,#11046,.F.);
#14726=ORIENTED_EDGE('',*,*,#11047,.F.);
#14727=ORIENTED_EDGE('',*,*,#11048,.F.);
#14728=ORIENTED_EDGE('',*,*,#11044,.F.);
#14729=ORIENTED_EDGE('',*,*,#11049,.F.);
#14730=ORIENTED_EDGE('',*,*,#11050,.T.);
#14731=ORIENTED_EDGE('',*,*,#11051,.F.);
#14732=ORIENTED_EDGE('',*,*,#11052,.F.);
#14733=ORIENTED_EDGE('',*,*,#11053,.F.);
#14734=ORIENTED_EDGE('',*,*,#11054,.T.);
#14735=ORIENTED_EDGE('',*,*,#11055,.F.);
#14736=ORIENTED_EDGE('',*,*,#11050,.F.);
#14737=ORIENTED_EDGE('',*,*,#11056,.F.);
#14738=ORIENTED_EDGE('',*,*,#11057,.T.);
#14739=ORIENTED_EDGE('',*,*,#11058,.F.);
#14740=ORIENTED_EDGE('',*,*,#11054,.F.);
#14741=ORIENTED_EDGE('',*,*,#11059,.F.);
#14742=ORIENTED_EDGE('',*,*,#11060,.T.);
#14743=ORIENTED_EDGE('',*,*,#11061,.F.);
#14744=ORIENTED_EDGE('',*,*,#11057,.F.);
#14745=ORIENTED_EDGE('',*,*,#11062,.F.);
#14746=ORIENTED_EDGE('',*,*,#11063,.T.);
#14747=ORIENTED_EDGE('',*,*,#11064,.F.);
#14748=ORIENTED_EDGE('',*,*,#11060,.F.);
#14749=ORIENTED_EDGE('',*,*,#11065,.F.);
#14750=ORIENTED_EDGE('',*,*,#11066,.T.);
#14751=ORIENTED_EDGE('',*,*,#11067,.F.);
#14752=ORIENTED_EDGE('',*,*,#11063,.F.);
#14753=ORIENTED_EDGE('',*,*,#11068,.F.);
#14754=ORIENTED_EDGE('',*,*,#11069,.T.);
#14755=ORIENTED_EDGE('',*,*,#11070,.F.);
#14756=ORIENTED_EDGE('',*,*,#11066,.F.);
#14757=ORIENTED_EDGE('',*,*,#11071,.F.);
#14758=ORIENTED_EDGE('',*,*,#11072,.T.);
#14759=ORIENTED_EDGE('',*,*,#11073,.F.);
#14760=ORIENTED_EDGE('',*,*,#11069,.F.);
#14761=ORIENTED_EDGE('',*,*,#11074,.F.);
#14762=ORIENTED_EDGE('',*,*,#11075,.F.);
#14763=ORIENTED_EDGE('',*,*,#11076,.F.);
#14764=ORIENTED_EDGE('',*,*,#11072,.F.);
#14765=ORIENTED_EDGE('',*,*,#11077,.F.);
#14766=ORIENTED_EDGE('',*,*,#11078,.T.);
#14767=ORIENTED_EDGE('',*,*,#11079,.F.);
#14768=ORIENTED_EDGE('',*,*,#11080,.F.);
#14769=ORIENTED_EDGE('',*,*,#11081,.F.);
#14770=ORIENTED_EDGE('',*,*,#11082,.T.);
#14771=ORIENTED_EDGE('',*,*,#11083,.F.);
#14772=ORIENTED_EDGE('',*,*,#11078,.F.);
#14773=ORIENTED_EDGE('',*,*,#11084,.F.);
#14774=ORIENTED_EDGE('',*,*,#11085,.T.);
#14775=ORIENTED_EDGE('',*,*,#11086,.F.);
#14776=ORIENTED_EDGE('',*,*,#11082,.F.);
#14777=ORIENTED_EDGE('',*,*,#11087,.F.);
#14778=ORIENTED_EDGE('',*,*,#11088,.T.);
#14779=ORIENTED_EDGE('',*,*,#11089,.F.);
#14780=ORIENTED_EDGE('',*,*,#11085,.F.);
#14781=ORIENTED_EDGE('',*,*,#11090,.F.);
#14782=ORIENTED_EDGE('',*,*,#11091,.T.);
#14783=ORIENTED_EDGE('',*,*,#11092,.F.);
#14784=ORIENTED_EDGE('',*,*,#11088,.F.);
#14785=ORIENTED_EDGE('',*,*,#11093,.F.);
#14786=ORIENTED_EDGE('',*,*,#11094,.T.);
#14787=ORIENTED_EDGE('',*,*,#11095,.F.);
#14788=ORIENTED_EDGE('',*,*,#11091,.F.);
#14789=ORIENTED_EDGE('',*,*,#11096,.F.);
#14790=ORIENTED_EDGE('',*,*,#11097,.T.);
#14791=ORIENTED_EDGE('',*,*,#11098,.F.);
#14792=ORIENTED_EDGE('',*,*,#11094,.F.);
#14793=ORIENTED_EDGE('',*,*,#11099,.F.);
#14794=ORIENTED_EDGE('',*,*,#11100,.T.);
#14795=ORIENTED_EDGE('',*,*,#11101,.F.);
#14796=ORIENTED_EDGE('',*,*,#11097,.F.);
#14797=ORIENTED_EDGE('',*,*,#11102,.F.);
#14798=ORIENTED_EDGE('',*,*,#11103,.F.);
#14799=ORIENTED_EDGE('',*,*,#11104,.F.);
#14800=ORIENTED_EDGE('',*,*,#11100,.F.);
#14801=ORIENTED_EDGE('',*,*,#11105,.F.);
#14802=ORIENTED_EDGE('',*,*,#11106,.T.);
#14803=ORIENTED_EDGE('',*,*,#11107,.F.);
#14804=ORIENTED_EDGE('',*,*,#11106,.F.);
#14805=ORIENTED_EDGE('',*,*,#11019,.T.);
#14806=ORIENTED_EDGE('',*,*,#11108,.T.);
#14807=ORIENTED_EDGE('',*,*,#11109,.T.);
#14808=ORIENTED_EDGE('',*,*,#11110,.F.);
#14809=ORIENTED_EDGE('',*,*,#10996,.T.);
#14810=ORIENTED_EDGE('',*,*,#11111,.F.);
#14811=ORIENTED_EDGE('',*,*,#11112,.F.);
#14812=ORIENTED_EDGE('',*,*,#11113,.T.);
#14813=ORIENTED_EDGE('',*,*,#11047,.T.);
#14814=ORIENTED_EDGE('',*,*,#11114,.T.);
#14815=ORIENTED_EDGE('',*,*,#11112,.T.);
#14816=ORIENTED_EDGE('',*,*,#11115,.F.);
#14817=ORIENTED_EDGE('',*,*,#11024,.T.);
#14818=ORIENTED_EDGE('',*,*,#11116,.F.);
#14819=ORIENTED_EDGE('',*,*,#11117,.F.);
#14820=ORIENTED_EDGE('',*,*,#11118,.T.);
#14821=ORIENTED_EDGE('',*,*,#11075,.T.);
#14822=ORIENTED_EDGE('',*,*,#11119,.T.);
#14823=ORIENTED_EDGE('',*,*,#11117,.T.);
#14824=ORIENTED_EDGE('',*,*,#11120,.F.);
#14825=ORIENTED_EDGE('',*,*,#11052,.T.);
#14826=ORIENTED_EDGE('',*,*,#11121,.F.);
#14827=ORIENTED_EDGE('',*,*,#11122,.F.);
#14828=ORIENTED_EDGE('',*,*,#11123,.T.);
#14829=ORIENTED_EDGE('',*,*,#11103,.T.);
#14830=ORIENTED_EDGE('',*,*,#11124,.T.);
#14831=ORIENTED_EDGE('',*,*,#11122,.T.);
#14832=ORIENTED_EDGE('',*,*,#11125,.F.);
#14833=ORIENTED_EDGE('',*,*,#11080,.T.);
#14834=ORIENTED_EDGE('',*,*,#11126,.F.);
#14835=ORIENTED_EDGE('',*,*,#11109,.F.);
#14836=ORIENTED_EDGE('',*,*,#11127,.T.);
#14837=ORIENTED_EDGE('',*,*,#10995,.T.);
#14838=ORIENTED_EDGE('',*,*,#10999,.T.);
#14839=ORIENTED_EDGE('',*,*,#11002,.T.);
#14840=ORIENTED_EDGE('',*,*,#11005,.T.);
#14841=ORIENTED_EDGE('',*,*,#11008,.T.);
#14842=ORIENTED_EDGE('',*,*,#11011,.T.);
#14843=ORIENTED_EDGE('',*,*,#11014,.T.);
#14844=ORIENTED_EDGE('',*,*,#11017,.T.);
#14845=ORIENTED_EDGE('',*,*,#11020,.T.);
#14846=ORIENTED_EDGE('',*,*,#11110,.T.);
#14847=ORIENTED_EDGE('',*,*,#11126,.T.);
#14848=ORIENTED_EDGE('',*,*,#11079,.T.);
#14849=ORIENTED_EDGE('',*,*,#11083,.T.);
#14850=ORIENTED_EDGE('',*,*,#11086,.T.);
#14851=ORIENTED_EDGE('',*,*,#11089,.T.);
#14852=ORIENTED_EDGE('',*,*,#11092,.T.);
#14853=ORIENTED_EDGE('',*,*,#11095,.T.);
#14854=ORIENTED_EDGE('',*,*,#11098,.T.);
#14855=ORIENTED_EDGE('',*,*,#11101,.T.);
#14856=ORIENTED_EDGE('',*,*,#11104,.T.);
#14857=ORIENTED_EDGE('',*,*,#11125,.T.);
#14858=ORIENTED_EDGE('',*,*,#11121,.T.);
#14859=ORIENTED_EDGE('',*,*,#11051,.T.);
#14860=ORIENTED_EDGE('',*,*,#11055,.T.);
#14861=ORIENTED_EDGE('',*,*,#11058,.T.);
#14862=ORIENTED_EDGE('',*,*,#11061,.T.);
#14863=ORIENTED_EDGE('',*,*,#11064,.T.);
#14864=ORIENTED_EDGE('',*,*,#11067,.T.);
#14865=ORIENTED_EDGE('',*,*,#11070,.T.);
#14866=ORIENTED_EDGE('',*,*,#11073,.T.);
#14867=ORIENTED_EDGE('',*,*,#11076,.T.);
#14868=ORIENTED_EDGE('',*,*,#11120,.T.);
#14869=ORIENTED_EDGE('',*,*,#11116,.T.);
#14870=ORIENTED_EDGE('',*,*,#11023,.T.);
#14871=ORIENTED_EDGE('',*,*,#11027,.T.);
#14872=ORIENTED_EDGE('',*,*,#11030,.T.);
#14873=ORIENTED_EDGE('',*,*,#11033,.T.);
#14874=ORIENTED_EDGE('',*,*,#11036,.T.);
#14875=ORIENTED_EDGE('',*,*,#11039,.T.);
#14876=ORIENTED_EDGE('',*,*,#11042,.T.);
#14877=ORIENTED_EDGE('',*,*,#11045,.T.);
#14878=ORIENTED_EDGE('',*,*,#11048,.T.);
#14879=ORIENTED_EDGE('',*,*,#11115,.T.);
#14880=ORIENTED_EDGE('',*,*,#11111,.T.);
#14881=ORIENTED_EDGE('',*,*,#11107,.T.);
#14882=ORIENTED_EDGE('',*,*,#10993,.T.);
#14883=ORIENTED_EDGE('',*,*,#11113,.F.);
#14884=ORIENTED_EDGE('',*,*,#11114,.F.);
#14885=ORIENTED_EDGE('',*,*,#11046,.T.);
#14886=ORIENTED_EDGE('',*,*,#11043,.T.);
#14887=ORIENTED_EDGE('',*,*,#11040,.T.);
#14888=ORIENTED_EDGE('',*,*,#11037,.T.);
#14889=ORIENTED_EDGE('',*,*,#11034,.T.);
#14890=ORIENTED_EDGE('',*,*,#11031,.T.);
#14891=ORIENTED_EDGE('',*,*,#11028,.T.);
#14892=ORIENTED_EDGE('',*,*,#11025,.T.);
#14893=ORIENTED_EDGE('',*,*,#11021,.T.);
#14894=ORIENTED_EDGE('',*,*,#11118,.F.);
#14895=ORIENTED_EDGE('',*,*,#11119,.F.);
#14896=ORIENTED_EDGE('',*,*,#11074,.T.);
#14897=ORIENTED_EDGE('',*,*,#11071,.T.);
#14898=ORIENTED_EDGE('',*,*,#11068,.T.);
#14899=ORIENTED_EDGE('',*,*,#11065,.T.);
#14900=ORIENTED_EDGE('',*,*,#11062,.T.);
#14901=ORIENTED_EDGE('',*,*,#11059,.T.);
#14902=ORIENTED_EDGE('',*,*,#11056,.T.);
#14903=ORIENTED_EDGE('',*,*,#11053,.T.);
#14904=ORIENTED_EDGE('',*,*,#11049,.T.);
#14905=ORIENTED_EDGE('',*,*,#11123,.F.);
#14906=ORIENTED_EDGE('',*,*,#11124,.F.);
#14907=ORIENTED_EDGE('',*,*,#11102,.T.);
#14908=ORIENTED_EDGE('',*,*,#11099,.T.);
#14909=ORIENTED_EDGE('',*,*,#11096,.T.);
#14910=ORIENTED_EDGE('',*,*,#11093,.T.);
#14911=ORIENTED_EDGE('',*,*,#11090,.T.);
#14912=ORIENTED_EDGE('',*,*,#11087,.T.);
#14913=ORIENTED_EDGE('',*,*,#11084,.T.);
#14914=ORIENTED_EDGE('',*,*,#11081,.T.);
#14915=ORIENTED_EDGE('',*,*,#11077,.T.);
#14916=ORIENTED_EDGE('',*,*,#11127,.F.);
#14917=ORIENTED_EDGE('',*,*,#11108,.F.);
#14918=ORIENTED_EDGE('',*,*,#11018,.T.);
#14919=ORIENTED_EDGE('',*,*,#11015,.T.);
#14920=ORIENTED_EDGE('',*,*,#11012,.T.);
#14921=ORIENTED_EDGE('',*,*,#11009,.T.);
#14922=ORIENTED_EDGE('',*,*,#11006,.T.);
#14923=ORIENTED_EDGE('',*,*,#11003,.T.);
#14924=ORIENTED_EDGE('',*,*,#11000,.T.);
#14925=ORIENTED_EDGE('',*,*,#10997,.T.);
#14926=ORIENTED_EDGE('',*,*,#11105,.T.);
#14927=ORIENTED_EDGE('',*,*,#11128,.F.);
#14928=ORIENTED_EDGE('',*,*,#11129,.F.);
#14929=ORIENTED_EDGE('',*,*,#11130,.T.);
#14930=ORIENTED_EDGE('',*,*,#11128,.T.);
#14931=ORIENTED_EDGE('',*,*,#11130,.F.);
#14932=ORIENTED_EDGE('',*,*,#11131,.F.);
#14933=ORIENTED_EDGE('',*,*,#11132,.T.);
#14934=ORIENTED_EDGE('',*,*,#11129,.T.);
#14935=ORIENTED_EDGE('',*,*,#11132,.F.);
#14936=ORIENTED_EDGE('',*,*,#11133,.F.);
#14937=ORIENTED_EDGE('',*,*,#11134,.T.);
#14938=ORIENTED_EDGE('',*,*,#11131,.T.);
#14939=ORIENTED_EDGE('',*,*,#11134,.F.);
#14940=ORIENTED_EDGE('',*,*,#11133,.T.);
#14941=ORIENTED_EDGE('',*,*,#11135,.F.);
#14942=ORIENTED_EDGE('',*,*,#11136,.F.);
#14943=ORIENTED_EDGE('',*,*,#11137,.T.);
#14944=ORIENTED_EDGE('',*,*,#11135,.T.);
#14945=ORIENTED_EDGE('',*,*,#11137,.F.);
#14946=ORIENTED_EDGE('',*,*,#11138,.F.);
#14947=ORIENTED_EDGE('',*,*,#11139,.T.);
#14948=ORIENTED_EDGE('',*,*,#11136,.T.);
#14949=ORIENTED_EDGE('',*,*,#11139,.F.);
#14950=ORIENTED_EDGE('',*,*,#11140,.F.);
#14951=ORIENTED_EDGE('',*,*,#11141,.T.);
#14952=ORIENTED_EDGE('',*,*,#11138,.T.);
#14953=ORIENTED_EDGE('',*,*,#11141,.F.);
#14954=ORIENTED_EDGE('',*,*,#11140,.T.);
#14955=ORIENTED_EDGE('',*,*,#11142,.T.);
#14956=ORIENTED_EDGE('',*,*,#11143,.T.);
#14957=ORIENTED_EDGE('',*,*,#11144,.T.);
#14958=ORIENTED_EDGE('',*,*,#11145,.F.);
#14959=ORIENTED_EDGE('',*,*,#11146,.T.);
#14960=ORIENTED_EDGE('',*,*,#11147,.T.);
#14961=ORIENTED_EDGE('',*,*,#11148,.T.);
#14962=ORIENTED_EDGE('',*,*,#11143,.F.);
#14963=ORIENTED_EDGE('',*,*,#11149,.T.);
#14964=ORIENTED_EDGE('',*,*,#11150,.T.);
#14965=ORIENTED_EDGE('',*,*,#11151,.T.);
#14966=ORIENTED_EDGE('',*,*,#11147,.F.);
#14967=ORIENTED_EDGE('',*,*,#11152,.T.);
#14968=ORIENTED_EDGE('',*,*,#11153,.T.);
#14969=ORIENTED_EDGE('',*,*,#11154,.T.);
#14970=ORIENTED_EDGE('',*,*,#11150,.F.);
#14971=ORIENTED_EDGE('',*,*,#11155,.T.);
#14972=ORIENTED_EDGE('',*,*,#11156,.T.);
#14973=ORIENTED_EDGE('',*,*,#11157,.T.);
#14974=ORIENTED_EDGE('',*,*,#11153,.F.);
#14975=ORIENTED_EDGE('',*,*,#11158,.T.);
#14976=ORIENTED_EDGE('',*,*,#11145,.T.);
#14977=ORIENTED_EDGE('',*,*,#11159,.T.);
#14978=ORIENTED_EDGE('',*,*,#11156,.F.);
#14979=ORIENTED_EDGE('',*,*,#11158,.F.);
#14980=ORIENTED_EDGE('',*,*,#11155,.F.);
#14981=ORIENTED_EDGE('',*,*,#11152,.F.);
#14982=ORIENTED_EDGE('',*,*,#11149,.F.);
#14983=ORIENTED_EDGE('',*,*,#11146,.F.);
#14984=ORIENTED_EDGE('',*,*,#11142,.F.);
#14985=ORIENTED_EDGE('',*,*,#11159,.F.);
#14986=ORIENTED_EDGE('',*,*,#11144,.F.);
#14987=ORIENTED_EDGE('',*,*,#11148,.F.);
#14988=ORIENTED_EDGE('',*,*,#11151,.F.);
#14989=ORIENTED_EDGE('',*,*,#11154,.F.);
#14990=ORIENTED_EDGE('',*,*,#11157,.F.);
#14991=ORIENTED_EDGE('',*,*,#11160,.F.);
#14992=ORIENTED_EDGE('',*,*,#11161,.F.);
#14993=ORIENTED_EDGE('',*,*,#11162,.F.);
#14994=ORIENTED_EDGE('',*,*,#11163,.F.);
#14995=ORIENTED_EDGE('',*,*,#11162,.T.);
#14996=ORIENTED_EDGE('',*,*,#11164,.T.);
#14997=ORIENTED_EDGE('',*,*,#11165,.F.);
#14998=ORIENTED_EDGE('',*,*,#11166,.F.);
#14999=ORIENTED_EDGE('',*,*,#11167,.T.);
#15000=ORIENTED_EDGE('',*,*,#11168,.T.);
#15001=ORIENTED_EDGE('',*,*,#11169,.T.);
#15002=ORIENTED_EDGE('',*,*,#11165,.T.);
#15003=ORIENTED_EDGE('',*,*,#11170,.T.);
#15004=ORIENTED_EDGE('',*,*,#11167,.F.);
#15005=ORIENTED_EDGE('',*,*,#11164,.F.);
#15006=ORIENTED_EDGE('',*,*,#11161,.T.);
#15007=ORIENTED_EDGE('',*,*,#11171,.F.);
#15008=ORIENTED_EDGE('',*,*,#11172,.F.);
#15009=ORIENTED_EDGE('',*,*,#11173,.T.);
#15010=ORIENTED_EDGE('',*,*,#11174,.F.);
#15011=ORIENTED_EDGE('',*,*,#11175,.T.);
#15012=ORIENTED_EDGE('',*,*,#11176,.T.);
#15013=ORIENTED_EDGE('',*,*,#11177,.T.);
#15014=ORIENTED_EDGE('',*,*,#11178,.T.);
#15015=ORIENTED_EDGE('',*,*,#11179,.T.);
#15016=ORIENTED_EDGE('',*,*,#11168,.F.);
#15017=ORIENTED_EDGE('',*,*,#11177,.F.);
#15018=ORIENTED_EDGE('',*,*,#11180,.F.);
#15019=ORIENTED_EDGE('',*,*,#11181,.F.);
#15020=ORIENTED_EDGE('',*,*,#11178,.F.);
#15021=ORIENTED_EDGE('',*,*,#11176,.F.);
#15022=ORIENTED_EDGE('',*,*,#11169,.F.);
#15023=ORIENTED_EDGE('',*,*,#11179,.F.);
#15024=ORIENTED_EDGE('',*,*,#11181,.T.);
#15025=ORIENTED_EDGE('',*,*,#11182,.F.);
#15026=ORIENTED_EDGE('',*,*,#11183,.F.);
#15027=ORIENTED_EDGE('',*,*,#11184,.T.);
#15028=ORIENTED_EDGE('',*,*,#11185,.F.);
#15029=ORIENTED_EDGE('',*,*,#11186,.T.);
#15030=ORIENTED_EDGE('',*,*,#11163,.T.);
#15031=ORIENTED_EDGE('',*,*,#11166,.T.);
#15032=ORIENTED_EDGE('',*,*,#11180,.T.);
#15033=ORIENTED_EDGE('',*,*,#11175,.F.);
#15034=ORIENTED_EDGE('',*,*,#11187,.F.);
#15035=ORIENTED_EDGE('',*,*,#11182,.T.);
#15036=ORIENTED_EDGE('',*,*,#11183,.T.);
#15037=ORIENTED_EDGE('',*,*,#11187,.T.);
#15038=ORIENTED_EDGE('',*,*,#11174,.T.);
#15039=ORIENTED_EDGE('',*,*,#11188,.T.);
#15040=ORIENTED_EDGE('',*,*,#11189,.T.);
#15041=ORIENTED_EDGE('',*,*,#11190,.T.);
#15042=ORIENTED_EDGE('',*,*,#11189,.F.);
#15043=ORIENTED_EDGE('',*,*,#11191,.F.);
#15044=ORIENTED_EDGE('',*,*,#11192,.T.);
#15045=ORIENTED_EDGE('',*,*,#11170,.F.);
#15046=ORIENTED_EDGE('',*,*,#11192,.F.);
#15047=ORIENTED_EDGE('',*,*,#11193,.F.);
#15048=ORIENTED_EDGE('',*,*,#11194,.F.);
#15049=ORIENTED_EDGE('',*,*,#11195,.F.);
#15050=ORIENTED_EDGE('',*,*,#11188,.F.);
#15051=ORIENTED_EDGE('',*,*,#11173,.F.);
#15052=ORIENTED_EDGE('',*,*,#11196,.F.);
#15053=ORIENTED_EDGE('',*,*,#11193,.T.);
#15054=ORIENTED_EDGE('',*,*,#11191,.T.);
#15055=ORIENTED_EDGE('',*,*,#11190,.F.);
#15056=ORIENTED_EDGE('',*,*,#11195,.T.);
#15057=ORIENTED_EDGE('',*,*,#11197,.F.);
#15058=ORIENTED_EDGE('',*,*,#11184,.F.);
#15059=ORIENTED_EDGE('',*,*,#11172,.T.);
#15060=ORIENTED_EDGE('',*,*,#11198,.T.);
#15061=ORIENTED_EDGE('',*,*,#11185,.T.);
#15062=ORIENTED_EDGE('',*,*,#11197,.T.);
#15063=ORIENTED_EDGE('',*,*,#11194,.T.);
#15064=ORIENTED_EDGE('',*,*,#11196,.T.);
#15065=ORIENTED_EDGE('',*,*,#11160,.T.);
#15066=ORIENTED_EDGE('',*,*,#11186,.F.);
#15067=ORIENTED_EDGE('',*,*,#11198,.F.);
#15068=ORIENTED_EDGE('',*,*,#11171,.T.);
#15069=ORIENTED_EDGE('',*,*,#11199,.F.);
#15070=ORIENTED_EDGE('',*,*,#11200,.F.);
#15071=ORIENTED_EDGE('',*,*,#11201,.F.);
#15072=ORIENTED_EDGE('',*,*,#11202,.F.);
#15073=ORIENTED_EDGE('',*,*,#11203,.F.);
#15074=ORIENTED_EDGE('',*,*,#11204,.F.);
#15075=ORIENTED_EDGE('',*,*,#11205,.F.);
#15076=ORIENTED_EDGE('',*,*,#11206,.F.);
#15077=ORIENTED_EDGE('',*,*,#11207,.F.);
#15078=ORIENTED_EDGE('',*,*,#11208,.T.);
#15079=ORIENTED_EDGE('',*,*,#11206,.T.);
#15080=ORIENTED_EDGE('',*,*,#11208,.F.);
#15081=ORIENTED_EDGE('',*,*,#11209,.F.);
#15082=ORIENTED_EDGE('',*,*,#11210,.T.);
#15083=ORIENTED_EDGE('',*,*,#11207,.T.);
#15084=ORIENTED_EDGE('',*,*,#11210,.F.);
#15085=ORIENTED_EDGE('',*,*,#11211,.F.);
#15086=ORIENTED_EDGE('',*,*,#11212,.T.);
#15087=ORIENTED_EDGE('',*,*,#11209,.T.);
#15088=ORIENTED_EDGE('',*,*,#11212,.F.);
#15089=ORIENTED_EDGE('',*,*,#11211,.T.);
#15090=ORIENTED_EDGE('',*,*,#11213,.F.);
#15091=ORIENTED_EDGE('',*,*,#11214,.F.);
#15092=ORIENTED_EDGE('',*,*,#11215,.T.);
#15093=ORIENTED_EDGE('',*,*,#11213,.T.);
#15094=ORIENTED_EDGE('',*,*,#11215,.F.);
#15095=ORIENTED_EDGE('',*,*,#11199,.T.);
#15096=ORIENTED_EDGE('',*,*,#11216,.T.);
#15097=ORIENTED_EDGE('',*,*,#11214,.T.);
#15098=ORIENTED_EDGE('',*,*,#11216,.F.);
#15099=ORIENTED_EDGE('',*,*,#11217,.T.);
#15100=ORIENTED_EDGE('',*,*,#11218,.T.);
#15101=ORIENTED_EDGE('',*,*,#11200,.T.);
#15102=ORIENTED_EDGE('',*,*,#11219,.F.);
#15103=ORIENTED_EDGE('',*,*,#11220,.T.);
#15104=ORIENTED_EDGE('',*,*,#11221,.T.);
#15105=ORIENTED_EDGE('',*,*,#11201,.T.);
#15106=ORIENTED_EDGE('',*,*,#11218,.F.);
#15107=ORIENTED_EDGE('',*,*,#11222,.T.);
#15108=ORIENTED_EDGE('',*,*,#11223,.T.);
#15109=ORIENTED_EDGE('',*,*,#11202,.T.);
#15110=ORIENTED_EDGE('',*,*,#11221,.F.);
#15111=ORIENTED_EDGE('',*,*,#11224,.T.);
#15112=ORIENTED_EDGE('',*,*,#11225,.T.);
#15113=ORIENTED_EDGE('',*,*,#11203,.T.);
#15114=ORIENTED_EDGE('',*,*,#11223,.F.);
#15115=ORIENTED_EDGE('',*,*,#11226,.T.);
#15116=ORIENTED_EDGE('',*,*,#11227,.T.);
#15117=ORIENTED_EDGE('',*,*,#11204,.T.);
#15118=ORIENTED_EDGE('',*,*,#11225,.F.);
#15119=ORIENTED_EDGE('',*,*,#11228,.T.);
#15120=ORIENTED_EDGE('',*,*,#11219,.T.);
#15121=ORIENTED_EDGE('',*,*,#11205,.T.);
#15122=ORIENTED_EDGE('',*,*,#11227,.F.);
#15123=ORIENTED_EDGE('',*,*,#11228,.F.);
#15124=ORIENTED_EDGE('',*,*,#11226,.F.);
#15125=ORIENTED_EDGE('',*,*,#11224,.F.);
#15126=ORIENTED_EDGE('',*,*,#11222,.F.);
#15127=ORIENTED_EDGE('',*,*,#11220,.F.);
#15128=ORIENTED_EDGE('',*,*,#11217,.F.);
#15129=ORIENTED_EDGE('',*,*,#11229,.F.);
#15130=ORIENTED_EDGE('',*,*,#11230,.T.);
#15131=ORIENTED_EDGE('',*,*,#11231,.F.);
#15132=ORIENTED_EDGE('',*,*,#11230,.F.);
#15133=ORIENTED_EDGE('',*,*,#11232,.F.);
#15134=ORIENTED_EDGE('',*,*,#11233,.T.);
#15135=ORIENTED_EDGE('',*,*,#11234,.F.);
#15136=ORIENTED_EDGE('',*,*,#11233,.F.);
#15137=ORIENTED_EDGE('',*,*,#11235,.F.);
#15138=ORIENTED_EDGE('',*,*,#11236,.T.);
#15139=ORIENTED_EDGE('',*,*,#11237,.F.);
#15140=ORIENTED_EDGE('',*,*,#11236,.F.);
#15141=ORIENTED_EDGE('',*,*,#11238,.F.);
#15142=ORIENTED_EDGE('',*,*,#11239,.T.);
#15143=ORIENTED_EDGE('',*,*,#11240,.F.);
#15144=ORIENTED_EDGE('',*,*,#11239,.F.);
#15145=ORIENTED_EDGE('',*,*,#11241,.F.);
#15146=ORIENTED_EDGE('',*,*,#11242,.T.);
#15147=ORIENTED_EDGE('',*,*,#11243,.F.);
#15148=ORIENTED_EDGE('',*,*,#11242,.F.);
#15149=ORIENTED_EDGE('',*,*,#11244,.F.);
#15150=ORIENTED_EDGE('',*,*,#11245,.T.);
#15151=ORIENTED_EDGE('',*,*,#11246,.F.);
#15152=ORIENTED_EDGE('',*,*,#11245,.F.);
#15153=ORIENTED_EDGE('',*,*,#11247,.F.);
#15154=ORIENTED_EDGE('',*,*,#11248,.T.);
#15155=ORIENTED_EDGE('',*,*,#11249,.F.);
#15156=ORIENTED_EDGE('',*,*,#11248,.F.);
#15157=ORIENTED_EDGE('',*,*,#11250,.F.);
#15158=ORIENTED_EDGE('',*,*,#11251,.T.);
#15159=ORIENTED_EDGE('',*,*,#11252,.F.);
#15160=ORIENTED_EDGE('',*,*,#11251,.F.);
#15161=ORIENTED_EDGE('',*,*,#11253,.F.);
#15162=ORIENTED_EDGE('',*,*,#11254,.T.);
#15163=ORIENTED_EDGE('',*,*,#11255,.F.);
#15164=ORIENTED_EDGE('',*,*,#11254,.F.);
#15165=ORIENTED_EDGE('',*,*,#11256,.F.);
#15166=ORIENTED_EDGE('',*,*,#11257,.T.);
#15167=ORIENTED_EDGE('',*,*,#11258,.F.);
#15168=ORIENTED_EDGE('',*,*,#11257,.F.);
#15169=ORIENTED_EDGE('',*,*,#11259,.F.);
#15170=ORIENTED_EDGE('',*,*,#11260,.T.);
#15171=ORIENTED_EDGE('',*,*,#11261,.F.);
#15172=ORIENTED_EDGE('',*,*,#11260,.F.);
#15173=ORIENTED_EDGE('',*,*,#11262,.F.);
#15174=ORIENTED_EDGE('',*,*,#11263,.T.);
#15175=ORIENTED_EDGE('',*,*,#11264,.F.);
#15176=ORIENTED_EDGE('',*,*,#11263,.F.);
#15177=ORIENTED_EDGE('',*,*,#11265,.F.);
#15178=ORIENTED_EDGE('',*,*,#11266,.T.);
#15179=ORIENTED_EDGE('',*,*,#11267,.F.);
#15180=ORIENTED_EDGE('',*,*,#11266,.F.);
#15181=ORIENTED_EDGE('',*,*,#11268,.F.);
#15182=ORIENTED_EDGE('',*,*,#11269,.T.);
#15183=ORIENTED_EDGE('',*,*,#11270,.F.);
#15184=ORIENTED_EDGE('',*,*,#11269,.F.);
#15185=ORIENTED_EDGE('',*,*,#11271,.F.);
#15186=ORIENTED_EDGE('',*,*,#11272,.T.);
#15187=ORIENTED_EDGE('',*,*,#11273,.F.);
#15188=ORIENTED_EDGE('',*,*,#11272,.F.);
#15189=ORIENTED_EDGE('',*,*,#11274,.F.);
#15190=ORIENTED_EDGE('',*,*,#11275,.T.);
#15191=ORIENTED_EDGE('',*,*,#11276,.F.);
#15192=ORIENTED_EDGE('',*,*,#11275,.F.);
#15193=ORIENTED_EDGE('',*,*,#11277,.F.);
#15194=ORIENTED_EDGE('',*,*,#11278,.T.);
#15195=ORIENTED_EDGE('',*,*,#11279,.F.);
#15196=ORIENTED_EDGE('',*,*,#11278,.F.);
#15197=ORIENTED_EDGE('',*,*,#11280,.F.);
#15198=ORIENTED_EDGE('',*,*,#11281,.T.);
#15199=ORIENTED_EDGE('',*,*,#11282,.F.);
#15200=ORIENTED_EDGE('',*,*,#11281,.F.);
#15201=ORIENTED_EDGE('',*,*,#11283,.T.);
#15202=ORIENTED_EDGE('',*,*,#11284,.T.);
#15203=ORIENTED_EDGE('',*,*,#11285,.F.);
#15204=ORIENTED_EDGE('',*,*,#11286,.F.);
#15205=ORIENTED_EDGE('',*,*,#11287,.T.);
#15206=ORIENTED_EDGE('',*,*,#11286,.T.);
#15207=ORIENTED_EDGE('',*,*,#11288,.F.);
#15208=ORIENTED_EDGE('',*,*,#11289,.F.);
#15209=ORIENTED_EDGE('',*,*,#11290,.T.);
#15210=ORIENTED_EDGE('',*,*,#11289,.T.);
#15211=ORIENTED_EDGE('',*,*,#11291,.F.);
#15212=ORIENTED_EDGE('',*,*,#11292,.F.);
#15213=ORIENTED_EDGE('',*,*,#11293,.T.);
#15214=ORIENTED_EDGE('',*,*,#11292,.T.);
#15215=ORIENTED_EDGE('',*,*,#11294,.F.);
#15216=ORIENTED_EDGE('',*,*,#11284,.F.);
#15217=ORIENTED_EDGE('',*,*,#11294,.T.);
#15218=ORIENTED_EDGE('',*,*,#11291,.T.);
#15219=ORIENTED_EDGE('',*,*,#11288,.T.);
#15220=ORIENTED_EDGE('',*,*,#11285,.T.);
#15221=ORIENTED_EDGE('',*,*,#11237,.T.);
#15222=ORIENTED_EDGE('',*,*,#11240,.T.);
#15223=ORIENTED_EDGE('',*,*,#11252,.T.);
#15224=ORIENTED_EDGE('',*,*,#11255,.T.);
#15225=ORIENTED_EDGE('',*,*,#11258,.T.);
#15226=ORIENTED_EDGE('',*,*,#11261,.T.);
#15227=ORIENTED_EDGE('',*,*,#11282,.T.);
#15228=ORIENTED_EDGE('',*,*,#11279,.T.);
#15229=ORIENTED_EDGE('',*,*,#11276,.T.);
#15230=ORIENTED_EDGE('',*,*,#11273,.T.);
#15231=ORIENTED_EDGE('',*,*,#11270,.T.);
#15232=ORIENTED_EDGE('',*,*,#11267,.T.);
#15233=ORIENTED_EDGE('',*,*,#11264,.T.);
#15234=ORIENTED_EDGE('',*,*,#11249,.T.);
#15235=ORIENTED_EDGE('',*,*,#11246,.T.);
#15236=ORIENTED_EDGE('',*,*,#11243,.T.);
#15237=ORIENTED_EDGE('',*,*,#11234,.T.);
#15238=ORIENTED_EDGE('',*,*,#11231,.T.);
#15239=ORIENTED_EDGE('',*,*,#11293,.F.);
#15240=ORIENTED_EDGE('',*,*,#11283,.F.);
#15241=ORIENTED_EDGE('',*,*,#11287,.F.);
#15242=ORIENTED_EDGE('',*,*,#11290,.F.);
#15243=ORIENTED_EDGE('',*,*,#11235,.T.);
#15244=ORIENTED_EDGE('',*,*,#11238,.T.);
#15245=ORIENTED_EDGE('',*,*,#11250,.T.);
#15246=ORIENTED_EDGE('',*,*,#11253,.T.);
#15247=ORIENTED_EDGE('',*,*,#11256,.T.);
#15248=ORIENTED_EDGE('',*,*,#11259,.T.);
#15249=ORIENTED_EDGE('',*,*,#11280,.T.);
#15250=ORIENTED_EDGE('',*,*,#11277,.T.);
#15251=ORIENTED_EDGE('',*,*,#11274,.T.);
#15252=ORIENTED_EDGE('',*,*,#11271,.T.);
#15253=ORIENTED_EDGE('',*,*,#11268,.T.);
#15254=ORIENTED_EDGE('',*,*,#11265,.T.);
#15255=ORIENTED_EDGE('',*,*,#11262,.T.);
#15256=ORIENTED_EDGE('',*,*,#11247,.T.);
#15257=ORIENTED_EDGE('',*,*,#11244,.T.);
#15258=ORIENTED_EDGE('',*,*,#11241,.T.);
#15259=ORIENTED_EDGE('',*,*,#11232,.T.);
#15260=ORIENTED_EDGE('',*,*,#11229,.T.);
#15261=ORIENTED_EDGE('',*,*,#11295,.F.);
#15262=ORIENTED_EDGE('',*,*,#11296,.T.);
#15263=ORIENTED_EDGE('',*,*,#11297,.F.);
#15264=ORIENTED_EDGE('',*,*,#11298,.F.);
#15265=ORIENTED_EDGE('',*,*,#11299,.T.);
#15266=ORIENTED_EDGE('',*,*,#11300,.F.);
#15267=ORIENTED_EDGE('',*,*,#11299,.F.);
#15268=ORIENTED_EDGE('',*,*,#11301,.F.);
#15269=ORIENTED_EDGE('',*,*,#11302,.F.);
#15270=ORIENTED_EDGE('',*,*,#11296,.F.);
#15271=ORIENTED_EDGE('',*,*,#11303,.F.);
#15272=ORIENTED_EDGE('',*,*,#11304,.T.);
#15273=ORIENTED_EDGE('',*,*,#11305,.F.);
#15274=ORIENTED_EDGE('',*,*,#11306,.F.);
#15275=ORIENTED_EDGE('',*,*,#11307,.T.);
#15276=ORIENTED_EDGE('',*,*,#11308,.F.);
#15277=ORIENTED_EDGE('',*,*,#11307,.F.);
#15278=ORIENTED_EDGE('',*,*,#11309,.F.);
#15279=ORIENTED_EDGE('',*,*,#11310,.F.);
#15280=ORIENTED_EDGE('',*,*,#11304,.F.);
#15281=ORIENTED_EDGE('',*,*,#11311,.F.);
#15282=ORIENTED_EDGE('',*,*,#11312,.T.);
#15283=ORIENTED_EDGE('',*,*,#11313,.T.);
#15284=ORIENTED_EDGE('',*,*,#11314,.F.);
#15285=ORIENTED_EDGE('',*,*,#11315,.F.);
#15286=ORIENTED_EDGE('',*,*,#11316,.F.);
#15287=ORIENTED_EDGE('',*,*,#11313,.F.);
#15288=ORIENTED_EDGE('',*,*,#11317,.T.);
#15289=ORIENTED_EDGE('',*,*,#11318,.F.);
#15290=ORIENTED_EDGE('',*,*,#11317,.F.);
#15291=ORIENTED_EDGE('',*,*,#11312,.F.);
#15292=ORIENTED_EDGE('',*,*,#11319,.F.);
#15293=ORIENTED_EDGE('',*,*,#11320,.T.);
#15294=ORIENTED_EDGE('',*,*,#11321,.T.);
#15295=ORIENTED_EDGE('',*,*,#11322,.F.);
#15296=ORIENTED_EDGE('',*,*,#11323,.F.);
#15297=ORIENTED_EDGE('',*,*,#11324,.F.);
#15298=ORIENTED_EDGE('',*,*,#11321,.F.);
#15299=ORIENTED_EDGE('',*,*,#11325,.T.);
#15300=ORIENTED_EDGE('',*,*,#11326,.F.);
#15301=ORIENTED_EDGE('',*,*,#11325,.F.);
#15302=ORIENTED_EDGE('',*,*,#11320,.F.);
#15303=ORIENTED_EDGE('',*,*,#11297,.T.);
#15304=ORIENTED_EDGE('',*,*,#11295,.T.);
#15305=ORIENTED_EDGE('',*,*,#11302,.T.);
#15306=ORIENTED_EDGE('',*,*,#11327,.T.);
#15307=ORIENTED_EDGE('',*,*,#11328,.T.);
#15308=ORIENTED_EDGE('',*,*,#11329,.T.);
#15309=ORIENTED_EDGE('',*,*,#11328,.F.);
#15310=ORIENTED_EDGE('',*,*,#11330,.T.);
#15311=ORIENTED_EDGE('',*,*,#11305,.T.);
#15312=ORIENTED_EDGE('',*,*,#11303,.T.);
#15313=ORIENTED_EDGE('',*,*,#11310,.T.);
#15314=ORIENTED_EDGE('',*,*,#11331,.T.);
#15315=ORIENTED_EDGE('',*,*,#11314,.T.);
#15316=ORIENTED_EDGE('',*,*,#11311,.T.);
#15317=ORIENTED_EDGE('',*,*,#11316,.T.);
#15318=ORIENTED_EDGE('',*,*,#11332,.T.);
#15319=ORIENTED_EDGE('',*,*,#11322,.T.);
#15320=ORIENTED_EDGE('',*,*,#11319,.T.);
#15321=ORIENTED_EDGE('',*,*,#11324,.T.);
#15322=ORIENTED_EDGE('',*,*,#11333,.T.);
#15323=ORIENTED_EDGE('',*,*,#11334,.F.);
#15324=ORIENTED_EDGE('',*,*,#11335,.T.);
#15325=ORIENTED_EDGE('',*,*,#11336,.F.);
#15326=ORIENTED_EDGE('',*,*,#11335,.F.);
#15327=ORIENTED_EDGE('',*,*,#11334,.T.);
#15328=ORIENTED_EDGE('',*,*,#11337,.F.);
#15329=ORIENTED_EDGE('',*,*,#11338,.F.);
#15330=ORIENTED_EDGE('',*,*,#11301,.T.);
#15331=ORIENTED_EDGE('',*,*,#11298,.T.);
#15332=ORIENTED_EDGE('',*,*,#11333,.F.);
#15333=ORIENTED_EDGE('',*,*,#11323,.T.);
#15334=ORIENTED_EDGE('',*,*,#11332,.F.);
#15335=ORIENTED_EDGE('',*,*,#11315,.T.);
#15336=ORIENTED_EDGE('',*,*,#11331,.F.);
#15337=ORIENTED_EDGE('',*,*,#11309,.T.);
#15338=ORIENTED_EDGE('',*,*,#11306,.T.);
#15339=ORIENTED_EDGE('',*,*,#11330,.F.);
#15340=ORIENTED_EDGE('',*,*,#11327,.F.);
#15341=ORIENTED_EDGE('',*,*,#11339,.F.);
#15342=ORIENTED_EDGE('',*,*,#11340,.T.);
#15343=ORIENTED_EDGE('',*,*,#11338,.T.);
#15344=ORIENTED_EDGE('',*,*,#11340,.F.);
#15345=ORIENTED_EDGE('',*,*,#11337,.T.);
#15346=ORIENTED_EDGE('',*,*,#11341,.T.);
#15347=ORIENTED_EDGE('',*,*,#11342,.T.);
#15348=ORIENTED_EDGE('',*,*,#11341,.F.);
#15349=ORIENTED_EDGE('',*,*,#11339,.T.);
#15350=ORIENTED_EDGE('',*,*,#11336,.T.);
#15351=ORIENTED_EDGE('',*,*,#11326,.T.);
#15352=ORIENTED_EDGE('',*,*,#11318,.T.);
#15353=ORIENTED_EDGE('',*,*,#11308,.T.);
#15354=ORIENTED_EDGE('',*,*,#11300,.T.);
#15355=ORIENTED_EDGE('',*,*,#11329,.F.);
#15356=ORIENTED_EDGE('',*,*,#11342,.F.);
#15357=ORIENTED_EDGE('',*,*,#11343,.F.);
#15358=ORIENTED_EDGE('',*,*,#11344,.T.);
#15359=ORIENTED_EDGE('',*,*,#11345,.F.);
#15360=ORIENTED_EDGE('',*,*,#11346,.F.);
#15361=ORIENTED_EDGE('',*,*,#11347,.T.);
#15362=ORIENTED_EDGE('',*,*,#11348,.F.);
#15363=ORIENTED_EDGE('',*,*,#11347,.F.);
#15364=ORIENTED_EDGE('',*,*,#11349,.F.);
#15365=ORIENTED_EDGE('',*,*,#11350,.F.);
#15366=ORIENTED_EDGE('',*,*,#11344,.F.);
#15367=ORIENTED_EDGE('',*,*,#11351,.F.);
#15368=ORIENTED_EDGE('',*,*,#11352,.T.);
#15369=ORIENTED_EDGE('',*,*,#11353,.F.);
#15370=ORIENTED_EDGE('',*,*,#11354,.F.);
#15371=ORIENTED_EDGE('',*,*,#11355,.T.);
#15372=ORIENTED_EDGE('',*,*,#11356,.F.);
#15373=ORIENTED_EDGE('',*,*,#11355,.F.);
#15374=ORIENTED_EDGE('',*,*,#11357,.F.);
#15375=ORIENTED_EDGE('',*,*,#11358,.F.);
#15376=ORIENTED_EDGE('',*,*,#11352,.F.);
#15377=ORIENTED_EDGE('',*,*,#11359,.F.);
#15378=ORIENTED_EDGE('',*,*,#11360,.T.);
#15379=ORIENTED_EDGE('',*,*,#11361,.T.);
#15380=ORIENTED_EDGE('',*,*,#11362,.F.);
#15381=ORIENTED_EDGE('',*,*,#11363,.F.);
#15382=ORIENTED_EDGE('',*,*,#11364,.F.);
#15383=ORIENTED_EDGE('',*,*,#11361,.F.);
#15384=ORIENTED_EDGE('',*,*,#11365,.T.);
#15385=ORIENTED_EDGE('',*,*,#11366,.F.);
#15386=ORIENTED_EDGE('',*,*,#11365,.F.);
#15387=ORIENTED_EDGE('',*,*,#11360,.F.);
#15388=ORIENTED_EDGE('',*,*,#11367,.F.);
#15389=ORIENTED_EDGE('',*,*,#11368,.T.);
#15390=ORIENTED_EDGE('',*,*,#11369,.T.);
#15391=ORIENTED_EDGE('',*,*,#11370,.F.);
#15392=ORIENTED_EDGE('',*,*,#11371,.F.);
#15393=ORIENTED_EDGE('',*,*,#11372,.F.);
#15394=ORIENTED_EDGE('',*,*,#11369,.F.);
#15395=ORIENTED_EDGE('',*,*,#11373,.T.);
#15396=ORIENTED_EDGE('',*,*,#11374,.F.);
#15397=ORIENTED_EDGE('',*,*,#11373,.F.);
#15398=ORIENTED_EDGE('',*,*,#11368,.F.);
#15399=ORIENTED_EDGE('',*,*,#11345,.T.);
#15400=ORIENTED_EDGE('',*,*,#11343,.T.);
#15401=ORIENTED_EDGE('',*,*,#11350,.T.);
#15402=ORIENTED_EDGE('',*,*,#11375,.T.);
#15403=ORIENTED_EDGE('',*,*,#11376,.T.);
#15404=ORIENTED_EDGE('',*,*,#11377,.T.);
#15405=ORIENTED_EDGE('',*,*,#11376,.F.);
#15406=ORIENTED_EDGE('',*,*,#11378,.T.);
#15407=ORIENTED_EDGE('',*,*,#11353,.T.);
#15408=ORIENTED_EDGE('',*,*,#11351,.T.);
#15409=ORIENTED_EDGE('',*,*,#11358,.T.);
#15410=ORIENTED_EDGE('',*,*,#11379,.T.);
#15411=ORIENTED_EDGE('',*,*,#11362,.T.);
#15412=ORIENTED_EDGE('',*,*,#11359,.T.);
#15413=ORIENTED_EDGE('',*,*,#11364,.T.);
#15414=ORIENTED_EDGE('',*,*,#11380,.T.);
#15415=ORIENTED_EDGE('',*,*,#11370,.T.);
#15416=ORIENTED_EDGE('',*,*,#11367,.T.);
#15417=ORIENTED_EDGE('',*,*,#11372,.T.);
#15418=ORIENTED_EDGE('',*,*,#11381,.T.);
#15419=ORIENTED_EDGE('',*,*,#11382,.F.);
#15420=ORIENTED_EDGE('',*,*,#11383,.T.);
#15421=ORIENTED_EDGE('',*,*,#11384,.F.);
#15422=ORIENTED_EDGE('',*,*,#11383,.F.);
#15423=ORIENTED_EDGE('',*,*,#11382,.T.);
#15424=ORIENTED_EDGE('',*,*,#11385,.F.);
#15425=ORIENTED_EDGE('',*,*,#11386,.F.);
#15426=ORIENTED_EDGE('',*,*,#11349,.T.);
#15427=ORIENTED_EDGE('',*,*,#11346,.T.);
#15428=ORIENTED_EDGE('',*,*,#11381,.F.);
#15429=ORIENTED_EDGE('',*,*,#11371,.T.);
#15430=ORIENTED_EDGE('',*,*,#11380,.F.);
#15431=ORIENTED_EDGE('',*,*,#11363,.T.);
#15432=ORIENTED_EDGE('',*,*,#11379,.F.);
#15433=ORIENTED_EDGE('',*,*,#11357,.T.);
#15434=ORIENTED_EDGE('',*,*,#11354,.T.);
#15435=ORIENTED_EDGE('',*,*,#11378,.F.);
#15436=ORIENTED_EDGE('',*,*,#11375,.F.);
#15437=ORIENTED_EDGE('',*,*,#11387,.F.);
#15438=ORIENTED_EDGE('',*,*,#11388,.T.);
#15439=ORIENTED_EDGE('',*,*,#11386,.T.);
#15440=ORIENTED_EDGE('',*,*,#11388,.F.);
#15441=ORIENTED_EDGE('',*,*,#11385,.T.);
#15442=ORIENTED_EDGE('',*,*,#11389,.T.);
#15443=ORIENTED_EDGE('',*,*,#11390,.T.);
#15444=ORIENTED_EDGE('',*,*,#11389,.F.);
#15445=ORIENTED_EDGE('',*,*,#11387,.T.);
#15446=ORIENTED_EDGE('',*,*,#11384,.T.);
#15447=ORIENTED_EDGE('',*,*,#11374,.T.);
#15448=ORIENTED_EDGE('',*,*,#11366,.T.);
#15449=ORIENTED_EDGE('',*,*,#11356,.T.);
#15450=ORIENTED_EDGE('',*,*,#11348,.T.);
#15451=ORIENTED_EDGE('',*,*,#11377,.F.);
#15452=ORIENTED_EDGE('',*,*,#11390,.F.);
#15453=ORIENTED_EDGE('',*,*,#11391,.F.);
#15454=ORIENTED_EDGE('',*,*,#11392,.T.);
#15455=ORIENTED_EDGE('',*,*,#11393,.F.);
#15456=ORIENTED_EDGE('',*,*,#11392,.F.);
#15457=ORIENTED_EDGE('',*,*,#11391,.T.);
#15458=ORIENTED_EDGE('',*,*,#11394,.F.);
#15459=ORIENTED_EDGE('',*,*,#11395,.T.);
#15460=ORIENTED_EDGE('',*,*,#11396,.F.);
#15461=ORIENTED_EDGE('',*,*,#11395,.F.);
#15462=ORIENTED_EDGE('',*,*,#11394,.T.);
#15463=ORIENTED_EDGE('',*,*,#11397,.F.);
#15464=ORIENTED_EDGE('',*,*,#11398,.T.);
#15465=ORIENTED_EDGE('',*,*,#11399,.F.);
#15466=ORIENTED_EDGE('',*,*,#11398,.F.);
#15467=ORIENTED_EDGE('',*,*,#11397,.T.);
#15468=ORIENTED_EDGE('',*,*,#11400,.F.);
#15469=ORIENTED_EDGE('',*,*,#11401,.T.);
#15470=ORIENTED_EDGE('',*,*,#11402,.T.);
#15471=ORIENTED_EDGE('',*,*,#11401,.F.);
#15472=ORIENTED_EDGE('',*,*,#11403,.F.);
#15473=ORIENTED_EDGE('',*,*,#11404,.T.);
#15474=ORIENTED_EDGE('',*,*,#11405,.T.);
#15475=ORIENTED_EDGE('',*,*,#11404,.F.);
#15476=ORIENTED_EDGE('',*,*,#11403,.T.);
#15477=ORIENTED_EDGE('',*,*,#11393,.T.);
#15478=ORIENTED_EDGE('',*,*,#11396,.T.);
#15479=ORIENTED_EDGE('',*,*,#11399,.T.);
#15480=ORIENTED_EDGE('',*,*,#11400,.T.);
#15481=ORIENTED_EDGE('',*,*,#11405,.F.);
#15482=ORIENTED_EDGE('',*,*,#11402,.F.);
#15483=ORIENTED_EDGE('',*,*,#11406,.F.);
#15484=ORIENTED_EDGE('',*,*,#11407,.T.);
#15485=ORIENTED_EDGE('',*,*,#11408,.F.);
#15486=ORIENTED_EDGE('',*,*,#11407,.F.);
#15487=ORIENTED_EDGE('',*,*,#11409,.F.);
#15488=ORIENTED_EDGE('',*,*,#11410,.T.);
#15489=ORIENTED_EDGE('',*,*,#11411,.F.);
#15490=ORIENTED_EDGE('',*,*,#11410,.F.);
#15491=ORIENTED_EDGE('',*,*,#11412,.F.);
#15492=ORIENTED_EDGE('',*,*,#11413,.T.);
#15493=ORIENTED_EDGE('',*,*,#11414,.T.);
#15494=ORIENTED_EDGE('',*,*,#11413,.F.);
#15495=ORIENTED_EDGE('',*,*,#11412,.T.);
#15496=ORIENTED_EDGE('',*,*,#11408,.T.);
#15497=ORIENTED_EDGE('',*,*,#11411,.T.);
#15498=ORIENTED_EDGE('',*,*,#11414,.F.);
#15499=ORIENTED_EDGE('',*,*,#11406,.T.);
#15500=ORIENTED_EDGE('',*,*,#11409,.T.);
#15501=ORIENTED_EDGE('',*,*,#11415,.F.);
#15502=ORIENTED_EDGE('',*,*,#11416,.T.);
#15503=ORIENTED_EDGE('',*,*,#11417,.F.);
#15504=ORIENTED_EDGE('',*,*,#11416,.F.);
#15505=ORIENTED_EDGE('',*,*,#11418,.F.);
#15506=ORIENTED_EDGE('',*,*,#11419,.T.);
#15507=ORIENTED_EDGE('',*,*,#11420,.F.);
#15508=ORIENTED_EDGE('',*,*,#11419,.F.);
#15509=ORIENTED_EDGE('',*,*,#11421,.T.);
#15510=ORIENTED_EDGE('',*,*,#11422,.F.);
#15511=ORIENTED_EDGE('',*,*,#11423,.F.);
#15512=ORIENTED_EDGE('',*,*,#11424,.F.);
#15513=ORIENTED_EDGE('',*,*,#11425,.T.);
#15514=ORIENTED_EDGE('',*,*,#11424,.T.);
#15515=ORIENTED_EDGE('',*,*,#11426,.F.);
#15516=ORIENTED_EDGE('',*,*,#11427,.F.);
#15517=ORIENTED_EDGE('',*,*,#11428,.F.);
#15518=ORIENTED_EDGE('',*,*,#11426,.T.);
#15519=ORIENTED_EDGE('',*,*,#11423,.T.);
#15520=ORIENTED_EDGE('',*,*,#11429,.F.);
#15521=ORIENTED_EDGE('',*,*,#11430,.T.);
#15522=ORIENTED_EDGE('',*,*,#11431,.T.);
#15523=ORIENTED_EDGE('',*,*,#11432,.F.);
#15524=ORIENTED_EDGE('',*,*,#11433,.F.);
#15525=ORIENTED_EDGE('',*,*,#11434,.F.);
#15526=ORIENTED_EDGE('',*,*,#11435,.F.);
#15527=ORIENTED_EDGE('',*,*,#11430,.F.);
#15528=ORIENTED_EDGE('',*,*,#11415,.T.);
#15529=ORIENTED_EDGE('',*,*,#11418,.T.);
#15530=ORIENTED_EDGE('',*,*,#11436,.F.);
#15531=ORIENTED_EDGE('',*,*,#11437,.F.);
#15532=ORIENTED_EDGE('',*,*,#11438,.F.);
#15533=ORIENTED_EDGE('',*,*,#11434,.T.);
#15534=ORIENTED_EDGE('',*,*,#11435,.T.);
#15535=ORIENTED_EDGE('',*,*,#11438,.T.);
#15536=ORIENTED_EDGE('',*,*,#11439,.F.);
#15537=ORIENTED_EDGE('',*,*,#11431,.F.);
#15538=ORIENTED_EDGE('',*,*,#11422,.T.);
#15539=ORIENTED_EDGE('',*,*,#11440,.T.);
#15540=ORIENTED_EDGE('',*,*,#11441,.T.);
#15541=ORIENTED_EDGE('',*,*,#11442,.F.);
#15542=ORIENTED_EDGE('',*,*,#11443,.F.);
#15543=ORIENTED_EDGE('',*,*,#11444,.T.);
#15544=ORIENTED_EDGE('',*,*,#11427,.T.);
#15545=ORIENTED_EDGE('',*,*,#11428,.T.);
#15546=ORIENTED_EDGE('',*,*,#11445,.T.);
#15547=ORIENTED_EDGE('',*,*,#11446,.T.);
#15548=ORIENTED_EDGE('',*,*,#11447,.F.);
#15549=ORIENTED_EDGE('',*,*,#11441,.F.);
#15550=ORIENTED_EDGE('',*,*,#11448,.T.);
#15551=ORIENTED_EDGE('',*,*,#11443,.T.);
#15552=ORIENTED_EDGE('',*,*,#11449,.F.);
#15553=ORIENTED_EDGE('',*,*,#11450,.F.);
#15554=ORIENTED_EDGE('',*,*,#11429,.T.);
#15555=ORIENTED_EDGE('',*,*,#11451,.F.);
#15556=ORIENTED_EDGE('',*,*,#11446,.F.);
#15557=ORIENTED_EDGE('',*,*,#11452,.T.);
#15558=ORIENTED_EDGE('',*,*,#11450,.T.);
#15559=ORIENTED_EDGE('',*,*,#11453,.F.);
#15560=ORIENTED_EDGE('',*,*,#11436,.T.);
#15561=ORIENTED_EDGE('',*,*,#11433,.T.);
#15562=ORIENTED_EDGE('',*,*,#11442,.T.);
#15563=ORIENTED_EDGE('',*,*,#11447,.T.);
#15564=ORIENTED_EDGE('',*,*,#11451,.T.);
#15565=ORIENTED_EDGE('',*,*,#11432,.T.);
#15566=ORIENTED_EDGE('',*,*,#11439,.T.);
#15567=ORIENTED_EDGE('',*,*,#11437,.T.);
#15568=ORIENTED_EDGE('',*,*,#11453,.T.);
#15569=ORIENTED_EDGE('',*,*,#11449,.T.);
#15570=ORIENTED_EDGE('',*,*,#11417,.T.);
#15571=ORIENTED_EDGE('',*,*,#11420,.T.);
#15572=ORIENTED_EDGE('',*,*,#11452,.F.);
#15573=ORIENTED_EDGE('',*,*,#11445,.F.);
#15574=ORIENTED_EDGE('',*,*,#11440,.F.);
#15575=ORIENTED_EDGE('',*,*,#11421,.F.);
#15576=ORIENTED_EDGE('',*,*,#11425,.F.);
#15577=ORIENTED_EDGE('',*,*,#11444,.F.);
#15578=ORIENTED_EDGE('',*,*,#11448,.F.);
#15579=ORIENTED_EDGE('',*,*,#11454,.F.);
#15580=ORIENTED_EDGE('',*,*,#11455,.F.);
#15581=ORIENTED_EDGE('',*,*,#11456,.F.);
#15582=ORIENTED_EDGE('',*,*,#11457,.F.);
#15583=ORIENTED_EDGE('',*,*,#11458,.F.);
#15584=ORIENTED_EDGE('',*,*,#11457,.T.);
#15585=ORIENTED_EDGE('',*,*,#11459,.F.);
#15586=ORIENTED_EDGE('',*,*,#11460,.T.);
#15587=ORIENTED_EDGE('',*,*,#11461,.F.);
#15588=ORIENTED_EDGE('',*,*,#11460,.F.);
#15589=ORIENTED_EDGE('',*,*,#11462,.F.);
#15590=ORIENTED_EDGE('',*,*,#11463,.F.);
#15591=ORIENTED_EDGE('',*,*,#11464,.F.);
#15592=ORIENTED_EDGE('',*,*,#11463,.T.);
#15593=ORIENTED_EDGE('',*,*,#11465,.T.);
#15594=ORIENTED_EDGE('',*,*,#11455,.T.);
#15595=ORIENTED_EDGE('',*,*,#11465,.F.);
#15596=ORIENTED_EDGE('',*,*,#11462,.T.);
#15597=ORIENTED_EDGE('',*,*,#11459,.T.);
#15598=ORIENTED_EDGE('',*,*,#11456,.T.);
#15599=ORIENTED_EDGE('',*,*,#11466,.F.);
#15600=ORIENTED_EDGE('',*,*,#11467,.T.);
#15601=ORIENTED_EDGE('',*,*,#11468,.F.);
#15602=ORIENTED_EDGE('',*,*,#11469,.T.);
#15603=ORIENTED_EDGE('',*,*,#11466,.T.);
#15604=ORIENTED_EDGE('',*,*,#11469,.F.);
#15605=ORIENTED_EDGE('',*,*,#11468,.T.);
#15606=ORIENTED_EDGE('',*,*,#11470,.F.);
#15607=ORIENTED_EDGE('',*,*,#11471,.F.);
#15608=ORIENTED_EDGE('',*,*,#11472,.T.);
#15609=ORIENTED_EDGE('',*,*,#11470,.T.);
#15610=ORIENTED_EDGE('',*,*,#11472,.F.);
#15611=ORIENTED_EDGE('',*,*,#11473,.F.);
#15612=ORIENTED_EDGE('',*,*,#11471,.T.);
#15613=ORIENTED_EDGE('',*,*,#11474,.F.);
#15614=ORIENTED_EDGE('',*,*,#11475,.T.);
#15615=ORIENTED_EDGE('',*,*,#11473,.T.);
#15616=ORIENTED_EDGE('',*,*,#11475,.F.);
#15617=ORIENTED_EDGE('',*,*,#11474,.T.);
#15618=ORIENTED_EDGE('',*,*,#11476,.F.);
#15619=ORIENTED_EDGE('',*,*,#11477,.F.);
#15620=ORIENTED_EDGE('',*,*,#11478,.T.);
#15621=ORIENTED_EDGE('',*,*,#11476,.T.);
#15622=ORIENTED_EDGE('',*,*,#11478,.F.);
#15623=ORIENTED_EDGE('',*,*,#11479,.F.);
#15624=ORIENTED_EDGE('',*,*,#11477,.T.);
#15625=ORIENTED_EDGE('',*,*,#11480,.F.);
#15626=ORIENTED_EDGE('',*,*,#11481,.T.);
#15627=ORIENTED_EDGE('',*,*,#11479,.T.);
#15628=ORIENTED_EDGE('',*,*,#11481,.F.);
#15629=ORIENTED_EDGE('',*,*,#11480,.T.);
#15630=ORIENTED_EDGE('',*,*,#11482,.F.);
#15631=ORIENTED_EDGE('',*,*,#11482,.T.);
#15632=ORIENTED_EDGE('',*,*,#11483,.T.);
#15633=ORIENTED_EDGE('',*,*,#11467,.F.);
#15634=ORIENTED_EDGE('',*,*,#11483,.F.);
#15635=ORIENTED_EDGE('',*,*,#11461,.T.);
#15636=ORIENTED_EDGE('',*,*,#11464,.T.);
#15637=ORIENTED_EDGE('',*,*,#11454,.T.);
#15638=ORIENTED_EDGE('',*,*,#11458,.T.);
#15639=ORIENTED_EDGE('',*,*,#11484,.F.);
#15640=ORIENTED_EDGE('',*,*,#11485,.F.);
#15641=ORIENTED_EDGE('',*,*,#11486,.F.);
#15642=ORIENTED_EDGE('',*,*,#11487,.F.);
#15643=ORIENTED_EDGE('',*,*,#11488,.F.);
#15644=ORIENTED_EDGE('',*,*,#11487,.T.);
#15645=ORIENTED_EDGE('',*,*,#11489,.F.);
#15646=ORIENTED_EDGE('',*,*,#11490,.T.);
#15647=ORIENTED_EDGE('',*,*,#11491,.F.);
#15648=ORIENTED_EDGE('',*,*,#11490,.F.);
#15649=ORIENTED_EDGE('',*,*,#11492,.F.);
#15650=ORIENTED_EDGE('',*,*,#11493,.F.);
#15651=ORIENTED_EDGE('',*,*,#11494,.F.);
#15652=ORIENTED_EDGE('',*,*,#11493,.T.);
#15653=ORIENTED_EDGE('',*,*,#11495,.F.);
#15654=ORIENTED_EDGE('',*,*,#11485,.T.);
#15655=ORIENTED_EDGE('',*,*,#11496,.F.);
#15656=ORIENTED_EDGE('',*,*,#11497,.T.);
#15657=ORIENTED_EDGE('',*,*,#11498,.F.);
#15658=ORIENTED_EDGE('',*,*,#11499,.T.);
#15659=ORIENTED_EDGE('',*,*,#11496,.T.);
#15660=ORIENTED_EDGE('',*,*,#11499,.F.);
#15661=ORIENTED_EDGE('',*,*,#11491,.T.);
#15662=ORIENTED_EDGE('',*,*,#11494,.T.);
#15663=ORIENTED_EDGE('',*,*,#11484,.T.);
#15664=ORIENTED_EDGE('',*,*,#11488,.T.);
#15665=ORIENTED_EDGE('',*,*,#11498,.T.);
#15666=ORIENTED_EDGE('',*,*,#11500,.F.);
#15667=ORIENTED_EDGE('',*,*,#11500,.T.);
#15668=ORIENTED_EDGE('',*,*,#11501,.T.);
#15669=ORIENTED_EDGE('',*,*,#11497,.F.);
#15670=ORIENTED_EDGE('',*,*,#11501,.F.);
#15671=ORIENTED_EDGE('',*,*,#11492,.T.);
#15672=ORIENTED_EDGE('',*,*,#11489,.T.);
#15673=ORIENTED_EDGE('',*,*,#11486,.T.);
#15674=ORIENTED_EDGE('',*,*,#11495,.T.);
#15675=ORIENTED_EDGE('',*,*,#11502,.T.);
#15676=ORIENTED_EDGE('',*,*,#11503,.T.);
#15677=ORIENTED_EDGE('',*,*,#11504,.T.);
#15678=ORIENTED_EDGE('',*,*,#11505,.T.);
#15679=ORIENTED_EDGE('',*,*,#11506,.T.);
#15680=ORIENTED_EDGE('',*,*,#11507,.T.);
#15681=ORIENTED_EDGE('',*,*,#11502,.F.);
#15682=ORIENTED_EDGE('',*,*,#11508,.T.);
#15683=ORIENTED_EDGE('',*,*,#11509,.T.);
#15684=ORIENTED_EDGE('',*,*,#11510,.T.);
#15685=ORIENTED_EDGE('',*,*,#11506,.F.);
#15686=ORIENTED_EDGE('',*,*,#11511,.T.);
#15687=ORIENTED_EDGE('',*,*,#11512,.T.);
#15688=ORIENTED_EDGE('',*,*,#11513,.T.);
#15689=ORIENTED_EDGE('',*,*,#11509,.F.);
#15690=ORIENTED_EDGE('',*,*,#11514,.T.);
#15691=ORIENTED_EDGE('',*,*,#11515,.T.);
#15692=ORIENTED_EDGE('',*,*,#11516,.T.);
#15693=ORIENTED_EDGE('',*,*,#11512,.F.);
#15694=ORIENTED_EDGE('',*,*,#11517,.T.);
#15695=ORIENTED_EDGE('',*,*,#11518,.T.);
#15696=ORIENTED_EDGE('',*,*,#11519,.T.);
#15697=ORIENTED_EDGE('',*,*,#11515,.F.);
#15698=ORIENTED_EDGE('',*,*,#11520,.T.);
#15699=ORIENTED_EDGE('',*,*,#11521,.T.);
#15700=ORIENTED_EDGE('',*,*,#11522,.T.);
#15701=ORIENTED_EDGE('',*,*,#11518,.F.);
#15702=ORIENTED_EDGE('',*,*,#11523,.T.);
#15703=ORIENTED_EDGE('',*,*,#11524,.T.);
#15704=ORIENTED_EDGE('',*,*,#11525,.T.);
#15705=ORIENTED_EDGE('',*,*,#11521,.F.);
#15706=ORIENTED_EDGE('',*,*,#11526,.T.);
#15707=ORIENTED_EDGE('',*,*,#11527,.F.);
#15708=ORIENTED_EDGE('',*,*,#11528,.F.);
#15709=ORIENTED_EDGE('',*,*,#11529,.T.);
#15710=ORIENTED_EDGE('',*,*,#11530,.T.);
#15711=ORIENTED_EDGE('',*,*,#11531,.T.);
#15712=ORIENTED_EDGE('',*,*,#11532,.F.);
#15713=ORIENTED_EDGE('',*,*,#11533,.F.);
#15714=ORIENTED_EDGE('',*,*,#11534,.T.);
#15715=ORIENTED_EDGE('',*,*,#11535,.T.);
#15716=ORIENTED_EDGE('',*,*,#11530,.F.);
#15717=ORIENTED_EDGE('',*,*,#11536,.F.);
#15718=ORIENTED_EDGE('',*,*,#11537,.T.);
#15719=ORIENTED_EDGE('',*,*,#11538,.T.);
#15720=ORIENTED_EDGE('',*,*,#11534,.F.);
#15721=ORIENTED_EDGE('',*,*,#11539,.F.);
#15722=ORIENTED_EDGE('',*,*,#11540,.T.);
#15723=ORIENTED_EDGE('',*,*,#11541,.T.);
#15724=ORIENTED_EDGE('',*,*,#11537,.F.);
#15725=ORIENTED_EDGE('',*,*,#11542,.F.);
#15726=ORIENTED_EDGE('',*,*,#11543,.T.);
#15727=ORIENTED_EDGE('',*,*,#11544,.T.);
#15728=ORIENTED_EDGE('',*,*,#11540,.F.);
#15729=ORIENTED_EDGE('',*,*,#11545,.F.);
#15730=ORIENTED_EDGE('',*,*,#11546,.T.);
#15731=ORIENTED_EDGE('',*,*,#11547,.T.);
#15732=ORIENTED_EDGE('',*,*,#11543,.F.);
#15733=ORIENTED_EDGE('',*,*,#11548,.F.);
#15734=ORIENTED_EDGE('',*,*,#11549,.T.);
#15735=ORIENTED_EDGE('',*,*,#11550,.T.);
#15736=ORIENTED_EDGE('',*,*,#11546,.F.);
#15737=ORIENTED_EDGE('',*,*,#11551,.F.);
#15738=ORIENTED_EDGE('',*,*,#11552,.T.);
#15739=ORIENTED_EDGE('',*,*,#11553,.T.);
#15740=ORIENTED_EDGE('',*,*,#11549,.F.);
#15741=ORIENTED_EDGE('',*,*,#11554,.F.);
#15742=ORIENTED_EDGE('',*,*,#11555,.F.);
#15743=ORIENTED_EDGE('',*,*,#11556,.F.);
#15744=ORIENTED_EDGE('',*,*,#11557,.F.);
#15745=ORIENTED_EDGE('',*,*,#11558,.T.);
#15746=ORIENTED_EDGE('',*,*,#11555,.T.);
#15747=ORIENTED_EDGE('',*,*,#11559,.T.);
#15748=ORIENTED_EDGE('',*,*,#11552,.F.);
#15749=ORIENTED_EDGE('',*,*,#11560,.F.);
#15750=ORIENTED_EDGE('',*,*,#11561,.F.);
#15751=ORIENTED_EDGE('',*,*,#11531,.F.);
#15752=ORIENTED_EDGE('',*,*,#11535,.F.);
#15753=ORIENTED_EDGE('',*,*,#11538,.F.);
#15754=ORIENTED_EDGE('',*,*,#11541,.F.);
#15755=ORIENTED_EDGE('',*,*,#11544,.F.);
#15756=ORIENTED_EDGE('',*,*,#11547,.F.);
#15757=ORIENTED_EDGE('',*,*,#11550,.F.);
#15758=ORIENTED_EDGE('',*,*,#11553,.F.);
#15759=ORIENTED_EDGE('',*,*,#11559,.F.);
#15760=ORIENTED_EDGE('',*,*,#11558,.F.);
#15761=ORIENTED_EDGE('',*,*,#11562,.F.);
#15762=ORIENTED_EDGE('',*,*,#11503,.F.);
#15763=ORIENTED_EDGE('',*,*,#11507,.F.);
#15764=ORIENTED_EDGE('',*,*,#11510,.F.);
#15765=ORIENTED_EDGE('',*,*,#11513,.F.);
#15766=ORIENTED_EDGE('',*,*,#11516,.F.);
#15767=ORIENTED_EDGE('',*,*,#11519,.F.);
#15768=ORIENTED_EDGE('',*,*,#11522,.F.);
#15769=ORIENTED_EDGE('',*,*,#11525,.F.);
#15770=ORIENTED_EDGE('',*,*,#11563,.F.);
#15771=ORIENTED_EDGE('',*,*,#11529,.F.);
#15772=ORIENTED_EDGE('',*,*,#11564,.F.);
#15773=ORIENTED_EDGE('',*,*,#11565,.F.);
#15774=ORIENTED_EDGE('',*,*,#11526,.F.);
#15775=ORIENTED_EDGE('',*,*,#11523,.F.);
#15776=ORIENTED_EDGE('',*,*,#11520,.F.);
#15777=ORIENTED_EDGE('',*,*,#11517,.F.);
#15778=ORIENTED_EDGE('',*,*,#11514,.F.);
#15779=ORIENTED_EDGE('',*,*,#11511,.F.);
#15780=ORIENTED_EDGE('',*,*,#11508,.F.);
#15781=ORIENTED_EDGE('',*,*,#11505,.F.);
#15782=ORIENTED_EDGE('',*,*,#11566,.F.);
#15783=ORIENTED_EDGE('',*,*,#11556,.T.);
#15784=ORIENTED_EDGE('',*,*,#11560,.T.);
#15785=ORIENTED_EDGE('',*,*,#11554,.T.);
#15786=ORIENTED_EDGE('',*,*,#11551,.T.);
#15787=ORIENTED_EDGE('',*,*,#11548,.T.);
#15788=ORIENTED_EDGE('',*,*,#11545,.T.);
#15789=ORIENTED_EDGE('',*,*,#11542,.T.);
#15790=ORIENTED_EDGE('',*,*,#11539,.T.);
#15791=ORIENTED_EDGE('',*,*,#11536,.T.);
#15792=ORIENTED_EDGE('',*,*,#11533,.T.);
#15793=ORIENTED_EDGE('',*,*,#11567,.T.);
#15794=ORIENTED_EDGE('',*,*,#11568,.T.);
#15795=ORIENTED_EDGE('',*,*,#11564,.T.);
#15796=ORIENTED_EDGE('',*,*,#11532,.T.);
#15797=ORIENTED_EDGE('',*,*,#11561,.T.);
#15798=ORIENTED_EDGE('',*,*,#11528,.T.);
#15799=ORIENTED_EDGE('',*,*,#11569,.T.);
#15800=ORIENTED_EDGE('',*,*,#11570,.T.);
#15801=ORIENTED_EDGE('',*,*,#11571,.T.);
#15802=ORIENTED_EDGE('',*,*,#11572,.T.);
#15803=ORIENTED_EDGE('',*,*,#11573,.F.);
#15804=ORIENTED_EDGE('',*,*,#11574,.T.);
#15805=ORIENTED_EDGE('',*,*,#11572,.F.);
#15806=ORIENTED_EDGE('',*,*,#11574,.F.);
#15807=ORIENTED_EDGE('',*,*,#11575,.F.);
#15808=ORIENTED_EDGE('',*,*,#11576,.T.);
#15809=ORIENTED_EDGE('',*,*,#11571,.F.);
#15810=ORIENTED_EDGE('',*,*,#11576,.F.);
#15811=ORIENTED_EDGE('',*,*,#11577,.F.);
#15812=ORIENTED_EDGE('',*,*,#11578,.T.);
#15813=ORIENTED_EDGE('',*,*,#11570,.F.);
#15814=ORIENTED_EDGE('',*,*,#11578,.F.);
#15815=ORIENTED_EDGE('',*,*,#11579,.F.);
#15816=ORIENTED_EDGE('',*,*,#11580,.F.);
#15817=ORIENTED_EDGE('',*,*,#11567,.F.);
#15818=ORIENTED_EDGE('',*,*,#11581,.F.);
#15819=ORIENTED_EDGE('',*,*,#11579,.T.);
#15820=ORIENTED_EDGE('',*,*,#11582,.F.);
#15821=ORIENTED_EDGE('',*,*,#11573,.T.);
#15822=ORIENTED_EDGE('',*,*,#11575,.T.);
#15823=ORIENTED_EDGE('',*,*,#11577,.T.);
#15824=ORIENTED_EDGE('',*,*,#11583,.T.);
#15825=ORIENTED_EDGE('',*,*,#11581,.T.);
#15826=ORIENTED_EDGE('',*,*,#11568,.F.);
#15827=ORIENTED_EDGE('',*,*,#11580,.T.);
#15828=ORIENTED_EDGE('',*,*,#11582,.T.);
#15829=ORIENTED_EDGE('',*,*,#11527,.T.);
#15830=ORIENTED_EDGE('',*,*,#11563,.T.);
#15831=ORIENTED_EDGE('',*,*,#11524,.F.);
#15832=ORIENTED_EDGE('',*,*,#11565,.T.);
#15833=ORIENTED_EDGE('',*,*,#11569,.F.);
#15834=ORIENTED_EDGE('',*,*,#11583,.F.);
#15835=ORIENTED_EDGE('',*,*,#11584,.T.);
#15836=ORIENTED_EDGE('',*,*,#11585,.T.);
#15837=ORIENTED_EDGE('',*,*,#11584,.F.);
#15838=ORIENTED_EDGE('',*,*,#11585,.F.);
#15839=ORIENTED_EDGE('',*,*,#11566,.T.);
#15840=ORIENTED_EDGE('',*,*,#11504,.F.);
#15841=ORIENTED_EDGE('',*,*,#11562,.T.);
#15842=ORIENTED_EDGE('',*,*,#11557,.T.);
#15843=ORIENTED_EDGE('',*,*,#11586,.T.);
#15844=ORIENTED_EDGE('',*,*,#11587,.T.);
#15845=ORIENTED_EDGE('',*,*,#11588,.T.);
#15846=ORIENTED_EDGE('',*,*,#11589,.F.);
#15847=ORIENTED_EDGE('',*,*,#11590,.T.);
#15848=ORIENTED_EDGE('',*,*,#11591,.T.);
#15849=ORIENTED_EDGE('',*,*,#11592,.T.);
#15850=ORIENTED_EDGE('',*,*,#11587,.F.);
#15851=ORIENTED_EDGE('',*,*,#11593,.T.);
#15852=ORIENTED_EDGE('',*,*,#11594,.T.);
#15853=ORIENTED_EDGE('',*,*,#11595,.T.);
#15854=ORIENTED_EDGE('',*,*,#11591,.F.);
#15855=ORIENTED_EDGE('',*,*,#11596,.T.);
#15856=ORIENTED_EDGE('',*,*,#11597,.T.);
#15857=ORIENTED_EDGE('',*,*,#11598,.T.);
#15858=ORIENTED_EDGE('',*,*,#11594,.F.);
#15859=ORIENTED_EDGE('',*,*,#11599,.T.);
#15860=ORIENTED_EDGE('',*,*,#11600,.T.);
#15861=ORIENTED_EDGE('',*,*,#11601,.T.);
#15862=ORIENTED_EDGE('',*,*,#11597,.F.);
#15863=ORIENTED_EDGE('',*,*,#11602,.T.);
#15864=ORIENTED_EDGE('',*,*,#11589,.T.);
#15865=ORIENTED_EDGE('',*,*,#11603,.T.);
#15866=ORIENTED_EDGE('',*,*,#11600,.F.);
#15867=ORIENTED_EDGE('',*,*,#11602,.F.);
#15868=ORIENTED_EDGE('',*,*,#11599,.F.);
#15869=ORIENTED_EDGE('',*,*,#11596,.F.);
#15870=ORIENTED_EDGE('',*,*,#11593,.F.);
#15871=ORIENTED_EDGE('',*,*,#11590,.F.);
#15872=ORIENTED_EDGE('',*,*,#11586,.F.);
#15873=ORIENTED_EDGE('',*,*,#11603,.F.);
#15874=ORIENTED_EDGE('',*,*,#11588,.F.);
#15875=ORIENTED_EDGE('',*,*,#11592,.F.);
#15876=ORIENTED_EDGE('',*,*,#11595,.F.);
#15877=ORIENTED_EDGE('',*,*,#11598,.F.);
#15878=ORIENTED_EDGE('',*,*,#11601,.F.);
#15879=ORIENTED_EDGE('',*,*,#11604,.T.);
#15880=ORIENTED_EDGE('',*,*,#11605,.F.);
#15881=ORIENTED_EDGE('',*,*,#11604,.F.);
#15882=ORIENTED_EDGE('',*,*,#11606,.T.);
#15883=ORIENTED_EDGE('',*,*,#11607,.T.);
#15884=ORIENTED_EDGE('',*,*,#11606,.F.);
#15885=ORIENTED_EDGE('',*,*,#11607,.F.);
#15886=ORIENTED_EDGE('',*,*,#11608,.F.);
#15887=ORIENTED_EDGE('',*,*,#11609,.F.);
#15888=ORIENTED_EDGE('',*,*,#11610,.T.);
#15889=ORIENTED_EDGE('',*,*,#11608,.T.);
#15890=ORIENTED_EDGE('',*,*,#11610,.F.);
#15891=ORIENTED_EDGE('',*,*,#11611,.F.);
#15892=ORIENTED_EDGE('',*,*,#11612,.T.);
#15893=ORIENTED_EDGE('',*,*,#11609,.T.);
#15894=ORIENTED_EDGE('',*,*,#11612,.F.);
#15895=ORIENTED_EDGE('',*,*,#11613,.F.);
#15896=ORIENTED_EDGE('',*,*,#11614,.T.);
#15897=ORIENTED_EDGE('',*,*,#11611,.T.);
#15898=ORIENTED_EDGE('',*,*,#11614,.F.);
#15899=ORIENTED_EDGE('',*,*,#11613,.T.);
#15900=ORIENTED_EDGE('',*,*,#11615,.F.);
#15901=ORIENTED_EDGE('',*,*,#11616,.F.);
#15902=ORIENTED_EDGE('',*,*,#11617,.T.);
#15903=ORIENTED_EDGE('',*,*,#11615,.T.);
#15904=ORIENTED_EDGE('',*,*,#11617,.F.);
#15905=ORIENTED_EDGE('',*,*,#11605,.T.);
#15906=ORIENTED_EDGE('',*,*,#11618,.T.);
#15907=ORIENTED_EDGE('',*,*,#11616,.T.);
#15908=ORIENTED_EDGE('',*,*,#11618,.F.);
#15909=ORIENTED_EDGE('',*,*,#11619,.F.);
#15910=ORIENTED_EDGE('',*,*,#11620,.F.);
#15911=ORIENTED_EDGE('',*,*,#11621,.T.);
#15912=ORIENTED_EDGE('',*,*,#11619,.T.);
#15913=ORIENTED_EDGE('',*,*,#11621,.F.);
#15914=ORIENTED_EDGE('',*,*,#11622,.F.);
#15915=ORIENTED_EDGE('',*,*,#11623,.T.);
#15916=ORIENTED_EDGE('',*,*,#11620,.T.);
#15917=ORIENTED_EDGE('',*,*,#11623,.F.);
#15918=ORIENTED_EDGE('',*,*,#11624,.F.);
#15919=ORIENTED_EDGE('',*,*,#11625,.T.);
#15920=ORIENTED_EDGE('',*,*,#11622,.T.);
#15921=ORIENTED_EDGE('',*,*,#11625,.F.);
#15922=ORIENTED_EDGE('',*,*,#11624,.T.);
#15923=ORIENTED_EDGE('',*,*,#11626,.F.);
#15924=ORIENTED_EDGE('',*,*,#11627,.F.);
#15925=ORIENTED_EDGE('',*,*,#11628,.T.);
#15926=ORIENTED_EDGE('',*,*,#11626,.T.);
#15927=ORIENTED_EDGE('',*,*,#11628,.F.);
#15928=ORIENTED_EDGE('',*,*,#11629,.F.);
#15929=ORIENTED_EDGE('',*,*,#11630,.T.);
#15930=ORIENTED_EDGE('',*,*,#11627,.T.);
#15931=ORIENTED_EDGE('',*,*,#11630,.F.);
#15932=ORIENTED_EDGE('',*,*,#11631,.F.);
#15933=ORIENTED_EDGE('',*,*,#11632,.T.);
#15934=ORIENTED_EDGE('',*,*,#11629,.T.);
#15935=ORIENTED_EDGE('',*,*,#11632,.F.);
#15936=ORIENTED_EDGE('',*,*,#11631,.T.);
#15937=ORIENTED_EDGE('',*,*,#11633,.T.);
#15938=ORIENTED_EDGE('',*,*,#11634,.T.);
#15939=ORIENTED_EDGE('',*,*,#11635,.T.);
#15940=ORIENTED_EDGE('',*,*,#11636,.F.);
#15941=ORIENTED_EDGE('',*,*,#11637,.T.);
#15942=ORIENTED_EDGE('',*,*,#11638,.T.);
#15943=ORIENTED_EDGE('',*,*,#11639,.T.);
#15944=ORIENTED_EDGE('',*,*,#11634,.F.);
#15945=ORIENTED_EDGE('',*,*,#11640,.T.);
#15946=ORIENTED_EDGE('',*,*,#11641,.T.);
#15947=ORIENTED_EDGE('',*,*,#11642,.T.);
#15948=ORIENTED_EDGE('',*,*,#11638,.F.);
#15949=ORIENTED_EDGE('',*,*,#11643,.T.);
#15950=ORIENTED_EDGE('',*,*,#11644,.T.);
#15951=ORIENTED_EDGE('',*,*,#11645,.T.);
#15952=ORIENTED_EDGE('',*,*,#11641,.F.);
#15953=ORIENTED_EDGE('',*,*,#11646,.T.);
#15954=ORIENTED_EDGE('',*,*,#11647,.T.);
#15955=ORIENTED_EDGE('',*,*,#11648,.T.);
#15956=ORIENTED_EDGE('',*,*,#11644,.F.);
#15957=ORIENTED_EDGE('',*,*,#11649,.T.);
#15958=ORIENTED_EDGE('',*,*,#11636,.T.);
#15959=ORIENTED_EDGE('',*,*,#11650,.T.);
#15960=ORIENTED_EDGE('',*,*,#11647,.F.);
#15961=ORIENTED_EDGE('',*,*,#11649,.F.);
#15962=ORIENTED_EDGE('',*,*,#11646,.F.);
#15963=ORIENTED_EDGE('',*,*,#11643,.F.);
#15964=ORIENTED_EDGE('',*,*,#11640,.F.);
#15965=ORIENTED_EDGE('',*,*,#11637,.F.);
#15966=ORIENTED_EDGE('',*,*,#11633,.F.);
#15967=ORIENTED_EDGE('',*,*,#11650,.F.);
#15968=ORIENTED_EDGE('',*,*,#11635,.F.);
#15969=ORIENTED_EDGE('',*,*,#11639,.F.);
#15970=ORIENTED_EDGE('',*,*,#11642,.F.);
#15971=ORIENTED_EDGE('',*,*,#11645,.F.);
#15972=ORIENTED_EDGE('',*,*,#11648,.F.);
#15973=ORIENTED_EDGE('',*,*,#11651,.F.);
#15974=ORIENTED_EDGE('',*,*,#11652,.T.);
#15975=ORIENTED_EDGE('',*,*,#11653,.T.);
#15976=ORIENTED_EDGE('',*,*,#11654,.T.);
#15977=ORIENTED_EDGE('',*,*,#11655,.F.);
#15978=ORIENTED_EDGE('',*,*,#11656,.T.);
#15979=ORIENTED_EDGE('',*,*,#11651,.T.);
#15980=ORIENTED_EDGE('',*,*,#11657,.T.);
#15981=ORIENTED_EDGE('',*,*,#11658,.F.);
#15982=ORIENTED_EDGE('',*,*,#11659,.T.);
#15983=ORIENTED_EDGE('',*,*,#11655,.T.);
#15984=ORIENTED_EDGE('',*,*,#11660,.T.);
#15985=ORIENTED_EDGE('',*,*,#11661,.F.);
#15986=ORIENTED_EDGE('',*,*,#11662,.T.);
#15987=ORIENTED_EDGE('',*,*,#11658,.T.);
#15988=ORIENTED_EDGE('',*,*,#11663,.T.);
#15989=ORIENTED_EDGE('',*,*,#11664,.F.);
#15990=ORIENTED_EDGE('',*,*,#11665,.T.);
#15991=ORIENTED_EDGE('',*,*,#11661,.T.);
#15992=ORIENTED_EDGE('',*,*,#11666,.T.);
#15993=ORIENTED_EDGE('',*,*,#11667,.F.);
#15994=ORIENTED_EDGE('',*,*,#11668,.T.);
#15995=ORIENTED_EDGE('',*,*,#11664,.T.);
#15996=ORIENTED_EDGE('',*,*,#11669,.T.);
#15997=ORIENTED_EDGE('',*,*,#11670,.F.);
#15998=ORIENTED_EDGE('',*,*,#11671,.T.);
#15999=ORIENTED_EDGE('',*,*,#11667,.T.);
#16000=ORIENTED_EDGE('',*,*,#11672,.T.);
#16001=ORIENTED_EDGE('',*,*,#11673,.F.);
#16002=ORIENTED_EDGE('',*,*,#11674,.T.);
#16003=ORIENTED_EDGE('',*,*,#11670,.T.);
#16004=ORIENTED_EDGE('',*,*,#11675,.T.);
#16005=ORIENTED_EDGE('',*,*,#11676,.F.);
#16006=ORIENTED_EDGE('',*,*,#11677,.T.);
#16007=ORIENTED_EDGE('',*,*,#11673,.T.);
#16008=ORIENTED_EDGE('',*,*,#11678,.T.);
#16009=ORIENTED_EDGE('',*,*,#11679,.F.);
#16010=ORIENTED_EDGE('',*,*,#11680,.T.);
#16011=ORIENTED_EDGE('',*,*,#11676,.T.);
#16012=ORIENTED_EDGE('',*,*,#11681,.T.);
#16013=ORIENTED_EDGE('',*,*,#11682,.F.);
#16014=ORIENTED_EDGE('',*,*,#11683,.T.);
#16015=ORIENTED_EDGE('',*,*,#11679,.T.);
#16016=ORIENTED_EDGE('',*,*,#11684,.T.);
#16017=ORIENTED_EDGE('',*,*,#11685,.F.);
#16018=ORIENTED_EDGE('',*,*,#11686,.T.);
#16019=ORIENTED_EDGE('',*,*,#11682,.T.);
#16020=ORIENTED_EDGE('',*,*,#11687,.T.);
#16021=ORIENTED_EDGE('',*,*,#11688,.F.);
#16022=ORIENTED_EDGE('',*,*,#11689,.T.);
#16023=ORIENTED_EDGE('',*,*,#11685,.T.);
#16024=ORIENTED_EDGE('',*,*,#11690,.T.);
#16025=ORIENTED_EDGE('',*,*,#11691,.F.);
#16026=ORIENTED_EDGE('',*,*,#11692,.T.);
#16027=ORIENTED_EDGE('',*,*,#11688,.T.);
#16028=ORIENTED_EDGE('',*,*,#11693,.T.);
#16029=ORIENTED_EDGE('',*,*,#11694,.F.);
#16030=ORIENTED_EDGE('',*,*,#11695,.T.);
#16031=ORIENTED_EDGE('',*,*,#11691,.T.);
#16032=ORIENTED_EDGE('',*,*,#11696,.T.);
#16033=ORIENTED_EDGE('',*,*,#11697,.F.);
#16034=ORIENTED_EDGE('',*,*,#11698,.T.);
#16035=ORIENTED_EDGE('',*,*,#11694,.T.);
#16036=ORIENTED_EDGE('',*,*,#11699,.T.);
#16037=ORIENTED_EDGE('',*,*,#11700,.F.);
#16038=ORIENTED_EDGE('',*,*,#11701,.T.);
#16039=ORIENTED_EDGE('',*,*,#11697,.T.);
#16040=ORIENTED_EDGE('',*,*,#11702,.T.);
#16041=ORIENTED_EDGE('',*,*,#11703,.F.);
#16042=ORIENTED_EDGE('',*,*,#11704,.T.);
#16043=ORIENTED_EDGE('',*,*,#11700,.T.);
#16044=ORIENTED_EDGE('',*,*,#11705,.T.);
#16045=ORIENTED_EDGE('',*,*,#11706,.F.);
#16046=ORIENTED_EDGE('',*,*,#11707,.T.);
#16047=ORIENTED_EDGE('',*,*,#11703,.T.);
#16048=ORIENTED_EDGE('',*,*,#11708,.T.);
#16049=ORIENTED_EDGE('',*,*,#11709,.F.);
#16050=ORIENTED_EDGE('',*,*,#11710,.T.);
#16051=ORIENTED_EDGE('',*,*,#11706,.T.);
#16052=ORIENTED_EDGE('',*,*,#11711,.T.);
#16053=ORIENTED_EDGE('',*,*,#11712,.F.);
#16054=ORIENTED_EDGE('',*,*,#11713,.T.);
#16055=ORIENTED_EDGE('',*,*,#11709,.T.);
#16056=ORIENTED_EDGE('',*,*,#11714,.T.);
#16057=ORIENTED_EDGE('',*,*,#11715,.F.);
#16058=ORIENTED_EDGE('',*,*,#11716,.T.);
#16059=ORIENTED_EDGE('',*,*,#11712,.T.);
#16060=ORIENTED_EDGE('',*,*,#11717,.T.);
#16061=ORIENTED_EDGE('',*,*,#11718,.F.);
#16062=ORIENTED_EDGE('',*,*,#11719,.T.);
#16063=ORIENTED_EDGE('',*,*,#11715,.T.);
#16064=ORIENTED_EDGE('',*,*,#11720,.T.);
#16065=ORIENTED_EDGE('',*,*,#11721,.F.);
#16066=ORIENTED_EDGE('',*,*,#11722,.T.);
#16067=ORIENTED_EDGE('',*,*,#11718,.T.);
#16068=ORIENTED_EDGE('',*,*,#11723,.T.);
#16069=ORIENTED_EDGE('',*,*,#11724,.F.);
#16070=ORIENTED_EDGE('',*,*,#11725,.T.);
#16071=ORIENTED_EDGE('',*,*,#11721,.T.);
#16072=ORIENTED_EDGE('',*,*,#11726,.T.);
#16073=ORIENTED_EDGE('',*,*,#11727,.F.);
#16074=ORIENTED_EDGE('',*,*,#11728,.T.);
#16075=ORIENTED_EDGE('',*,*,#11724,.T.);
#16076=ORIENTED_EDGE('',*,*,#11729,.T.);
#16077=ORIENTED_EDGE('',*,*,#11730,.F.);
#16078=ORIENTED_EDGE('',*,*,#11731,.T.);
#16079=ORIENTED_EDGE('',*,*,#11727,.T.);
#16080=ORIENTED_EDGE('',*,*,#11732,.T.);
#16081=ORIENTED_EDGE('',*,*,#11733,.F.);
#16082=ORIENTED_EDGE('',*,*,#11734,.T.);
#16083=ORIENTED_EDGE('',*,*,#11730,.T.);
#16084=ORIENTED_EDGE('',*,*,#11735,.T.);
#16085=ORIENTED_EDGE('',*,*,#11736,.F.);
#16086=ORIENTED_EDGE('',*,*,#11737,.T.);
#16087=ORIENTED_EDGE('',*,*,#11733,.T.);
#16088=ORIENTED_EDGE('',*,*,#11738,.T.);
#16089=ORIENTED_EDGE('',*,*,#11739,.F.);
#16090=ORIENTED_EDGE('',*,*,#11740,.T.);
#16091=ORIENTED_EDGE('',*,*,#11736,.T.);
#16092=ORIENTED_EDGE('',*,*,#11741,.T.);
#16093=ORIENTED_EDGE('',*,*,#11742,.F.);
#16094=ORIENTED_EDGE('',*,*,#11743,.T.);
#16095=ORIENTED_EDGE('',*,*,#11739,.T.);
#16096=ORIENTED_EDGE('',*,*,#11744,.T.);
#16097=ORIENTED_EDGE('',*,*,#11745,.F.);
#16098=ORIENTED_EDGE('',*,*,#11746,.T.);
#16099=ORIENTED_EDGE('',*,*,#11742,.T.);
#16100=ORIENTED_EDGE('',*,*,#11747,.T.);
#16101=ORIENTED_EDGE('',*,*,#11748,.F.);
#16102=ORIENTED_EDGE('',*,*,#11749,.T.);
#16103=ORIENTED_EDGE('',*,*,#11745,.T.);
#16104=ORIENTED_EDGE('',*,*,#11750,.T.);
#16105=ORIENTED_EDGE('',*,*,#11751,.F.);
#16106=ORIENTED_EDGE('',*,*,#11752,.T.);
#16107=ORIENTED_EDGE('',*,*,#11748,.T.);
#16108=ORIENTED_EDGE('',*,*,#11753,.T.);
#16109=ORIENTED_EDGE('',*,*,#11754,.F.);
#16110=ORIENTED_EDGE('',*,*,#11755,.T.);
#16111=ORIENTED_EDGE('',*,*,#11751,.T.);
#16112=ORIENTED_EDGE('',*,*,#11756,.T.);
#16113=ORIENTED_EDGE('',*,*,#11757,.F.);
#16114=ORIENTED_EDGE('',*,*,#11758,.T.);
#16115=ORIENTED_EDGE('',*,*,#11754,.T.);
#16116=ORIENTED_EDGE('',*,*,#11759,.T.);
#16117=ORIENTED_EDGE('',*,*,#11760,.F.);
#16118=ORIENTED_EDGE('',*,*,#11761,.T.);
#16119=ORIENTED_EDGE('',*,*,#11757,.T.);
#16120=ORIENTED_EDGE('',*,*,#11762,.T.);
#16121=ORIENTED_EDGE('',*,*,#11763,.F.);
#16122=ORIENTED_EDGE('',*,*,#11764,.T.);
#16123=ORIENTED_EDGE('',*,*,#11760,.T.);
#16124=ORIENTED_EDGE('',*,*,#11765,.T.);
#16125=ORIENTED_EDGE('',*,*,#11766,.F.);
#16126=ORIENTED_EDGE('',*,*,#11767,.T.);
#16127=ORIENTED_EDGE('',*,*,#11763,.T.);
#16128=ORIENTED_EDGE('',*,*,#11768,.T.);
#16129=ORIENTED_EDGE('',*,*,#11769,.F.);
#16130=ORIENTED_EDGE('',*,*,#11770,.T.);
#16131=ORIENTED_EDGE('',*,*,#11766,.T.);
#16132=ORIENTED_EDGE('',*,*,#11771,.T.);
#16133=ORIENTED_EDGE('',*,*,#11772,.F.);
#16134=ORIENTED_EDGE('',*,*,#11773,.T.);
#16135=ORIENTED_EDGE('',*,*,#11769,.T.);
#16136=ORIENTED_EDGE('',*,*,#11774,.T.);
#16137=ORIENTED_EDGE('',*,*,#11775,.F.);
#16138=ORIENTED_EDGE('',*,*,#11776,.T.);
#16139=ORIENTED_EDGE('',*,*,#11772,.T.);
#16140=ORIENTED_EDGE('',*,*,#11777,.T.);
#16141=ORIENTED_EDGE('',*,*,#11778,.F.);
#16142=ORIENTED_EDGE('',*,*,#11779,.T.);
#16143=ORIENTED_EDGE('',*,*,#11775,.T.);
#16144=ORIENTED_EDGE('',*,*,#11780,.T.);
#16145=ORIENTED_EDGE('',*,*,#11781,.F.);
#16146=ORIENTED_EDGE('',*,*,#11782,.T.);
#16147=ORIENTED_EDGE('',*,*,#11778,.T.);
#16148=ORIENTED_EDGE('',*,*,#11783,.T.);
#16149=ORIENTED_EDGE('',*,*,#11784,.F.);
#16150=ORIENTED_EDGE('',*,*,#11785,.T.);
#16151=ORIENTED_EDGE('',*,*,#11781,.T.);
#16152=ORIENTED_EDGE('',*,*,#11786,.T.);
#16153=ORIENTED_EDGE('',*,*,#11787,.F.);
#16154=ORIENTED_EDGE('',*,*,#11788,.T.);
#16155=ORIENTED_EDGE('',*,*,#11784,.T.);
#16156=ORIENTED_EDGE('',*,*,#11789,.T.);
#16157=ORIENTED_EDGE('',*,*,#11790,.F.);
#16158=ORIENTED_EDGE('',*,*,#11791,.T.);
#16159=ORIENTED_EDGE('',*,*,#11787,.T.);
#16160=ORIENTED_EDGE('',*,*,#11792,.T.);
#16161=ORIENTED_EDGE('',*,*,#11793,.F.);
#16162=ORIENTED_EDGE('',*,*,#11794,.T.);
#16163=ORIENTED_EDGE('',*,*,#11790,.T.);
#16164=ORIENTED_EDGE('',*,*,#11795,.T.);
#16165=ORIENTED_EDGE('',*,*,#11796,.F.);
#16166=ORIENTED_EDGE('',*,*,#11797,.T.);
#16167=ORIENTED_EDGE('',*,*,#11793,.T.);
#16168=ORIENTED_EDGE('',*,*,#11798,.T.);
#16169=ORIENTED_EDGE('',*,*,#11799,.F.);
#16170=ORIENTED_EDGE('',*,*,#11800,.T.);
#16171=ORIENTED_EDGE('',*,*,#11796,.T.);
#16172=ORIENTED_EDGE('',*,*,#11801,.T.);
#16173=ORIENTED_EDGE('',*,*,#11802,.F.);
#16174=ORIENTED_EDGE('',*,*,#11803,.T.);
#16175=ORIENTED_EDGE('',*,*,#11799,.T.);
#16176=ORIENTED_EDGE('',*,*,#11804,.T.);
#16177=ORIENTED_EDGE('',*,*,#11805,.F.);
#16178=ORIENTED_EDGE('',*,*,#11806,.T.);
#16179=ORIENTED_EDGE('',*,*,#11802,.T.);
#16180=ORIENTED_EDGE('',*,*,#11807,.T.);
#16181=ORIENTED_EDGE('',*,*,#11808,.F.);
#16182=ORIENTED_EDGE('',*,*,#11809,.T.);
#16183=ORIENTED_EDGE('',*,*,#11805,.T.);
#16184=ORIENTED_EDGE('',*,*,#11810,.T.);
#16185=ORIENTED_EDGE('',*,*,#11811,.F.);
#16186=ORIENTED_EDGE('',*,*,#11812,.T.);
#16187=ORIENTED_EDGE('',*,*,#11808,.T.);
#16188=ORIENTED_EDGE('',*,*,#11813,.T.);
#16189=ORIENTED_EDGE('',*,*,#11814,.F.);
#16190=ORIENTED_EDGE('',*,*,#11815,.T.);
#16191=ORIENTED_EDGE('',*,*,#11811,.T.);
#16192=ORIENTED_EDGE('',*,*,#11816,.T.);
#16193=ORIENTED_EDGE('',*,*,#11817,.F.);
#16194=ORIENTED_EDGE('',*,*,#11818,.T.);
#16195=ORIENTED_EDGE('',*,*,#11814,.T.);
#16196=ORIENTED_EDGE('',*,*,#11819,.T.);
#16197=ORIENTED_EDGE('',*,*,#11820,.F.);
#16198=ORIENTED_EDGE('',*,*,#11821,.T.);
#16199=ORIENTED_EDGE('',*,*,#11817,.T.);
#16200=ORIENTED_EDGE('',*,*,#11822,.T.);
#16201=ORIENTED_EDGE('',*,*,#11823,.F.);
#16202=ORIENTED_EDGE('',*,*,#11824,.T.);
#16203=ORIENTED_EDGE('',*,*,#11820,.T.);
#16204=ORIENTED_EDGE('',*,*,#11825,.T.);
#16205=ORIENTED_EDGE('',*,*,#11826,.F.);
#16206=ORIENTED_EDGE('',*,*,#11827,.T.);
#16207=ORIENTED_EDGE('',*,*,#11823,.T.);
#16208=ORIENTED_EDGE('',*,*,#11828,.T.);
#16209=ORIENTED_EDGE('',*,*,#11829,.F.);
#16210=ORIENTED_EDGE('',*,*,#11830,.T.);
#16211=ORIENTED_EDGE('',*,*,#11826,.T.);
#16212=ORIENTED_EDGE('',*,*,#11831,.T.);
#16213=ORIENTED_EDGE('',*,*,#11832,.F.);
#16214=ORIENTED_EDGE('',*,*,#11833,.T.);
#16215=ORIENTED_EDGE('',*,*,#11829,.T.);
#16216=ORIENTED_EDGE('',*,*,#11834,.T.);
#16217=ORIENTED_EDGE('',*,*,#11835,.F.);
#16218=ORIENTED_EDGE('',*,*,#11836,.T.);
#16219=ORIENTED_EDGE('',*,*,#11832,.T.);
#16220=ORIENTED_EDGE('',*,*,#11837,.T.);
#16221=ORIENTED_EDGE('',*,*,#11838,.F.);
#16222=ORIENTED_EDGE('',*,*,#11839,.T.);
#16223=ORIENTED_EDGE('',*,*,#11835,.T.);
#16224=ORIENTED_EDGE('',*,*,#11840,.T.);
#16225=ORIENTED_EDGE('',*,*,#11841,.F.);
#16226=ORIENTED_EDGE('',*,*,#11842,.T.);
#16227=ORIENTED_EDGE('',*,*,#11843,.F.);
#16228=ORIENTED_EDGE('',*,*,#11844,.F.);
#16229=ORIENTED_EDGE('',*,*,#11845,.T.);
#16230=ORIENTED_EDGE('',*,*,#11841,.T.);
#16231=ORIENTED_EDGE('',*,*,#11846,.F.);
#16232=ORIENTED_EDGE('',*,*,#11847,.F.);
#16233=ORIENTED_EDGE('',*,*,#11848,.F.);
#16234=ORIENTED_EDGE('',*,*,#11849,.T.);
#16235=ORIENTED_EDGE('',*,*,#11844,.T.);
#16236=ORIENTED_EDGE('',*,*,#11850,.F.);
#16237=ORIENTED_EDGE('',*,*,#11851,.F.);
#16238=ORIENTED_EDGE('',*,*,#11852,.T.);
#16239=ORIENTED_EDGE('',*,*,#11848,.T.);
#16240=ORIENTED_EDGE('',*,*,#11853,.F.);
#16241=ORIENTED_EDGE('',*,*,#11854,.F.);
#16242=ORIENTED_EDGE('',*,*,#11855,.T.);
#16243=ORIENTED_EDGE('',*,*,#11851,.T.);
#16244=ORIENTED_EDGE('',*,*,#11856,.F.);
#16245=ORIENTED_EDGE('',*,*,#11857,.F.);
#16246=ORIENTED_EDGE('',*,*,#11858,.T.);
#16247=ORIENTED_EDGE('',*,*,#11854,.T.);
#16248=ORIENTED_EDGE('',*,*,#11859,.F.);
#16249=ORIENTED_EDGE('',*,*,#11860,.F.);
#16250=ORIENTED_EDGE('',*,*,#11861,.T.);
#16251=ORIENTED_EDGE('',*,*,#11857,.T.);
#16252=ORIENTED_EDGE('',*,*,#11862,.F.);
#16253=ORIENTED_EDGE('',*,*,#11863,.F.);
#16254=ORIENTED_EDGE('',*,*,#11864,.T.);
#16255=ORIENTED_EDGE('',*,*,#11860,.T.);
#16256=ORIENTED_EDGE('',*,*,#11865,.F.);
#16257=ORIENTED_EDGE('',*,*,#11866,.F.);
#16258=ORIENTED_EDGE('',*,*,#11867,.T.);
#16259=ORIENTED_EDGE('',*,*,#11863,.T.);
#16260=ORIENTED_EDGE('',*,*,#11868,.F.);
#16261=ORIENTED_EDGE('',*,*,#11869,.F.);
#16262=ORIENTED_EDGE('',*,*,#11870,.T.);
#16263=ORIENTED_EDGE('',*,*,#11866,.T.);
#16264=ORIENTED_EDGE('',*,*,#11871,.F.);
#16265=ORIENTED_EDGE('',*,*,#11872,.F.);
#16266=ORIENTED_EDGE('',*,*,#11873,.T.);
#16267=ORIENTED_EDGE('',*,*,#11869,.T.);
#16268=ORIENTED_EDGE('',*,*,#11874,.F.);
#16269=ORIENTED_EDGE('',*,*,#11875,.F.);
#16270=ORIENTED_EDGE('',*,*,#11876,.T.);
#16271=ORIENTED_EDGE('',*,*,#11872,.T.);
#16272=ORIENTED_EDGE('',*,*,#11877,.F.);
#16273=ORIENTED_EDGE('',*,*,#11878,.F.);
#16274=ORIENTED_EDGE('',*,*,#11879,.T.);
#16275=ORIENTED_EDGE('',*,*,#11875,.T.);
#16276=ORIENTED_EDGE('',*,*,#11880,.F.);
#16277=ORIENTED_EDGE('',*,*,#11881,.F.);
#16278=ORIENTED_EDGE('',*,*,#11882,.T.);
#16279=ORIENTED_EDGE('',*,*,#11878,.T.);
#16280=ORIENTED_EDGE('',*,*,#11883,.F.);
#16281=ORIENTED_EDGE('',*,*,#11884,.F.);
#16282=ORIENTED_EDGE('',*,*,#11885,.T.);
#16283=ORIENTED_EDGE('',*,*,#11881,.T.);
#16284=ORIENTED_EDGE('',*,*,#11886,.F.);
#16285=ORIENTED_EDGE('',*,*,#11887,.F.);
#16286=ORIENTED_EDGE('',*,*,#11888,.T.);
#16287=ORIENTED_EDGE('',*,*,#11884,.T.);
#16288=ORIENTED_EDGE('',*,*,#11889,.F.);
#16289=ORIENTED_EDGE('',*,*,#11890,.F.);
#16290=ORIENTED_EDGE('',*,*,#11891,.T.);
#16291=ORIENTED_EDGE('',*,*,#11887,.T.);
#16292=ORIENTED_EDGE('',*,*,#11892,.F.);
#16293=ORIENTED_EDGE('',*,*,#11893,.F.);
#16294=ORIENTED_EDGE('',*,*,#11894,.T.);
#16295=ORIENTED_EDGE('',*,*,#11890,.T.);
#16296=ORIENTED_EDGE('',*,*,#11895,.F.);
#16297=ORIENTED_EDGE('',*,*,#11896,.F.);
#16298=ORIENTED_EDGE('',*,*,#11897,.T.);
#16299=ORIENTED_EDGE('',*,*,#11893,.T.);
#16300=ORIENTED_EDGE('',*,*,#11898,.F.);
#16301=ORIENTED_EDGE('',*,*,#11899,.F.);
#16302=ORIENTED_EDGE('',*,*,#11900,.T.);
#16303=ORIENTED_EDGE('',*,*,#11896,.T.);
#16304=ORIENTED_EDGE('',*,*,#11901,.F.);
#16305=ORIENTED_EDGE('',*,*,#11902,.F.);
#16306=ORIENTED_EDGE('',*,*,#11903,.T.);
#16307=ORIENTED_EDGE('',*,*,#11899,.T.);
#16308=ORIENTED_EDGE('',*,*,#11904,.F.);
#16309=ORIENTED_EDGE('',*,*,#11905,.F.);
#16310=ORIENTED_EDGE('',*,*,#11906,.T.);
#16311=ORIENTED_EDGE('',*,*,#11902,.T.);
#16312=ORIENTED_EDGE('',*,*,#11907,.F.);
#16313=ORIENTED_EDGE('',*,*,#11908,.F.);
#16314=ORIENTED_EDGE('',*,*,#11909,.T.);
#16315=ORIENTED_EDGE('',*,*,#11905,.T.);
#16316=ORIENTED_EDGE('',*,*,#11910,.F.);
#16317=ORIENTED_EDGE('',*,*,#11911,.F.);
#16318=ORIENTED_EDGE('',*,*,#11912,.T.);
#16319=ORIENTED_EDGE('',*,*,#11908,.T.);
#16320=ORIENTED_EDGE('',*,*,#11913,.F.);
#16321=ORIENTED_EDGE('',*,*,#11914,.F.);
#16322=ORIENTED_EDGE('',*,*,#11915,.T.);
#16323=ORIENTED_EDGE('',*,*,#11911,.T.);
#16324=ORIENTED_EDGE('',*,*,#11916,.F.);
#16325=ORIENTED_EDGE('',*,*,#11917,.F.);
#16326=ORIENTED_EDGE('',*,*,#11918,.T.);
#16327=ORIENTED_EDGE('',*,*,#11914,.T.);
#16328=ORIENTED_EDGE('',*,*,#11919,.F.);
#16329=ORIENTED_EDGE('',*,*,#11920,.F.);
#16330=ORIENTED_EDGE('',*,*,#11921,.T.);
#16331=ORIENTED_EDGE('',*,*,#11917,.T.);
#16332=ORIENTED_EDGE('',*,*,#11922,.F.);
#16333=ORIENTED_EDGE('',*,*,#11923,.F.);
#16334=ORIENTED_EDGE('',*,*,#11924,.T.);
#16335=ORIENTED_EDGE('',*,*,#11920,.T.);
#16336=ORIENTED_EDGE('',*,*,#11925,.F.);
#16337=ORIENTED_EDGE('',*,*,#11926,.F.);
#16338=ORIENTED_EDGE('',*,*,#11927,.T.);
#16339=ORIENTED_EDGE('',*,*,#11923,.T.);
#16340=ORIENTED_EDGE('',*,*,#11928,.F.);
#16341=ORIENTED_EDGE('',*,*,#11929,.F.);
#16342=ORIENTED_EDGE('',*,*,#11930,.T.);
#16343=ORIENTED_EDGE('',*,*,#11926,.T.);
#16344=ORIENTED_EDGE('',*,*,#11931,.F.);
#16345=ORIENTED_EDGE('',*,*,#11932,.F.);
#16346=ORIENTED_EDGE('',*,*,#11933,.T.);
#16347=ORIENTED_EDGE('',*,*,#11929,.T.);
#16348=ORIENTED_EDGE('',*,*,#11934,.F.);
#16349=ORIENTED_EDGE('',*,*,#11935,.F.);
#16350=ORIENTED_EDGE('',*,*,#11936,.T.);
#16351=ORIENTED_EDGE('',*,*,#11932,.T.);
#16352=ORIENTED_EDGE('',*,*,#11937,.F.);
#16353=ORIENTED_EDGE('',*,*,#11938,.F.);
#16354=ORIENTED_EDGE('',*,*,#11939,.T.);
#16355=ORIENTED_EDGE('',*,*,#11935,.T.);
#16356=ORIENTED_EDGE('',*,*,#11940,.F.);
#16357=ORIENTED_EDGE('',*,*,#11941,.F.);
#16358=ORIENTED_EDGE('',*,*,#11942,.T.);
#16359=ORIENTED_EDGE('',*,*,#11938,.T.);
#16360=ORIENTED_EDGE('',*,*,#11943,.F.);
#16361=ORIENTED_EDGE('',*,*,#11944,.F.);
#16362=ORIENTED_EDGE('',*,*,#11945,.T.);
#16363=ORIENTED_EDGE('',*,*,#11941,.T.);
#16364=ORIENTED_EDGE('',*,*,#11946,.F.);
#16365=ORIENTED_EDGE('',*,*,#11947,.F.);
#16366=ORIENTED_EDGE('',*,*,#11948,.T.);
#16367=ORIENTED_EDGE('',*,*,#11944,.T.);
#16368=ORIENTED_EDGE('',*,*,#11949,.F.);
#16369=ORIENTED_EDGE('',*,*,#11950,.F.);
#16370=ORIENTED_EDGE('',*,*,#11951,.T.);
#16371=ORIENTED_EDGE('',*,*,#11947,.T.);
#16372=ORIENTED_EDGE('',*,*,#11952,.F.);
#16373=ORIENTED_EDGE('',*,*,#11953,.F.);
#16374=ORIENTED_EDGE('',*,*,#11954,.T.);
#16375=ORIENTED_EDGE('',*,*,#11950,.T.);
#16376=ORIENTED_EDGE('',*,*,#11955,.F.);
#16377=ORIENTED_EDGE('',*,*,#11956,.F.);
#16378=ORIENTED_EDGE('',*,*,#11957,.T.);
#16379=ORIENTED_EDGE('',*,*,#11953,.T.);
#16380=ORIENTED_EDGE('',*,*,#11958,.F.);
#16381=ORIENTED_EDGE('',*,*,#11959,.F.);
#16382=ORIENTED_EDGE('',*,*,#11960,.T.);
#16383=ORIENTED_EDGE('',*,*,#11956,.T.);
#16384=ORIENTED_EDGE('',*,*,#11961,.F.);
#16385=ORIENTED_EDGE('',*,*,#11962,.F.);
#16386=ORIENTED_EDGE('',*,*,#11963,.T.);
#16387=ORIENTED_EDGE('',*,*,#11959,.T.);
#16388=ORIENTED_EDGE('',*,*,#11964,.F.);
#16389=ORIENTED_EDGE('',*,*,#11965,.F.);
#16390=ORIENTED_EDGE('',*,*,#11966,.T.);
#16391=ORIENTED_EDGE('',*,*,#11962,.T.);
#16392=ORIENTED_EDGE('',*,*,#11967,.F.);
#16393=ORIENTED_EDGE('',*,*,#11968,.F.);
#16394=ORIENTED_EDGE('',*,*,#11969,.T.);
#16395=ORIENTED_EDGE('',*,*,#11965,.T.);
#16396=ORIENTED_EDGE('',*,*,#11970,.F.);
#16397=ORIENTED_EDGE('',*,*,#11971,.F.);
#16398=ORIENTED_EDGE('',*,*,#11972,.T.);
#16399=ORIENTED_EDGE('',*,*,#11968,.T.);
#16400=ORIENTED_EDGE('',*,*,#11973,.F.);
#16401=ORIENTED_EDGE('',*,*,#11974,.F.);
#16402=ORIENTED_EDGE('',*,*,#11975,.T.);
#16403=ORIENTED_EDGE('',*,*,#11971,.T.);
#16404=ORIENTED_EDGE('',*,*,#11976,.F.);
#16405=ORIENTED_EDGE('',*,*,#11977,.F.);
#16406=ORIENTED_EDGE('',*,*,#11978,.T.);
#16407=ORIENTED_EDGE('',*,*,#11974,.T.);
#16408=ORIENTED_EDGE('',*,*,#11979,.F.);
#16409=ORIENTED_EDGE('',*,*,#11980,.F.);
#16410=ORIENTED_EDGE('',*,*,#11981,.T.);
#16411=ORIENTED_EDGE('',*,*,#11977,.T.);
#16412=ORIENTED_EDGE('',*,*,#11982,.F.);
#16413=ORIENTED_EDGE('',*,*,#11983,.F.);
#16414=ORIENTED_EDGE('',*,*,#11984,.T.);
#16415=ORIENTED_EDGE('',*,*,#11980,.T.);
#16416=ORIENTED_EDGE('',*,*,#11985,.F.);
#16417=ORIENTED_EDGE('',*,*,#11986,.F.);
#16418=ORIENTED_EDGE('',*,*,#11987,.T.);
#16419=ORIENTED_EDGE('',*,*,#11983,.T.);
#16420=ORIENTED_EDGE('',*,*,#11988,.F.);
#16421=ORIENTED_EDGE('',*,*,#11989,.F.);
#16422=ORIENTED_EDGE('',*,*,#11990,.T.);
#16423=ORIENTED_EDGE('',*,*,#11986,.T.);
#16424=ORIENTED_EDGE('',*,*,#11991,.F.);
#16425=ORIENTED_EDGE('',*,*,#11992,.F.);
#16426=ORIENTED_EDGE('',*,*,#11993,.T.);
#16427=ORIENTED_EDGE('',*,*,#11989,.T.);
#16428=ORIENTED_EDGE('',*,*,#11994,.F.);
#16429=ORIENTED_EDGE('',*,*,#11995,.F.);
#16430=ORIENTED_EDGE('',*,*,#11996,.T.);
#16431=ORIENTED_EDGE('',*,*,#11992,.T.);
#16432=ORIENTED_EDGE('',*,*,#11997,.F.);
#16433=ORIENTED_EDGE('',*,*,#11998,.F.);
#16434=ORIENTED_EDGE('',*,*,#11999,.T.);
#16435=ORIENTED_EDGE('',*,*,#11995,.T.);
#16436=ORIENTED_EDGE('',*,*,#12000,.F.);
#16437=ORIENTED_EDGE('',*,*,#12001,.F.);
#16438=ORIENTED_EDGE('',*,*,#12002,.T.);
#16439=ORIENTED_EDGE('',*,*,#11998,.T.);
#16440=ORIENTED_EDGE('',*,*,#12003,.F.);
#16441=ORIENTED_EDGE('',*,*,#12004,.F.);
#16442=ORIENTED_EDGE('',*,*,#12005,.T.);
#16443=ORIENTED_EDGE('',*,*,#12001,.T.);
#16444=ORIENTED_EDGE('',*,*,#12006,.F.);
#16445=ORIENTED_EDGE('',*,*,#12007,.F.);
#16446=ORIENTED_EDGE('',*,*,#12008,.T.);
#16447=ORIENTED_EDGE('',*,*,#12004,.T.);
#16448=ORIENTED_EDGE('',*,*,#12009,.F.);
#16449=ORIENTED_EDGE('',*,*,#12010,.F.);
#16450=ORIENTED_EDGE('',*,*,#12011,.T.);
#16451=ORIENTED_EDGE('',*,*,#12007,.T.);
#16452=ORIENTED_EDGE('',*,*,#12012,.F.);
#16453=ORIENTED_EDGE('',*,*,#12013,.F.);
#16454=ORIENTED_EDGE('',*,*,#12014,.T.);
#16455=ORIENTED_EDGE('',*,*,#12010,.T.);
#16456=ORIENTED_EDGE('',*,*,#12015,.F.);
#16457=ORIENTED_EDGE('',*,*,#12016,.F.);
#16458=ORIENTED_EDGE('',*,*,#12017,.T.);
#16459=ORIENTED_EDGE('',*,*,#12013,.T.);
#16460=ORIENTED_EDGE('',*,*,#12018,.F.);
#16461=ORIENTED_EDGE('',*,*,#12019,.F.);
#16462=ORIENTED_EDGE('',*,*,#12020,.T.);
#16463=ORIENTED_EDGE('',*,*,#12016,.T.);
#16464=ORIENTED_EDGE('',*,*,#12021,.F.);
#16465=ORIENTED_EDGE('',*,*,#12022,.F.);
#16466=ORIENTED_EDGE('',*,*,#12023,.T.);
#16467=ORIENTED_EDGE('',*,*,#12019,.T.);
#16468=ORIENTED_EDGE('',*,*,#12024,.F.);
#16469=ORIENTED_EDGE('',*,*,#12025,.F.);
#16470=ORIENTED_EDGE('',*,*,#12026,.T.);
#16471=ORIENTED_EDGE('',*,*,#12022,.T.);
#16472=ORIENTED_EDGE('',*,*,#12027,.F.);
#16473=ORIENTED_EDGE('',*,*,#12028,.F.);
#16474=ORIENTED_EDGE('',*,*,#12029,.T.);
#16475=ORIENTED_EDGE('',*,*,#12025,.T.);
#16476=ORIENTED_EDGE('',*,*,#12030,.F.);
#16477=ORIENTED_EDGE('',*,*,#12031,.T.);
#16478=ORIENTED_EDGE('',*,*,#12032,.T.);
#16479=ORIENTED_EDGE('',*,*,#11653,.F.);
#16480=ORIENTED_EDGE('',*,*,#12033,.T.);
#16481=ORIENTED_EDGE('',*,*,#12034,.T.);
#16482=ORIENTED_EDGE('',*,*,#12031,.F.);
#16483=ORIENTED_EDGE('',*,*,#12035,.T.);
#16484=ORIENTED_EDGE('',*,*,#12036,.T.);
#16485=ORIENTED_EDGE('',*,*,#12035,.F.);
#16486=ORIENTED_EDGE('',*,*,#12036,.F.);
#16487=ORIENTED_EDGE('',*,*,#12037,.F.);
#16488=ORIENTED_EDGE('',*,*,#12038,.F.);
#16489=ORIENTED_EDGE('',*,*,#11840,.F.);
#16490=ORIENTED_EDGE('',*,*,#11837,.F.);
#16491=ORIENTED_EDGE('',*,*,#11834,.F.);
#16492=ORIENTED_EDGE('',*,*,#11831,.F.);
#16493=ORIENTED_EDGE('',*,*,#11828,.F.);
#16494=ORIENTED_EDGE('',*,*,#11825,.F.);
#16495=ORIENTED_EDGE('',*,*,#11822,.F.);
#16496=ORIENTED_EDGE('',*,*,#11819,.F.);
#16497=ORIENTED_EDGE('',*,*,#11816,.F.);
#16498=ORIENTED_EDGE('',*,*,#11813,.F.);
#16499=ORIENTED_EDGE('',*,*,#11810,.F.);
#16500=ORIENTED_EDGE('',*,*,#11807,.F.);
#16501=ORIENTED_EDGE('',*,*,#11804,.F.);
#16502=ORIENTED_EDGE('',*,*,#11801,.F.);
#16503=ORIENTED_EDGE('',*,*,#11798,.F.);
#16504=ORIENTED_EDGE('',*,*,#11795,.F.);
#16505=ORIENTED_EDGE('',*,*,#11792,.F.);
#16506=ORIENTED_EDGE('',*,*,#11789,.F.);
#16507=ORIENTED_EDGE('',*,*,#11786,.F.);
#16508=ORIENTED_EDGE('',*,*,#11783,.F.);
#16509=ORIENTED_EDGE('',*,*,#11780,.F.);
#16510=ORIENTED_EDGE('',*,*,#11777,.F.);
#16511=ORIENTED_EDGE('',*,*,#11774,.F.);
#16512=ORIENTED_EDGE('',*,*,#11771,.F.);
#16513=ORIENTED_EDGE('',*,*,#11768,.F.);
#16514=ORIENTED_EDGE('',*,*,#11765,.F.);
#16515=ORIENTED_EDGE('',*,*,#11762,.F.);
#16516=ORIENTED_EDGE('',*,*,#11759,.F.);
#16517=ORIENTED_EDGE('',*,*,#11756,.F.);
#16518=ORIENTED_EDGE('',*,*,#11753,.F.);
#16519=ORIENTED_EDGE('',*,*,#11750,.F.);
#16520=ORIENTED_EDGE('',*,*,#11747,.F.);
#16521=ORIENTED_EDGE('',*,*,#11744,.F.);
#16522=ORIENTED_EDGE('',*,*,#11741,.F.);
#16523=ORIENTED_EDGE('',*,*,#11738,.F.);
#16524=ORIENTED_EDGE('',*,*,#11735,.F.);
#16525=ORIENTED_EDGE('',*,*,#11732,.F.);
#16526=ORIENTED_EDGE('',*,*,#11729,.F.);
#16527=ORIENTED_EDGE('',*,*,#11726,.F.);
#16528=ORIENTED_EDGE('',*,*,#11723,.F.);
#16529=ORIENTED_EDGE('',*,*,#11720,.F.);
#16530=ORIENTED_EDGE('',*,*,#11717,.F.);
#16531=ORIENTED_EDGE('',*,*,#11714,.F.);
#16532=ORIENTED_EDGE('',*,*,#11711,.F.);
#16533=ORIENTED_EDGE('',*,*,#11708,.F.);
#16534=ORIENTED_EDGE('',*,*,#11705,.F.);
#16535=ORIENTED_EDGE('',*,*,#11702,.F.);
#16536=ORIENTED_EDGE('',*,*,#11699,.F.);
#16537=ORIENTED_EDGE('',*,*,#11696,.F.);
#16538=ORIENTED_EDGE('',*,*,#11693,.F.);
#16539=ORIENTED_EDGE('',*,*,#11690,.F.);
#16540=ORIENTED_EDGE('',*,*,#11687,.F.);
#16541=ORIENTED_EDGE('',*,*,#11684,.F.);
#16542=ORIENTED_EDGE('',*,*,#11681,.F.);
#16543=ORIENTED_EDGE('',*,*,#11678,.F.);
#16544=ORIENTED_EDGE('',*,*,#11675,.F.);
#16545=ORIENTED_EDGE('',*,*,#11672,.F.);
#16546=ORIENTED_EDGE('',*,*,#11669,.F.);
#16547=ORIENTED_EDGE('',*,*,#11666,.F.);
#16548=ORIENTED_EDGE('',*,*,#11663,.F.);
#16549=ORIENTED_EDGE('',*,*,#11660,.F.);
#16550=ORIENTED_EDGE('',*,*,#11657,.F.);
#16551=ORIENTED_EDGE('',*,*,#11654,.F.);
#16552=ORIENTED_EDGE('',*,*,#12032,.F.);
#16553=ORIENTED_EDGE('',*,*,#12039,.T.);
#16554=ORIENTED_EDGE('',*,*,#12030,.T.);
#16555=ORIENTED_EDGE('',*,*,#12027,.T.);
#16556=ORIENTED_EDGE('',*,*,#12024,.T.);
#16557=ORIENTED_EDGE('',*,*,#12021,.T.);
#16558=ORIENTED_EDGE('',*,*,#12018,.T.);
#16559=ORIENTED_EDGE('',*,*,#12015,.T.);
#16560=ORIENTED_EDGE('',*,*,#12012,.T.);
#16561=ORIENTED_EDGE('',*,*,#12009,.T.);
#16562=ORIENTED_EDGE('',*,*,#12006,.T.);
#16563=ORIENTED_EDGE('',*,*,#12003,.T.);
#16564=ORIENTED_EDGE('',*,*,#12000,.T.);
#16565=ORIENTED_EDGE('',*,*,#11997,.T.);
#16566=ORIENTED_EDGE('',*,*,#11994,.T.);
#16567=ORIENTED_EDGE('',*,*,#11991,.T.);
#16568=ORIENTED_EDGE('',*,*,#11988,.T.);
#16569=ORIENTED_EDGE('',*,*,#11985,.T.);
#16570=ORIENTED_EDGE('',*,*,#11982,.T.);
#16571=ORIENTED_EDGE('',*,*,#11979,.T.);
#16572=ORIENTED_EDGE('',*,*,#11976,.T.);
#16573=ORIENTED_EDGE('',*,*,#11973,.T.);
#16574=ORIENTED_EDGE('',*,*,#11970,.T.);
#16575=ORIENTED_EDGE('',*,*,#11967,.T.);
#16576=ORIENTED_EDGE('',*,*,#11964,.T.);
#16577=ORIENTED_EDGE('',*,*,#11961,.T.);
#16578=ORIENTED_EDGE('',*,*,#11958,.T.);
#16579=ORIENTED_EDGE('',*,*,#11955,.T.);
#16580=ORIENTED_EDGE('',*,*,#11952,.T.);
#16581=ORIENTED_EDGE('',*,*,#11949,.T.);
#16582=ORIENTED_EDGE('',*,*,#11946,.T.);
#16583=ORIENTED_EDGE('',*,*,#11943,.T.);
#16584=ORIENTED_EDGE('',*,*,#11940,.T.);
#16585=ORIENTED_EDGE('',*,*,#11937,.T.);
#16586=ORIENTED_EDGE('',*,*,#11934,.T.);
#16587=ORIENTED_EDGE('',*,*,#11931,.T.);
#16588=ORIENTED_EDGE('',*,*,#11928,.T.);
#16589=ORIENTED_EDGE('',*,*,#11925,.T.);
#16590=ORIENTED_EDGE('',*,*,#11922,.T.);
#16591=ORIENTED_EDGE('',*,*,#11919,.T.);
#16592=ORIENTED_EDGE('',*,*,#11916,.T.);
#16593=ORIENTED_EDGE('',*,*,#11913,.T.);
#16594=ORIENTED_EDGE('',*,*,#11910,.T.);
#16595=ORIENTED_EDGE('',*,*,#11907,.T.);
#16596=ORIENTED_EDGE('',*,*,#11904,.T.);
#16597=ORIENTED_EDGE('',*,*,#11901,.T.);
#16598=ORIENTED_EDGE('',*,*,#11898,.T.);
#16599=ORIENTED_EDGE('',*,*,#11895,.T.);
#16600=ORIENTED_EDGE('',*,*,#11892,.T.);
#16601=ORIENTED_EDGE('',*,*,#11889,.T.);
#16602=ORIENTED_EDGE('',*,*,#11886,.T.);
#16603=ORIENTED_EDGE('',*,*,#11883,.T.);
#16604=ORIENTED_EDGE('',*,*,#11880,.T.);
#16605=ORIENTED_EDGE('',*,*,#11877,.T.);
#16606=ORIENTED_EDGE('',*,*,#11874,.T.);
#16607=ORIENTED_EDGE('',*,*,#11871,.T.);
#16608=ORIENTED_EDGE('',*,*,#11868,.T.);
#16609=ORIENTED_EDGE('',*,*,#11865,.T.);
#16610=ORIENTED_EDGE('',*,*,#11862,.T.);
#16611=ORIENTED_EDGE('',*,*,#11859,.T.);
#16612=ORIENTED_EDGE('',*,*,#11856,.T.);
#16613=ORIENTED_EDGE('',*,*,#11853,.T.);
#16614=ORIENTED_EDGE('',*,*,#11850,.T.);
#16615=ORIENTED_EDGE('',*,*,#11847,.T.);
#16616=ORIENTED_EDGE('',*,*,#12028,.T.);
#16617=ORIENTED_EDGE('',*,*,#12039,.F.);
#16618=ORIENTED_EDGE('',*,*,#12034,.F.);
#16619=ORIENTED_EDGE('',*,*,#12040,.T.);
#16620=ORIENTED_EDGE('',*,*,#12041,.F.);
#16621=ORIENTED_EDGE('',*,*,#11842,.F.);
#16622=ORIENTED_EDGE('',*,*,#11845,.F.);
#16623=ORIENTED_EDGE('',*,*,#11849,.F.);
#16624=ORIENTED_EDGE('',*,*,#11852,.F.);
#16625=ORIENTED_EDGE('',*,*,#11855,.F.);
#16626=ORIENTED_EDGE('',*,*,#11858,.F.);
#16627=ORIENTED_EDGE('',*,*,#11861,.F.);
#16628=ORIENTED_EDGE('',*,*,#11864,.F.);
#16629=ORIENTED_EDGE('',*,*,#11867,.F.);
#16630=ORIENTED_EDGE('',*,*,#11870,.F.);
#16631=ORIENTED_EDGE('',*,*,#11873,.F.);
#16632=ORIENTED_EDGE('',*,*,#11876,.F.);
#16633=ORIENTED_EDGE('',*,*,#11879,.F.);
#16634=ORIENTED_EDGE('',*,*,#11882,.F.);
#16635=ORIENTED_EDGE('',*,*,#11885,.F.);
#16636=ORIENTED_EDGE('',*,*,#11888,.F.);
#16637=ORIENTED_EDGE('',*,*,#11891,.F.);
#16638=ORIENTED_EDGE('',*,*,#11894,.F.);
#16639=ORIENTED_EDGE('',*,*,#11897,.F.);
#16640=ORIENTED_EDGE('',*,*,#11900,.F.);
#16641=ORIENTED_EDGE('',*,*,#11903,.F.);
#16642=ORIENTED_EDGE('',*,*,#11906,.F.);
#16643=ORIENTED_EDGE('',*,*,#11909,.F.);
#16644=ORIENTED_EDGE('',*,*,#11912,.F.);
#16645=ORIENTED_EDGE('',*,*,#11915,.F.);
#16646=ORIENTED_EDGE('',*,*,#11918,.F.);
#16647=ORIENTED_EDGE('',*,*,#11921,.F.);
#16648=ORIENTED_EDGE('',*,*,#11924,.F.);
#16649=ORIENTED_EDGE('',*,*,#11927,.F.);
#16650=ORIENTED_EDGE('',*,*,#11930,.F.);
#16651=ORIENTED_EDGE('',*,*,#11933,.F.);
#16652=ORIENTED_EDGE('',*,*,#11936,.F.);
#16653=ORIENTED_EDGE('',*,*,#11939,.F.);
#16654=ORIENTED_EDGE('',*,*,#11942,.F.);
#16655=ORIENTED_EDGE('',*,*,#11945,.F.);
#16656=ORIENTED_EDGE('',*,*,#11948,.F.);
#16657=ORIENTED_EDGE('',*,*,#11951,.F.);
#16658=ORIENTED_EDGE('',*,*,#11954,.F.);
#16659=ORIENTED_EDGE('',*,*,#11957,.F.);
#16660=ORIENTED_EDGE('',*,*,#11960,.F.);
#16661=ORIENTED_EDGE('',*,*,#11963,.F.);
#16662=ORIENTED_EDGE('',*,*,#11966,.F.);
#16663=ORIENTED_EDGE('',*,*,#11969,.F.);
#16664=ORIENTED_EDGE('',*,*,#11972,.F.);
#16665=ORIENTED_EDGE('',*,*,#11975,.F.);
#16666=ORIENTED_EDGE('',*,*,#11978,.F.);
#16667=ORIENTED_EDGE('',*,*,#11981,.F.);
#16668=ORIENTED_EDGE('',*,*,#11984,.F.);
#16669=ORIENTED_EDGE('',*,*,#11987,.F.);
#16670=ORIENTED_EDGE('',*,*,#11990,.F.);
#16671=ORIENTED_EDGE('',*,*,#11993,.F.);
#16672=ORIENTED_EDGE('',*,*,#11996,.F.);
#16673=ORIENTED_EDGE('',*,*,#11999,.F.);
#16674=ORIENTED_EDGE('',*,*,#12002,.F.);
#16675=ORIENTED_EDGE('',*,*,#12005,.F.);
#16676=ORIENTED_EDGE('',*,*,#12008,.F.);
#16677=ORIENTED_EDGE('',*,*,#12011,.F.);
#16678=ORIENTED_EDGE('',*,*,#12014,.F.);
#16679=ORIENTED_EDGE('',*,*,#12017,.F.);
#16680=ORIENTED_EDGE('',*,*,#12020,.F.);
#16681=ORIENTED_EDGE('',*,*,#12023,.F.);
#16682=ORIENTED_EDGE('',*,*,#12026,.F.);
#16683=ORIENTED_EDGE('',*,*,#12029,.F.);
#16684=ORIENTED_EDGE('',*,*,#12040,.F.);
#16685=ORIENTED_EDGE('',*,*,#12033,.F.);
#16686=ORIENTED_EDGE('',*,*,#11652,.F.);
#16687=ORIENTED_EDGE('',*,*,#11656,.F.);
#16688=ORIENTED_EDGE('',*,*,#11659,.F.);
#16689=ORIENTED_EDGE('',*,*,#11662,.F.);
#16690=ORIENTED_EDGE('',*,*,#11665,.F.);
#16691=ORIENTED_EDGE('',*,*,#11668,.F.);
#16692=ORIENTED_EDGE('',*,*,#11671,.F.);
#16693=ORIENTED_EDGE('',*,*,#11674,.F.);
#16694=ORIENTED_EDGE('',*,*,#11677,.F.);
#16695=ORIENTED_EDGE('',*,*,#11680,.F.);
#16696=ORIENTED_EDGE('',*,*,#11683,.F.);
#16697=ORIENTED_EDGE('',*,*,#11686,.F.);
#16698=ORIENTED_EDGE('',*,*,#11689,.F.);
#16699=ORIENTED_EDGE('',*,*,#11692,.F.);
#16700=ORIENTED_EDGE('',*,*,#11695,.F.);
#16701=ORIENTED_EDGE('',*,*,#11698,.F.);
#16702=ORIENTED_EDGE('',*,*,#11701,.F.);
#16703=ORIENTED_EDGE('',*,*,#11704,.F.);
#16704=ORIENTED_EDGE('',*,*,#11707,.F.);
#16705=ORIENTED_EDGE('',*,*,#11710,.F.);
#16706=ORIENTED_EDGE('',*,*,#11713,.F.);
#16707=ORIENTED_EDGE('',*,*,#11716,.F.);
#16708=ORIENTED_EDGE('',*,*,#11719,.F.);
#16709=ORIENTED_EDGE('',*,*,#11722,.F.);
#16710=ORIENTED_EDGE('',*,*,#11725,.F.);
#16711=ORIENTED_EDGE('',*,*,#11728,.F.);
#16712=ORIENTED_EDGE('',*,*,#11731,.F.);
#16713=ORIENTED_EDGE('',*,*,#11734,.F.);
#16714=ORIENTED_EDGE('',*,*,#11737,.F.);
#16715=ORIENTED_EDGE('',*,*,#11740,.F.);
#16716=ORIENTED_EDGE('',*,*,#11743,.F.);
#16717=ORIENTED_EDGE('',*,*,#11746,.F.);
#16718=ORIENTED_EDGE('',*,*,#11749,.F.);
#16719=ORIENTED_EDGE('',*,*,#11752,.F.);
#16720=ORIENTED_EDGE('',*,*,#11755,.F.);
#16721=ORIENTED_EDGE('',*,*,#11758,.F.);
#16722=ORIENTED_EDGE('',*,*,#11761,.F.);
#16723=ORIENTED_EDGE('',*,*,#11764,.F.);
#16724=ORIENTED_EDGE('',*,*,#11767,.F.);
#16725=ORIENTED_EDGE('',*,*,#11770,.F.);
#16726=ORIENTED_EDGE('',*,*,#11773,.F.);
#16727=ORIENTED_EDGE('',*,*,#11776,.F.);
#16728=ORIENTED_EDGE('',*,*,#11779,.F.);
#16729=ORIENTED_EDGE('',*,*,#11782,.F.);
#16730=ORIENTED_EDGE('',*,*,#11785,.F.);
#16731=ORIENTED_EDGE('',*,*,#11788,.F.);
#16732=ORIENTED_EDGE('',*,*,#11791,.F.);
#16733=ORIENTED_EDGE('',*,*,#11794,.F.);
#16734=ORIENTED_EDGE('',*,*,#11797,.F.);
#16735=ORIENTED_EDGE('',*,*,#11800,.F.);
#16736=ORIENTED_EDGE('',*,*,#11803,.F.);
#16737=ORIENTED_EDGE('',*,*,#11806,.F.);
#16738=ORIENTED_EDGE('',*,*,#11809,.F.);
#16739=ORIENTED_EDGE('',*,*,#11812,.F.);
#16740=ORIENTED_EDGE('',*,*,#11815,.F.);
#16741=ORIENTED_EDGE('',*,*,#11818,.F.);
#16742=ORIENTED_EDGE('',*,*,#11821,.F.);
#16743=ORIENTED_EDGE('',*,*,#11824,.F.);
#16744=ORIENTED_EDGE('',*,*,#11827,.F.);
#16745=ORIENTED_EDGE('',*,*,#11830,.F.);
#16746=ORIENTED_EDGE('',*,*,#11833,.F.);
#16747=ORIENTED_EDGE('',*,*,#11836,.F.);
#16748=ORIENTED_EDGE('',*,*,#11839,.F.);
#16749=ORIENTED_EDGE('',*,*,#12042,.F.);
#16750=ORIENTED_EDGE('',*,*,#12043,.F.);
#16751=ORIENTED_EDGE('',*,*,#12044,.T.);
#16752=ORIENTED_EDGE('',*,*,#12045,.F.);
#16753=ORIENTED_EDGE('',*,*,#12046,.F.);
#16754=ORIENTED_EDGE('',*,*,#12047,.F.);
#16755=ORIENTED_EDGE('',*,*,#12046,.T.);
#16756=ORIENTED_EDGE('',*,*,#12048,.T.);
#16757=ORIENTED_EDGE('',*,*,#12049,.T.);
#16758=ORIENTED_EDGE('',*,*,#12048,.F.);
#16759=ORIENTED_EDGE('',*,*,#12045,.T.);
#16760=ORIENTED_EDGE('',*,*,#12050,.T.);
#16761=ORIENTED_EDGE('',*,*,#12051,.F.);
#16762=ORIENTED_EDGE('',*,*,#12052,.F.);
#16763=ORIENTED_EDGE('',*,*,#12049,.F.);
#16764=ORIENTED_EDGE('',*,*,#12051,.T.);
#16765=ORIENTED_EDGE('',*,*,#12053,.T.);
#16766=ORIENTED_EDGE('',*,*,#12054,.F.);
#16767=ORIENTED_EDGE('',*,*,#12053,.F.);
#16768=ORIENTED_EDGE('',*,*,#12050,.F.);
#16769=ORIENTED_EDGE('',*,*,#12044,.F.);
#16770=ORIENTED_EDGE('',*,*,#12055,.F.);
#16771=ORIENTED_EDGE('',*,*,#12056,.T.);
#16772=ORIENTED_EDGE('',*,*,#12057,.F.);
#16773=ORIENTED_EDGE('',*,*,#12056,.F.);
#16774=ORIENTED_EDGE('',*,*,#12052,.T.);
#16775=ORIENTED_EDGE('',*,*,#12054,.T.);
#16776=ORIENTED_EDGE('',*,*,#12043,.T.);
#16777=ORIENTED_EDGE('',*,*,#12047,.T.);
#16778=ORIENTED_EDGE('',*,*,#12055,.T.);
#16779=ORIENTED_EDGE('',*,*,#12058,.F.);
#16780=ORIENTED_EDGE('',*,*,#12059,.T.);
#16781=ORIENTED_EDGE('',*,*,#12037,.T.);
#16782=ORIENTED_EDGE('',*,*,#11846,.T.);
#16783=ORIENTED_EDGE('',*,*,#11843,.T.);
#16784=ORIENTED_EDGE('',*,*,#12041,.T.);
#16785=ORIENTED_EDGE('',*,*,#12060,.F.);
#16786=ORIENTED_EDGE('',*,*,#12061,.T.);
#16787=ORIENTED_EDGE('',*,*,#12058,.T.);
#16788=ORIENTED_EDGE('',*,*,#12061,.F.);
#16789=ORIENTED_EDGE('',*,*,#12060,.T.);
#16790=ORIENTED_EDGE('',*,*,#12057,.T.);
#16791=ORIENTED_EDGE('',*,*,#11838,.T.);
#16792=ORIENTED_EDGE('',*,*,#12038,.T.);
#16793=ORIENTED_EDGE('',*,*,#12059,.F.);
#16794=ORIENTED_EDGE('',*,*,#12042,.T.);
#16795=ORIENTED_EDGE('',*,*,#12062,.F.);
#16796=ORIENTED_EDGE('',*,*,#12063,.T.);
#16797=ORIENTED_EDGE('',*,*,#12064,.T.);
#16798=ORIENTED_EDGE('',*,*,#12063,.F.);
#16799=ORIENTED_EDGE('',*,*,#12065,.F.);
#16800=ORIENTED_EDGE('',*,*,#12066,.T.);
#16801=ORIENTED_EDGE('',*,*,#12067,.T.);
#16802=ORIENTED_EDGE('',*,*,#12066,.F.);
#16803=ORIENTED_EDGE('',*,*,#12065,.T.);
#16804=ORIENTED_EDGE('',*,*,#12062,.T.);
#16805=ORIENTED_EDGE('',*,*,#12067,.F.);
#16806=ORIENTED_EDGE('',*,*,#12064,.F.);
#16807=ORIENTED_EDGE('',*,*,#12068,.F.);
#16808=ORIENTED_EDGE('',*,*,#12069,.T.);
#16809=ORIENTED_EDGE('',*,*,#12070,.F.);
#16810=ORIENTED_EDGE('',*,*,#12071,.F.);
#16811=ORIENTED_EDGE('',*,*,#12072,.F.);
#16812=ORIENTED_EDGE('',*,*,#12069,.F.);
#16813=ORIENTED_EDGE('',*,*,#12073,.F.);
#16814=ORIENTED_EDGE('',*,*,#12074,.T.);
#16815=ORIENTED_EDGE('',*,*,#12075,.F.);
#16816=ORIENTED_EDGE('',*,*,#12076,.F.);
#16817=ORIENTED_EDGE('',*,*,#12074,.F.);
#16818=ORIENTED_EDGE('',*,*,#12077,.F.);
#16819=ORIENTED_EDGE('',*,*,#12071,.T.);
#16820=ORIENTED_EDGE('',*,*,#12078,.F.);
#16821=ORIENTED_EDGE('',*,*,#12079,.T.);
#16822=ORIENTED_EDGE('',*,*,#12080,.T.);
#16823=ORIENTED_EDGE('',*,*,#12079,.F.);
#16824=ORIENTED_EDGE('',*,*,#12072,.T.);
#16825=ORIENTED_EDGE('',*,*,#12077,.T.);
#16826=ORIENTED_EDGE('',*,*,#12070,.T.);
#16827=ORIENTED_EDGE('',*,*,#12073,.T.);
#16828=ORIENTED_EDGE('',*,*,#12068,.T.);
#16829=ORIENTED_EDGE('',*,*,#12081,.F.);
#16830=ORIENTED_EDGE('',*,*,#12082,.T.);
#16831=ORIENTED_EDGE('',*,*,#12083,.T.);
#16832=ORIENTED_EDGE('',*,*,#12082,.F.);
#16833=ORIENTED_EDGE('',*,*,#12075,.T.);
#16834=ORIENTED_EDGE('',*,*,#12076,.T.);
#16835=ORIENTED_EDGE('',*,*,#12081,.T.);
#16836=ORIENTED_EDGE('',*,*,#12078,.T.);
#16837=ORIENTED_EDGE('',*,*,#12083,.F.);
#16838=ORIENTED_EDGE('',*,*,#12080,.F.);
#16839=ORIENTED_EDGE('',*,*,#12084,.F.);
#16840=ORIENTED_EDGE('',*,*,#12085,.T.);
#16841=ORIENTED_EDGE('',*,*,#12086,.F.);
#16842=ORIENTED_EDGE('',*,*,#12085,.F.);
#16843=ORIENTED_EDGE('',*,*,#12087,.F.);
#16844=ORIENTED_EDGE('',*,*,#12088,.T.);
#16845=ORIENTED_EDGE('',*,*,#12089,.F.);
#16846=ORIENTED_EDGE('',*,*,#12090,.F.);
#16847=ORIENTED_EDGE('',*,*,#12091,.F.);
#16848=ORIENTED_EDGE('',*,*,#12088,.F.);
#16849=ORIENTED_EDGE('',*,*,#12092,.F.);
#16850=ORIENTED_EDGE('',*,*,#12093,.T.);
#16851=ORIENTED_EDGE('',*,*,#12094,.F.);
#16852=ORIENTED_EDGE('',*,*,#12095,.F.);
#16853=ORIENTED_EDGE('',*,*,#12093,.F.);
#16854=ORIENTED_EDGE('',*,*,#12096,.F.);
#16855=ORIENTED_EDGE('',*,*,#12090,.T.);
#16856=ORIENTED_EDGE('',*,*,#12097,.F.);
#16857=ORIENTED_EDGE('',*,*,#12098,.F.);
#16858=ORIENTED_EDGE('',*,*,#12099,.F.);
#16859=ORIENTED_EDGE('',*,*,#12100,.F.);
#16860=ORIENTED_EDGE('',*,*,#12101,.F.);
#16861=ORIENTED_EDGE('',*,*,#12102,.F.);
#16862=ORIENTED_EDGE('',*,*,#12103,.F.);
#16863=ORIENTED_EDGE('',*,*,#12104,.F.);
#16864=ORIENTED_EDGE('',*,*,#12105,.F.);
#16865=ORIENTED_EDGE('',*,*,#12098,.T.);
#16866=ORIENTED_EDGE('',*,*,#12106,.F.);
#16867=ORIENTED_EDGE('',*,*,#12107,.F.);
#16868=ORIENTED_EDGE('',*,*,#12108,.F.);
#16869=ORIENTED_EDGE('',*,*,#12109,.F.);
#16870=ORIENTED_EDGE('',*,*,#12110,.F.);
#16871=ORIENTED_EDGE('',*,*,#12104,.T.);
#16872=ORIENTED_EDGE('',*,*,#12111,.T.);
#16873=ORIENTED_EDGE('',*,*,#12086,.T.);
#16874=ORIENTED_EDGE('',*,*,#12106,.T.);
#16875=ORIENTED_EDGE('',*,*,#12103,.T.);
#16876=ORIENTED_EDGE('',*,*,#12097,.T.);
#16877=ORIENTED_EDGE('',*,*,#12112,.T.);
#16878=ORIENTED_EDGE('',*,*,#12113,.F.);
#16879=ORIENTED_EDGE('',*,*,#12084,.T.);
#16880=ORIENTED_EDGE('',*,*,#12110,.T.);
#16881=ORIENTED_EDGE('',*,*,#12114,.T.);
#16882=ORIENTED_EDGE('',*,*,#12099,.T.);
#16883=ORIENTED_EDGE('',*,*,#12105,.T.);
#16884=ORIENTED_EDGE('',*,*,#12111,.F.);
#16885=ORIENTED_EDGE('',*,*,#12115,.T.);
#16886=ORIENTED_EDGE('',*,*,#12113,.T.);
#16887=ORIENTED_EDGE('',*,*,#12115,.F.);
#16888=ORIENTED_EDGE('',*,*,#12107,.T.);
#16889=ORIENTED_EDGE('',*,*,#12112,.F.);
#16890=ORIENTED_EDGE('',*,*,#12102,.T.);
#16891=ORIENTED_EDGE('',*,*,#12116,.T.);
#16892=ORIENTED_EDGE('',*,*,#12091,.T.);
#16893=ORIENTED_EDGE('',*,*,#12096,.T.);
#16894=ORIENTED_EDGE('',*,*,#12089,.T.);
#16895=ORIENTED_EDGE('',*,*,#12092,.T.);
#16896=ORIENTED_EDGE('',*,*,#12087,.T.);
#16897=ORIENTED_EDGE('',*,*,#12109,.T.);
#16898=ORIENTED_EDGE('',*,*,#12117,.T.);
#16899=ORIENTED_EDGE('',*,*,#12100,.T.);
#16900=ORIENTED_EDGE('',*,*,#12114,.F.);
#16901=ORIENTED_EDGE('',*,*,#12094,.T.);
#16902=ORIENTED_EDGE('',*,*,#12095,.T.);
#16903=ORIENTED_EDGE('',*,*,#12108,.T.);
#16904=ORIENTED_EDGE('',*,*,#12116,.F.);
#16905=ORIENTED_EDGE('',*,*,#12101,.T.);
#16906=ORIENTED_EDGE('',*,*,#12117,.F.);
#16907=ORIENTED_EDGE('',*,*,#12118,.F.);
#16908=ORIENTED_EDGE('',*,*,#12119,.T.);
#16909=ORIENTED_EDGE('',*,*,#12120,.T.);
#16910=ORIENTED_EDGE('',*,*,#12119,.F.);
#16911=ORIENTED_EDGE('',*,*,#12121,.F.);
#16912=ORIENTED_EDGE('',*,*,#12122,.T.);
#16913=ORIENTED_EDGE('',*,*,#12123,.T.);
#16914=ORIENTED_EDGE('',*,*,#12122,.F.);
#16915=ORIENTED_EDGE('',*,*,#12121,.T.);
#16916=ORIENTED_EDGE('',*,*,#12118,.T.);
#16917=ORIENTED_EDGE('',*,*,#12123,.F.);
#16918=ORIENTED_EDGE('',*,*,#12120,.F.);
#16919=ORIENTED_EDGE('',*,*,#12124,.F.);
#16920=ORIENTED_EDGE('',*,*,#12125,.T.);
#16921=ORIENTED_EDGE('',*,*,#12126,.T.);
#16922=ORIENTED_EDGE('',*,*,#12125,.F.);
#16923=ORIENTED_EDGE('',*,*,#12127,.F.);
#16924=ORIENTED_EDGE('',*,*,#12128,.T.);
#16925=ORIENTED_EDGE('',*,*,#12129,.T.);
#16926=ORIENTED_EDGE('',*,*,#12128,.F.);
#16927=ORIENTED_EDGE('',*,*,#12127,.T.);
#16928=ORIENTED_EDGE('',*,*,#12124,.T.);
#16929=ORIENTED_EDGE('',*,*,#12129,.F.);
#16930=ORIENTED_EDGE('',*,*,#12126,.F.);
#16931=ORIENTED_EDGE('',*,*,#12130,.F.);
#16932=ORIENTED_EDGE('',*,*,#12131,.F.);
#16933=ORIENTED_EDGE('',*,*,#12132,.F.);
#16934=ORIENTED_EDGE('',*,*,#12133,.F.);
#16935=ORIENTED_EDGE('',*,*,#12134,.F.);
#16936=ORIENTED_EDGE('',*,*,#12135,.F.);
#16937=ORIENTED_EDGE('',*,*,#12136,.F.);
#16938=ORIENTED_EDGE('',*,*,#12137,.F.);
#16939=ORIENTED_EDGE('',*,*,#12134,.T.);
#16940=ORIENTED_EDGE('',*,*,#12138,.T.);
#16941=ORIENTED_EDGE('',*,*,#12139,.T.);
#16942=ORIENTED_EDGE('',*,*,#12140,.T.);
#16943=ORIENTED_EDGE('',*,*,#12133,.T.);
#16944=ORIENTED_EDGE('',*,*,#12141,.F.);
#16945=ORIENTED_EDGE('',*,*,#12142,.T.);
#16946=ORIENTED_EDGE('',*,*,#12138,.F.);
#16947=ORIENTED_EDGE('',*,*,#12132,.T.);
#16948=ORIENTED_EDGE('',*,*,#12143,.T.);
#16949=ORIENTED_EDGE('',*,*,#12144,.T.);
#16950=ORIENTED_EDGE('',*,*,#12141,.T.);
#16951=ORIENTED_EDGE('',*,*,#12131,.T.);
#16952=ORIENTED_EDGE('',*,*,#12145,.F.);
#16953=ORIENTED_EDGE('',*,*,#12146,.T.);
#16954=ORIENTED_EDGE('',*,*,#12143,.F.);
#16955=ORIENTED_EDGE('',*,*,#12147,.F.);
#16956=ORIENTED_EDGE('',*,*,#12148,.F.);
#16957=ORIENTED_EDGE('',*,*,#12139,.F.);
#16958=ORIENTED_EDGE('',*,*,#12142,.F.);
#16959=ORIENTED_EDGE('',*,*,#12144,.F.);
#16960=ORIENTED_EDGE('',*,*,#12146,.F.);
#16961=ORIENTED_EDGE('',*,*,#12149,.F.);
#16962=ORIENTED_EDGE('',*,*,#12150,.F.);
#16963=ORIENTED_EDGE('',*,*,#12135,.T.);
#16964=ORIENTED_EDGE('',*,*,#12140,.F.);
#16965=ORIENTED_EDGE('',*,*,#12148,.T.);
#16966=ORIENTED_EDGE('',*,*,#12151,.F.);
#16967=ORIENTED_EDGE('',*,*,#12130,.T.);
#16968=ORIENTED_EDGE('',*,*,#12152,.T.);
#16969=ORIENTED_EDGE('',*,*,#12149,.T.);
#16970=ORIENTED_EDGE('',*,*,#12145,.T.);
#16971=ORIENTED_EDGE('',*,*,#12136,.T.);
#16972=ORIENTED_EDGE('',*,*,#12151,.T.);
#16973=ORIENTED_EDGE('',*,*,#12147,.T.);
#16974=ORIENTED_EDGE('',*,*,#12153,.T.);
#16975=ORIENTED_EDGE('',*,*,#12137,.T.);
#16976=ORIENTED_EDGE('',*,*,#12153,.F.);
#16977=ORIENTED_EDGE('',*,*,#12150,.T.);
#16978=ORIENTED_EDGE('',*,*,#12152,.F.);
#16979=ORIENTED_EDGE('',*,*,#12154,.F.);
#16980=ORIENTED_EDGE('',*,*,#12155,.T.);
#16981=ORIENTED_EDGE('',*,*,#12156,.T.);
#16982=ORIENTED_EDGE('',*,*,#12157,.F.);
#16983=ORIENTED_EDGE('',*,*,#12158,.F.);
#16984=ORIENTED_EDGE('',*,*,#12159,.T.);
#16985=ORIENTED_EDGE('',*,*,#12160,.T.);
#16986=ORIENTED_EDGE('',*,*,#12155,.F.);
#16987=ORIENTED_EDGE('',*,*,#12161,.F.);
#16988=ORIENTED_EDGE('',*,*,#12162,.T.);
#16989=ORIENTED_EDGE('',*,*,#12163,.T.);
#16990=ORIENTED_EDGE('',*,*,#12159,.F.);
#16991=ORIENTED_EDGE('',*,*,#12164,.F.);
#16992=ORIENTED_EDGE('',*,*,#12165,.T.);
#16993=ORIENTED_EDGE('',*,*,#12166,.T.);
#16994=ORIENTED_EDGE('',*,*,#12162,.F.);
#16995=ORIENTED_EDGE('',*,*,#12167,.F.);
#16996=ORIENTED_EDGE('',*,*,#12168,.T.);
#16997=ORIENTED_EDGE('',*,*,#12169,.T.);
#16998=ORIENTED_EDGE('',*,*,#12165,.F.);
#16999=ORIENTED_EDGE('',*,*,#12170,.F.);
#17000=ORIENTED_EDGE('',*,*,#12157,.T.);
#17001=ORIENTED_EDGE('',*,*,#12171,.T.);
#17002=ORIENTED_EDGE('',*,*,#12168,.F.);
#17003=ORIENTED_EDGE('',*,*,#12171,.F.);
#17004=ORIENTED_EDGE('',*,*,#12156,.F.);
#17005=ORIENTED_EDGE('',*,*,#12160,.F.);
#17006=ORIENTED_EDGE('',*,*,#12163,.F.);
#17007=ORIENTED_EDGE('',*,*,#12166,.F.);
#17008=ORIENTED_EDGE('',*,*,#12169,.F.);
#17009=ORIENTED_EDGE('',*,*,#12172,.F.);
#17010=ORIENTED_EDGE('',*,*,#12154,.T.);
#17011=ORIENTED_EDGE('',*,*,#12170,.T.);
#17012=ORIENTED_EDGE('',*,*,#12167,.T.);
#17013=ORIENTED_EDGE('',*,*,#12164,.T.);
#17014=ORIENTED_EDGE('',*,*,#12161,.T.);
#17015=ORIENTED_EDGE('',*,*,#12158,.T.);
#17016=ORIENTED_EDGE('',*,*,#12173,.F.);
#17017=ORIENTED_EDGE('',*,*,#12174,.T.);
#17018=ORIENTED_EDGE('',*,*,#12172,.T.);
#17019=ORIENTED_EDGE('',*,*,#12174,.F.);
#17020=ORIENTED_EDGE('',*,*,#12175,.F.);
#17021=ORIENTED_EDGE('',*,*,#12176,.T.);
#17022=ORIENTED_EDGE('',*,*,#12173,.T.);
#17023=ORIENTED_EDGE('',*,*,#12176,.F.);
#17024=ORIENTED_EDGE('',*,*,#12177,.F.);
#17025=ORIENTED_EDGE('',*,*,#12178,.T.);
#17026=ORIENTED_EDGE('',*,*,#12175,.T.);
#17027=ORIENTED_EDGE('',*,*,#12178,.F.);
#17028=ORIENTED_EDGE('',*,*,#12177,.T.);
#17029=ORIENTED_EDGE('',*,*,#12179,.F.);
#17030=ORIENTED_EDGE('',*,*,#12180,.T.);
#17031=ORIENTED_EDGE('',*,*,#12181,.T.);
#17032=ORIENTED_EDGE('',*,*,#12180,.F.);
#17033=ORIENTED_EDGE('',*,*,#12182,.F.);
#17034=ORIENTED_EDGE('',*,*,#12183,.T.);
#17035=ORIENTED_EDGE('',*,*,#12184,.T.);
#17036=ORIENTED_EDGE('',*,*,#12183,.F.);
#17037=ORIENTED_EDGE('',*,*,#12182,.T.);
#17038=ORIENTED_EDGE('',*,*,#12179,.T.);
#17039=ORIENTED_EDGE('',*,*,#12184,.F.);
#17040=ORIENTED_EDGE('',*,*,#12181,.F.);
#17041=ORIENTED_EDGE('',*,*,#12185,.F.);
#17042=ORIENTED_EDGE('',*,*,#12186,.F.);
#17043=ORIENTED_EDGE('',*,*,#12187,.T.);
#17044=ORIENTED_EDGE('',*,*,#12185,.T.);
#17045=ORIENTED_EDGE('',*,*,#12187,.F.);
#17046=ORIENTED_EDGE('',*,*,#12188,.F.);
#17047=ORIENTED_EDGE('',*,*,#12189,.T.);
#17048=ORIENTED_EDGE('',*,*,#12186,.T.);
#17049=ORIENTED_EDGE('',*,*,#12189,.F.);
#17050=ORIENTED_EDGE('',*,*,#12190,.F.);
#17051=ORIENTED_EDGE('',*,*,#12191,.T.);
#17052=ORIENTED_EDGE('',*,*,#12188,.T.);
#17053=ORIENTED_EDGE('',*,*,#12191,.F.);
#17054=ORIENTED_EDGE('',*,*,#12190,.T.);
#17055=ORIENTED_EDGE('',*,*,#12192,.F.);
#17056=ORIENTED_EDGE('',*,*,#12193,.F.);
#17057=ORIENTED_EDGE('',*,*,#12194,.T.);
#17058=ORIENTED_EDGE('',*,*,#12192,.T.);
#17059=ORIENTED_EDGE('',*,*,#12194,.F.);
#17060=ORIENTED_EDGE('',*,*,#12195,.F.);
#17061=ORIENTED_EDGE('',*,*,#12196,.T.);
#17062=ORIENTED_EDGE('',*,*,#12193,.T.);
#17063=ORIENTED_EDGE('',*,*,#12196,.F.);
#17064=ORIENTED_EDGE('',*,*,#12197,.F.);
#17065=ORIENTED_EDGE('',*,*,#12198,.T.);
#17066=ORIENTED_EDGE('',*,*,#12195,.T.);
#17067=ORIENTED_EDGE('',*,*,#12198,.F.);
#17068=ORIENTED_EDGE('',*,*,#12197,.T.);
#17069=ORIENTED_EDGE('',*,*,#12199,.T.);
#17070=ORIENTED_EDGE('',*,*,#12200,.T.);
#17071=ORIENTED_EDGE('',*,*,#12201,.T.);
#17072=ORIENTED_EDGE('',*,*,#12202,.F.);
#17073=ORIENTED_EDGE('',*,*,#12203,.T.);
#17074=ORIENTED_EDGE('',*,*,#12204,.T.);
#17075=ORIENTED_EDGE('',*,*,#12205,.T.);
#17076=ORIENTED_EDGE('',*,*,#12200,.F.);
#17077=ORIENTED_EDGE('',*,*,#12206,.T.);
#17078=ORIENTED_EDGE('',*,*,#12207,.T.);
#17079=ORIENTED_EDGE('',*,*,#12208,.T.);
#17080=ORIENTED_EDGE('',*,*,#12204,.F.);
#17081=ORIENTED_EDGE('',*,*,#12209,.T.);
#17082=ORIENTED_EDGE('',*,*,#12210,.T.);
#17083=ORIENTED_EDGE('',*,*,#12211,.T.);
#17084=ORIENTED_EDGE('',*,*,#12207,.F.);
#17085=ORIENTED_EDGE('',*,*,#12212,.T.);
#17086=ORIENTED_EDGE('',*,*,#12213,.T.);
#17087=ORIENTED_EDGE('',*,*,#12214,.T.);
#17088=ORIENTED_EDGE('',*,*,#12210,.F.);
#17089=ORIENTED_EDGE('',*,*,#12215,.T.);
#17090=ORIENTED_EDGE('',*,*,#12202,.T.);
#17091=ORIENTED_EDGE('',*,*,#12216,.T.);
#17092=ORIENTED_EDGE('',*,*,#12213,.F.);
#17093=ORIENTED_EDGE('',*,*,#12215,.F.);
#17094=ORIENTED_EDGE('',*,*,#12212,.F.);
#17095=ORIENTED_EDGE('',*,*,#12209,.F.);
#17096=ORIENTED_EDGE('',*,*,#12206,.F.);
#17097=ORIENTED_EDGE('',*,*,#12203,.F.);
#17098=ORIENTED_EDGE('',*,*,#12199,.F.);
#17099=ORIENTED_EDGE('',*,*,#12216,.F.);
#17100=ORIENTED_EDGE('',*,*,#12201,.F.);
#17101=ORIENTED_EDGE('',*,*,#12205,.F.);
#17102=ORIENTED_EDGE('',*,*,#12208,.F.);
#17103=ORIENTED_EDGE('',*,*,#12211,.F.);
#17104=ORIENTED_EDGE('',*,*,#12214,.F.);
#17105=CYLINDRICAL_SURFACE('',#19287,0.275);
#17106=CYLINDRICAL_SURFACE('',#19295,0.165);
#17107=CYLINDRICAL_SURFACE('',#19299,0.165);
#17108=CYLINDRICAL_SURFACE('',#19303,0.165);
#17109=CYLINDRICAL_SURFACE('',#19307,0.165);
#17110=CYLINDRICAL_SURFACE('',#19311,0.275);
#17111=CYLINDRICAL_SURFACE('',#19314,0.275);
#17112=CYLINDRICAL_SURFACE('',#19317,0.275);
#17113=CYLINDRICAL_SURFACE('',#19320,0.275);
#17114=CYLINDRICAL_SURFACE('',#19323,0.275);
#17115=CYLINDRICAL_SURFACE('',#19326,0.275);
#17116=CYLINDRICAL_SURFACE('',#19329,2.5);
#17117=CYLINDRICAL_SURFACE('',#19332,0.275);
#17118=CYLINDRICAL_SURFACE('',#19335,0.275);
#17119=CYLINDRICAL_SURFACE('',#19338,0.275);
#17120=CYLINDRICAL_SURFACE('',#19341,0.275);
#17121=CYLINDRICAL_SURFACE('',#19344,0.275);
#17122=CYLINDRICAL_SURFACE('',#19347,0.275);
#17123=CYLINDRICAL_SURFACE('',#19350,0.275);
#17124=CYLINDRICAL_SURFACE('',#19353,0.275);
#17125=CYLINDRICAL_SURFACE('',#19376,0.275);
#17126=CYLINDRICAL_SURFACE('',#19379,0.275);
#17127=CYLINDRICAL_SURFACE('',#19382,0.275);
#17128=CYLINDRICAL_SURFACE('',#19385,0.275);
#17129=CYLINDRICAL_SURFACE('',#19388,0.275);
#17130=CYLINDRICAL_SURFACE('',#19391,0.275);
#17131=CYLINDRICAL_SURFACE('',#19394,0.275);
#17132=CYLINDRICAL_SURFACE('',#19397,0.275);
#17133=CYLINDRICAL_SURFACE('',#19404,0.61);
#17134=CYLINDRICAL_SURFACE('',#19407,0.61);
#17135=CYLINDRICAL_SURFACE('',#19417,0.274999999999999);
#17136=CYLINDRICAL_SURFACE('',#19420,0.274999999999999);
#17137=CYLINDRICAL_SURFACE('',#19423,0.21);
#17138=CYLINDRICAL_SURFACE('',#19427,0.21);
#17139=CYLINDRICAL_SURFACE('',#19431,0.21);
#17140=CYLINDRICAL_SURFACE('',#19435,0.21);
#17141=CYLINDRICAL_SURFACE('',#19446,0.274999999999999);
#17142=CYLINDRICAL_SURFACE('',#19449,0.274999999999999);
#17143=CYLINDRICAL_SURFACE('',#19452,0.21);
#17144=CYLINDRICAL_SURFACE('',#19456,0.21);
#17145=CYLINDRICAL_SURFACE('',#19460,0.21);
#17146=CYLINDRICAL_SURFACE('',#19464,0.21);
#17147=CYLINDRICAL_SURFACE('',#19475,0.21);
#17148=CYLINDRICAL_SURFACE('',#19479,0.21);
#17149=CYLINDRICAL_SURFACE('',#19483,0.21);
#17150=CYLINDRICAL_SURFACE('',#19486,0.21);
#17151=CYLINDRICAL_SURFACE('',#19496,0.21);
#17152=CYLINDRICAL_SURFACE('',#19499,0.21);
#17153=CYLINDRICAL_SURFACE('',#19502,0.21);
#17154=CYLINDRICAL_SURFACE('',#19508,0.21);
#17155=CYLINDRICAL_SURFACE('',#19523,0.21);
#17156=CYLINDRICAL_SURFACE('',#19527,0.21);
#17157=CYLINDRICAL_SURFACE('',#19531,0.21);
#17158=CYLINDRICAL_SURFACE('',#19534,0.21);
#17159=CYLINDRICAL_SURFACE('',#19544,0.21);
#17160=CYLINDRICAL_SURFACE('',#19547,0.21);
#17161=CYLINDRICAL_SURFACE('',#19550,0.21);
#17162=CYLINDRICAL_SURFACE('',#19556,0.21);
#17163=CYLINDRICAL_SURFACE('',#19571,0.165);
#17164=CYLINDRICAL_SURFACE('',#19574,0.165);
#17165=CYLINDRICAL_SURFACE('',#19577,0.165);
#17166=CYLINDRICAL_SURFACE('',#19580,0.21);
#17167=CYLINDRICAL_SURFACE('',#19584,0.21);
#17168=CYLINDRICAL_SURFACE('',#19588,0.21);
#17169=CYLINDRICAL_SURFACE('',#19592,0.21);
#17170=CYLINDRICAL_SURFACE('',#19596,1.6);
#17171=CYLINDRICAL_SURFACE('',#19601,1.4);
#17172=CYLINDRICAL_SURFACE('',#19603,2.5);
#17173=CYLINDRICAL_SURFACE('',#19614,0.275);
#17174=CYLINDRICAL_SURFACE('',#19617,0.275);
#17175=CYLINDRICAL_SURFACE('',#19620,0.165);
#17176=CYLINDRICAL_SURFACE('',#19623,0.165);
#17177=CYLINDRICAL_SURFACE('',#19626,0.165);
#17178=CYLINDRICAL_SURFACE('',#19629,0.210000000000001);
#17179=CYLINDRICAL_SURFACE('',#19633,0.210000000000001);
#17180=CYLINDRICAL_SURFACE('',#19637,0.210000000000001);
#17181=CYLINDRICAL_SURFACE('',#19641,0.210000000000001);
#17182=CYLINDRICAL_SURFACE('',#19645,2.35);
#17183=CYLINDRICAL_SURFACE('',#19650,2.15);
#17184=CYLINDRICAL_SURFACE('',#19652,0.625);
#17185=CYLINDRICAL_SURFACE('',#19655,0.625);
#17186=CYLINDRICAL_SURFACE('',#19665,0.225);
#17187=CYLINDRICAL_SURFACE('',#19668,0.225);
#17188=CYLINDRICAL_SURFACE('',#19671,0.225);
#17189=CYLINDRICAL_SURFACE('',#19674,1.59);
#17190=CYLINDRICAL_SURFACE('',#19679,1.2);
#17191=CYLINDRICAL_SURFACE('',#19681,2.4);
#17192=CYLINDRICAL_SURFACE('',#19687,0.225);
#17193=CYLINDRICAL_SURFACE('',#19690,0.225);
#17194=CYLINDRICAL_SURFACE('',#19693,0.225);
#17195=CYLINDRICAL_SURFACE('',#19696,2.34);
#17196=CYLINDRICAL_SURFACE('',#19701,1.8);
#17197=CYLINDRICAL_SURFACE('',#19703,3.);
#17198=CYLINDRICAL_SURFACE('',#19709,0.21);
#17199=CYLINDRICAL_SURFACE('',#19713,0.5);
#17200=CYLINDRICAL_SURFACE('',#19719,0.21);
#17201=CYLINDRICAL_SURFACE('',#19723,0.5);
#17202=CYLINDRICAL_SURFACE('',#19729,0.21);
#17203=CYLINDRICAL_SURFACE('',#19733,0.5);
#17204=CYLINDRICAL_SURFACE('',#19739,0.21);
#17205=CYLINDRICAL_SURFACE('',#19743,0.5);
#17206=CYLINDRICAL_SURFACE('',#19749,0.375);
#17207=CYLINDRICAL_SURFACE('',#19754,0.375);
#17208=CYLINDRICAL_SURFACE('',#19759,0.375);
#17209=CYLINDRICAL_SURFACE('',#19764,0.375);
#17210=CYLINDRICAL_SURFACE('',#19769,0.225);
#17211=CYLINDRICAL_SURFACE('',#19771,0.225);
#17212=CYLINDRICAL_SURFACE('',#19773,0.225);
#17213=CYLINDRICAL_SURFACE('',#19775,0.225);
#17214=CYLINDRICAL_SURFACE('',#19777,3.);
#17215=CYLINDRICAL_SURFACE('',#19908,0.274999999999999);
#17216=CYLINDRICAL_SURFACE('',#19911,0.275);
#17217=CYLINDRICAL_SURFACE('',#19924,0.6);
#17218=CYLINDRICAL_SURFACE('',#19933,0.525);
#17219=CYLINDRICAL_SURFACE('',#19935,0.525);
#17220=CYLINDRICAL_SURFACE('',#19945,0.225);
#17221=CYLINDRICAL_SURFACE('',#19948,0.165);
#17222=CYLINDRICAL_SURFACE('',#19950,0.275);
#17223=CYLINDRICAL_SURFACE('',#19952,0.275);
#17224=CYLINDRICAL_SURFACE('',#19954,0.6);
#17225=CYLINDRICAL_SURFACE('',#19983,0.425);
#17226=CYLINDRICAL_SURFACE('',#19991,0.24505);
#17227=CYLINDRICAL_SURFACE('',#20000,1.070235);
#17228=CYLINDRICAL_SURFACE('',#20002,0.6);
#17229=CYLINDRICAL_SURFACE('',#20008,1.070235);
#17230=CYLINDRICAL_SURFACE('',#20020,1.129765);
#17231=CYLINDRICAL_SURFACE('',#20027,1.6);
#17232=CYLINDRICAL_SURFACE('',#20032,1.129765);
#17233=CYLINDRICAL_SURFACE('',#20052,1.123812);
#17234=CYLINDRICAL_SURFACE('',#20088,1.076188);
#17235=CYLINDRICAL_SURFACE('',#20102,1.119765);
#17236=CYLINDRICAL_SURFACE('',#20106,1.085235);
#17237=CYLINDRICAL_SURFACE('',#20110,1.119765);
#17238=CYLINDRICAL_SURFACE('',#20114,1.085235);
#17239=CYLINDRICAL_SURFACE('',#20128,1.63531);
#17240=CYLINDRICAL_SURFACE('',#20130,1.);
#17241=CYLINDRICAL_SURFACE('',#20136,1.63531);
#17242=CYLINDRICAL_SURFACE('',#20148,1.71469);
#17243=CYLINDRICAL_SURFACE('',#20155,2.35);
#17244=CYLINDRICAL_SURFACE('',#20160,1.71469);
#17245=CYLINDRICAL_SURFACE('',#20182,1.706752);
#17246=CYLINDRICAL_SURFACE('',#20222,1.643248);
#17247=CYLINDRICAL_SURFACE('',#20236,1.70469);
#17248=CYLINDRICAL_SURFACE('',#20240,1.65031);
#17249=CYLINDRICAL_SURFACE('',#20244,1.70469);
#17250=CYLINDRICAL_SURFACE('',#20248,1.65031);
#17251=CYLINDRICAL_SURFACE('',#20260,0.25);
#17252=CYLINDRICAL_SURFACE('',#20265,0.425);
#17253=CYLINDRICAL_SURFACE('',#20273,0.24505);
#17254=CYLINDRICAL_SURFACE('',#20297,0.35);
#17255=CYLINDRICAL_SURFACE('',#20305,0.1954);
#17256=CYLINDRICAL_SURFACE('',#20343,0.21);
#17257=CYLINDRICAL_SURFACE('',#20361,0.425);
#17258=CYLINDRICAL_SURFACE('',#20369,0.24505);
#17259=CYLINDRICAL_SURFACE('',#20394,0.2117);
#17260=CYLINDRICAL_SURFACE('',#20410,0.425);
#17261=CYLINDRICAL_SURFACE('',#20418,0.24505);
#17262=CYLINDRICAL_SURFACE('',#20428,0.165);
#17263=CYLINDRICAL_SURFACE('',#20431,0.165);
#17264=CYLINDRICAL_SURFACE('',#20434,0.225);
#17265=CYLINDRICAL_SURFACE('',#20437,0.225);
#17266=CYLINDRICAL_SURFACE('',#20440,0.225);
#17267=CYLINDRICAL_SURFACE('',#20443,0.225);
#17268=CYLINDRICAL_SURFACE('',#20446,0.225);
#17269=CYLINDRICAL_SURFACE('',#20449,0.225);
#17270=CYLINDRICAL_SURFACE('',#20452,0.225);
#17271=CYLINDRICAL_SURFACE('',#20455,0.225);
#17272=CYLINDRICAL_SURFACE('',#20458,0.225);
#17273=CYLINDRICAL_SURFACE('',#20461,0.225);
#17274=CYLINDRICAL_SURFACE('',#20464,0.225);
#17275=CYLINDRICAL_SURFACE('',#20467,0.225);
#17276=CYLINDRICAL_SURFACE('',#20470,0.225);
#17277=CYLINDRICAL_SURFACE('',#20473,0.625);
#17278=CYLINDRICAL_SURFACE('',#20476,0.625);
#17279=CYLINDRICAL_SURFACE('',#20479,0.625);
#17280=CYLINDRICAL_SURFACE('',#20492,0.165);
#17281=CYLINDRICAL_SURFACE('',#20499,0.165);
#17282=CYLINDRICAL_SURFACE('',#20507,0.165);
#17283=CYLINDRICAL_SURFACE('',#20514,0.165);
#17284=CYLINDRICAL_SURFACE('',#20517,1.5);
#17285=CYLINDRICAL_SURFACE('',#20524,1.05);
#17286=CYLINDRICAL_SURFACE('',#20531,2.);
#17287=CYLINDRICAL_SURFACE('',#20533,0.625);
#17288=CYLINDRICAL_SURFACE('',#20541,0.165);
#17289=CYLINDRICAL_SURFACE('',#20548,0.165);
#17290=CYLINDRICAL_SURFACE('',#20556,0.165);
#17291=CYLINDRICAL_SURFACE('',#20563,0.165);
#17292=CYLINDRICAL_SURFACE('',#20566,1.5);
#17293=CYLINDRICAL_SURFACE('',#20573,1.05);
#17294=CYLINDRICAL_SURFACE('',#20580,2.);
#17295=CYLINDRICAL_SURFACE('',#20582,0.625);
#17296=CYLINDRICAL_SURFACE('',#20587,0.165);
#17297=CYLINDRICAL_SURFACE('',#20591,0.165);
#17298=CYLINDRICAL_SURFACE('',#20595,0.165);
#17299=CYLINDRICAL_SURFACE('',#20599,1.11);
#17300=CYLINDRICAL_SURFACE('',#20602,2.2);
#17301=CYLINDRICAL_SURFACE('',#20608,0.165);
#17302=CYLINDRICAL_SURFACE('',#20611,0.165);
#17303=CYLINDRICAL_SURFACE('',#20614,3.);
#17304=CYLINDRICAL_SURFACE('',#20620,0.225);
#17305=CYLINDRICAL_SURFACE('',#20623,0.225);
#17306=CYLINDRICAL_SURFACE('',#20651,1.05);
#17307=CYLINDRICAL_SURFACE('',#20655,1.);
#17308=CYLINDRICAL_SURFACE('',#20659,1.05);
#17309=CYLINDRICAL_SURFACE('',#20663,1.);
#17310=CYLINDRICAL_SURFACE('',#20667,1.05);
#17311=CYLINDRICAL_SURFACE('',#20671,0.9);
#17312=CYLINDRICAL_SURFACE('',#20684,0.895);
#17313=CYLINDRICAL_SURFACE('',#20688,0.605);
#17314=CYLINDRICAL_SURFACE('',#20692,0.457875);
#17315=CYLINDRICAL_SURFACE('',#20694,0.457875);
#17316=CYLINDRICAL_SURFACE('',#20695,0.457875);
#17317=CYLINDRICAL_SURFACE('',#20696,0.457875);
#17318=CYLINDRICAL_SURFACE('',#20697,0.457875);
#17319=CYLINDRICAL_SURFACE('',#20698,0.457875);
#17320=CYLINDRICAL_SURFACE('',#20699,0.457875);
#17321=CYLINDRICAL_SURFACE('',#20700,0.457875);
#17322=CYLINDRICAL_SURFACE('',#20701,0.457875);
#17323=CYLINDRICAL_SURFACE('',#20703,0.625);
#17324=CYLINDRICAL_SURFACE('',#20705,0.625);
#17325=CYLINDRICAL_SURFACE('',#20706,0.625);
#17326=CYLINDRICAL_SURFACE('',#20707,0.625);
#17327=CYLINDRICAL_SURFACE('',#20708,0.625);
#17328=CYLINDRICAL_SURFACE('',#20709,0.625);
#17329=CYLINDRICAL_SURFACE('',#20710,0.625);
#17330=CYLINDRICAL_SURFACE('',#20711,0.625);
#17331=CYLINDRICAL_SURFACE('',#20712,0.625);
#17332=CYLINDRICAL_SURFACE('',#20714,0.625);
#17333=CYLINDRICAL_SURFACE('',#20721,0.225);
#17334=CYLINDRICAL_SURFACE('',#20723,0.225);
#17335=CYLINDRICAL_SURFACE('',#20725,0.225);
#17336=CYLINDRICAL_SURFACE('',#20731,1.9);
#17337=CYLINDRICAL_SURFACE('',#20732,0.457875);
#17338=CYLINDRICAL_SURFACE('',#20733,1.1);
#17339=CYLINDRICAL_SURFACE('',#20748,0.2);
#17340=CYLINDRICAL_SURFACE('',#20755,0.35);
#17341=CYLINDRICAL_SURFACE('',#20763,0.1954);
#17342=CYLINDRICAL_SURFACE('',#20769,0.35);
#17343=CYLINDRICAL_SURFACE('',#20777,0.1954);
#17344=CYLINDRICAL_SURFACE('',#20900,0.5941);
#17345=CYLINDRICAL_SURFACE('',#20902,0.5941);
#17346=CYLINDRICAL_SURFACE('',#20903,0.5941);
#17347=CYLINDRICAL_SURFACE('',#20904,0.5941);
#17348=CYLINDRICAL_SURFACE('',#20905,0.5941);
#17349=CYLINDRICAL_SURFACE('',#20906,0.5941);
#17350=CYLINDRICAL_SURFACE('',#20907,0.5941);
#17351=CYLINDRICAL_SURFACE('',#20908,0.5941);
#17352=CYLINDRICAL_SURFACE('',#20909,0.5941);
#17353=CYLINDRICAL_SURFACE('',#20910,0.5941);
#17354=CYLINDRICAL_SURFACE('',#20911,0.5941);
#17355=CYLINDRICAL_SURFACE('',#20912,0.5941);
#17356=CYLINDRICAL_SURFACE('',#20913,0.5941);
#17357=CYLINDRICAL_SURFACE('',#20914,0.5941);
#17358=CYLINDRICAL_SURFACE('',#20915,0.5941);
#17359=CYLINDRICAL_SURFACE('',#20916,0.5941);
#17360=CYLINDRICAL_SURFACE('',#20917,0.5941);
#17361=CYLINDRICAL_SURFACE('',#20918,0.5941);
#17362=CYLINDRICAL_SURFACE('',#20919,0.5941);
#17363=CYLINDRICAL_SURFACE('',#20920,0.5941);
#17364=CYLINDRICAL_SURFACE('',#20921,0.5941);
#17365=CYLINDRICAL_SURFACE('',#20922,0.5941);
#17366=CYLINDRICAL_SURFACE('',#20923,0.5941);
#17367=CYLINDRICAL_SURFACE('',#20924,0.5941);
#17368=CYLINDRICAL_SURFACE('',#20925,0.5941);
#17369=CYLINDRICAL_SURFACE('',#20926,0.5941);
#17370=CYLINDRICAL_SURFACE('',#20927,0.5941);
#17371=CYLINDRICAL_SURFACE('',#20928,0.5941);
#17372=CYLINDRICAL_SURFACE('',#20929,0.5941);
#17373=CYLINDRICAL_SURFACE('',#20930,0.5941);
#17374=CYLINDRICAL_SURFACE('',#20931,0.5941);
#17375=CYLINDRICAL_SURFACE('',#20932,0.5941);
#17376=CYLINDRICAL_SURFACE('',#20933,0.5941);
#17377=CYLINDRICAL_SURFACE('',#20934,0.5941);
#17378=CYLINDRICAL_SURFACE('',#20935,0.5941);
#17379=CYLINDRICAL_SURFACE('',#20936,0.5941);
#17380=CYLINDRICAL_SURFACE('',#20937,0.5941);
#17381=CYLINDRICAL_SURFACE('',#20938,0.5941);
#17382=CYLINDRICAL_SURFACE('',#20939,0.5941);
#17383=CYLINDRICAL_SURFACE('',#20940,0.5941);
#17384=CYLINDRICAL_SURFACE('',#20941,0.5941);
#17385=CYLINDRICAL_SURFACE('',#20942,0.5941);
#17386=CYLINDRICAL_SURFACE('',#20943,0.5941);
#17387=CYLINDRICAL_SURFACE('',#20944,0.5941);
#17388=CYLINDRICAL_SURFACE('',#20945,0.5941);
#17389=CYLINDRICAL_SURFACE('',#20946,0.5941);
#17390=CYLINDRICAL_SURFACE('',#20947,0.5941);
#17391=CYLINDRICAL_SURFACE('',#20948,0.5941);
#17392=CYLINDRICAL_SURFACE('',#20949,0.5941);
#17393=CYLINDRICAL_SURFACE('',#20950,0.5941);
#17394=CYLINDRICAL_SURFACE('',#20951,0.5941);
#17395=CYLINDRICAL_SURFACE('',#20952,0.5941);
#17396=CYLINDRICAL_SURFACE('',#20953,0.5941);
#17397=CYLINDRICAL_SURFACE('',#20954,0.5941);
#17398=CYLINDRICAL_SURFACE('',#20955,0.5941);
#17399=CYLINDRICAL_SURFACE('',#20956,0.5941);
#17400=CYLINDRICAL_SURFACE('',#20957,0.5941);
#17401=CYLINDRICAL_SURFACE('',#20958,0.5941);
#17402=CYLINDRICAL_SURFACE('',#20959,0.5941);
#17403=CYLINDRICAL_SURFACE('',#20960,0.5941);
#17404=CYLINDRICAL_SURFACE('',#20961,0.5941);
#17405=CYLINDRICAL_SURFACE('',#20962,0.5941);
#17406=CYLINDRICAL_SURFACE('',#20963,0.5941);
#17407=CYLINDRICAL_SURFACE('',#20964,0.415875);
#17408=CYLINDRICAL_SURFACE('',#20966,0.415875);
#17409=CYLINDRICAL_SURFACE('',#20968,0.415875);
#17410=CYLINDRICAL_SURFACE('',#20969,0.415875);
#17411=CYLINDRICAL_SURFACE('',#20970,0.415875);
#17412=CYLINDRICAL_SURFACE('',#20971,0.415875);
#17413=CYLINDRICAL_SURFACE('',#20972,0.415875);
#17414=CYLINDRICAL_SURFACE('',#20973,0.415875);
#17415=CYLINDRICAL_SURFACE('',#20974,0.415875);
#17416=CYLINDRICAL_SURFACE('',#20975,0.415875);
#17417=CYLINDRICAL_SURFACE('',#20976,0.415875);
#17418=CYLINDRICAL_SURFACE('',#20977,0.415875);
#17419=CYLINDRICAL_SURFACE('',#20978,0.415875);
#17420=CYLINDRICAL_SURFACE('',#20979,0.415875);
#17421=CYLINDRICAL_SURFACE('',#20980,0.415875);
#17422=CYLINDRICAL_SURFACE('',#20981,0.415875);
#17423=CYLINDRICAL_SURFACE('',#20982,0.415875);
#17424=CYLINDRICAL_SURFACE('',#20983,0.415875);
#17425=CYLINDRICAL_SURFACE('',#20984,0.415875);
#17426=CYLINDRICAL_SURFACE('',#20985,0.415875);
#17427=CYLINDRICAL_SURFACE('',#20986,0.415875);
#17428=CYLINDRICAL_SURFACE('',#20987,0.415875);
#17429=CYLINDRICAL_SURFACE('',#20988,0.415875);
#17430=CYLINDRICAL_SURFACE('',#20989,0.415875);
#17431=CYLINDRICAL_SURFACE('',#20990,0.415875);
#17432=CYLINDRICAL_SURFACE('',#20991,0.415875);
#17433=CYLINDRICAL_SURFACE('',#20992,0.415875);
#17434=CYLINDRICAL_SURFACE('',#20993,0.415875);
#17435=CYLINDRICAL_SURFACE('',#20994,0.415875);
#17436=CYLINDRICAL_SURFACE('',#20995,0.415875);
#17437=CYLINDRICAL_SURFACE('',#20996,0.415875);
#17438=CYLINDRICAL_SURFACE('',#20997,0.415875);
#17439=CYLINDRICAL_SURFACE('',#20998,0.415875);
#17440=CYLINDRICAL_SURFACE('',#20999,0.415875);
#17441=CYLINDRICAL_SURFACE('',#21000,0.415875);
#17442=CYLINDRICAL_SURFACE('',#21001,0.415875);
#17443=CYLINDRICAL_SURFACE('',#21002,0.415875);
#17444=CYLINDRICAL_SURFACE('',#21003,0.415875);
#17445=CYLINDRICAL_SURFACE('',#21004,0.415875);
#17446=CYLINDRICAL_SURFACE('',#21005,0.415875);
#17447=CYLINDRICAL_SURFACE('',#21006,0.415875);
#17448=CYLINDRICAL_SURFACE('',#21007,0.415875);
#17449=CYLINDRICAL_SURFACE('',#21008,0.415875);
#17450=CYLINDRICAL_SURFACE('',#21009,0.415875);
#17451=CYLINDRICAL_SURFACE('',#21010,0.415875);
#17452=CYLINDRICAL_SURFACE('',#21011,0.415875);
#17453=CYLINDRICAL_SURFACE('',#21012,0.415875);
#17454=CYLINDRICAL_SURFACE('',#21013,0.415875);
#17455=CYLINDRICAL_SURFACE('',#21014,0.415875);
#17456=CYLINDRICAL_SURFACE('',#21015,0.415875);
#17457=CYLINDRICAL_SURFACE('',#21016,0.415875);
#17458=CYLINDRICAL_SURFACE('',#21017,0.415875);
#17459=CYLINDRICAL_SURFACE('',#21018,0.415875);
#17460=CYLINDRICAL_SURFACE('',#21019,0.415875);
#17461=CYLINDRICAL_SURFACE('',#21020,0.415875);
#17462=CYLINDRICAL_SURFACE('',#21021,0.415875);
#17463=CYLINDRICAL_SURFACE('',#21022,0.415875);
#17464=CYLINDRICAL_SURFACE('',#21023,0.415875);
#17465=CYLINDRICAL_SURFACE('',#21024,0.415875);
#17466=CYLINDRICAL_SURFACE('',#21025,0.415875);
#17467=CYLINDRICAL_SURFACE('',#21026,0.415875);
#17468=CYLINDRICAL_SURFACE('',#21027,0.415875);
#17469=CYLINDRICAL_SURFACE('',#21028,0.415875);
#17470=CYLINDRICAL_SURFACE('',#21032,0.6);
#17471=CYLINDRICAL_SURFACE('',#21035,0.415875);
#17472=CYLINDRICAL_SURFACE('',#21043,1.);
#17473=CYLINDRICAL_SURFACE('',#21050,1.35);
#17474=CYLINDRICAL_SURFACE('',#21053,0.5941);
#17475=CYLINDRICAL_SURFACE('',#21055,1.01);
#17476=CYLINDRICAL_SURFACE('',#21058,1.35);
#17477=CYLINDRICAL_SURFACE('',#21066,0.210000000000001);
#17478=CYLINDRICAL_SURFACE('',#21069,1.005);
#17479=CYLINDRICAL_SURFACE('',#21072,1.5);
#17480=CYLINDRICAL_SURFACE('',#21078,0.25);
#17481=CYLINDRICAL_SURFACE('',#21083,0.210000000000001);
#17482=CYLINDRICAL_SURFACE('',#21095,3.5);
#17483=CYLINDRICAL_SURFACE('',#21096,1.);
#17484=CYLINDRICAL_SURFACE('',#21098,1.5);
#17485=CYLINDRICAL_SURFACE('',#21102,0.33);
#17486=CYLINDRICAL_SURFACE('',#21105,0.4);
#17487=CYLINDRICAL_SURFACE('',#21111,0.405);
#17488=CYLINDRICAL_SURFACE('',#21114,0.9);
#17489=CYLINDRICAL_SURFACE('',#21142,0.24505);
#17490=CYLINDRICAL_SURFACE('',#21148,0.32);
#17491=CYLINDRICAL_SURFACE('',#21151,0.6);
#17492=CYLINDRICAL_SURFACE('',#21161,0.5);
#17493=CYLINDRICAL_SURFACE('',#21169,0.2942);
#17494=ADVANCED_FACE('',(#2170),#17105,.F.);
#17495=ADVANCED_FACE('',(#2171),#1589,.T.);
#17496=ADVANCED_FACE('',(#2172),#1590,.T.);
#17497=ADVANCED_FACE('',(#2173),#1591,.F.);
#17498=ADVANCED_FACE('',(#2174),#1592,.T.);
#17499=ADVANCED_FACE('',(#2175),#1593,.T.);
#17500=ADVANCED_FACE('',(#2176),#17106,.F.);
#17501=ADVANCED_FACE('',(#2177),#1594,.T.);
#17502=ADVANCED_FACE('',(#2178),#17107,.F.);
#17503=ADVANCED_FACE('',(#2179),#1595,.T.);
#17504=ADVANCED_FACE('',(#2180),#17108,.F.);
#17505=ADVANCED_FACE('',(#2181),#1596,.T.);
#17506=ADVANCED_FACE('',(#2182),#17109,.F.);
#17507=ADVANCED_FACE('',(#2183),#1597,.T.);
#17508=ADVANCED_FACE('',(#2184),#17110,.F.);
#17509=ADVANCED_FACE('',(#2185),#17111,.F.);
#17510=ADVANCED_FACE('',(#2186),#17112,.F.);
#17511=ADVANCED_FACE('',(#2187),#17113,.F.);
#17512=ADVANCED_FACE('',(#2188),#17114,.F.);
#17513=ADVANCED_FACE('',(#2189),#17115,.F.);
#17514=ADVANCED_FACE('',(#2190),#17116,.F.);
#17515=ADVANCED_FACE('',(#2191),#17117,.F.);
#17516=ADVANCED_FACE('',(#2192),#17118,.F.);
#17517=ADVANCED_FACE('',(#2193),#17119,.F.);
#17518=ADVANCED_FACE('',(#2194),#17120,.F.);
#17519=ADVANCED_FACE('',(#2195),#17121,.F.);
#17520=ADVANCED_FACE('',(#2196),#17122,.F.);
#17521=ADVANCED_FACE('',(#2197),#17123,.F.);
#17522=ADVANCED_FACE('',(#2198),#17124,.F.);
#17523=ADVANCED_FACE('',(#2199),#1598,.T.);
#17524=ADVANCED_FACE('',(#2200),#1599,.T.);
#17525=ADVANCED_FACE('',(#2201),#1600,.T.);
#17526=ADVANCED_FACE('',(#2202,#1247,#1248,#1249,#1250,#1251,#1252,#1253,
#1254,#1255,#1256,#1257,#1258,#1259,#1260,#1261,#1262,#1263,#1264,#1265,
#1266),#1601,.T.);
#17527=ADVANCED_FACE('',(#2203,#1267,#1268,#1269,#1270,#1271,#1272,#1273,
#1274,#1275,#1276,#1277,#1278,#1279,#1280,#1281,#1282),#1602,.F.);
#17528=ADVANCED_FACE('',(#2204),#1603,.T.);
#17529=ADVANCED_FACE('',(#2205),#1604,.T.);
#17530=ADVANCED_FACE('',(#2206),#1605,.T.);
#17531=ADVANCED_FACE('',(#2207),#1606,.T.);
#17532=ADVANCED_FACE('',(#2208),#1607,.T.);
#17533=ADVANCED_FACE('',(#2209),#1608,.F.);
#17534=ADVANCED_FACE('',(#2210),#1609,.T.);
#17535=ADVANCED_FACE('',(#2211),#1610,.T.);
#17536=ADVANCED_FACE('',(#2212),#1611,.T.);
#17537=ADVANCED_FACE('',(#2213),#1612,.T.);
#17538=ADVANCED_FACE('',(#2214),#1613,.T.);
#17539=ADVANCED_FACE('',(#2215),#1614,.F.);
#17540=ADVANCED_FACE('',(#2216),#17125,.F.);
#17541=ADVANCED_FACE('',(#2217),#17126,.F.);
#17542=ADVANCED_FACE('',(#2218),#17127,.F.);
#17543=ADVANCED_FACE('',(#2219),#17128,.F.);
#17544=ADVANCED_FACE('',(#2220),#17129,.F.);
#17545=ADVANCED_FACE('',(#2221),#17130,.F.);
#17546=ADVANCED_FACE('',(#2222),#17131,.F.);
#17547=ADVANCED_FACE('',(#2223),#17132,.F.);
#17548=ADVANCED_FACE('',(#2224),#1615,.F.);
#17549=ADVANCED_FACE('',(#2225),#1616,.F.);
#17550=ADVANCED_FACE('',(#2226),#1617,.F.);
#17551=ADVANCED_FACE('',(#2227),#1618,.F.);
#17552=ADVANCED_FACE('',(#2228),#17133,.F.);
#17553=ADVANCED_FACE('',(#2229),#17134,.F.);
#17554=ADVANCED_FACE('',(#2230),#1619,.T.);
#17555=ADVANCED_FACE('',(#2231),#1620,.T.);
#17556=ADVANCED_FACE('',(#2232),#1621,.T.);
#17557=ADVANCED_FACE('',(#2233),#1622,.T.);
#17558=ADVANCED_FACE('',(#2234,#1283,#1284,#1285,#1286,#1287,#1288,#1289,
#1290,#1291,#1292,#1293),#1623,.T.);
#17559=ADVANCED_FACE('',(#2235,#1294,#1295,#1296,#1297,#1298,#1299,#1300,
#1301,#1302,#1303,#1304),#1624,.F.);
#17560=ADVANCED_FACE('',(#2236),#17135,.F.);
#17561=ADVANCED_FACE('',(#2237),#17136,.F.);
#17562=ADVANCED_FACE('',(#2238),#17137,.F.);
#17563=ADVANCED_FACE('',(#2239),#1625,.T.);
#17564=ADVANCED_FACE('',(#2240),#17138,.F.);
#17565=ADVANCED_FACE('',(#2241),#1626,.T.);
#17566=ADVANCED_FACE('',(#2242),#17139,.F.);
#17567=ADVANCED_FACE('',(#2243),#1627,.F.);
#17568=ADVANCED_FACE('',(#2244),#17140,.F.);
#17569=ADVANCED_FACE('',(#2245),#1628,.F.);
#17570=ADVANCED_FACE('',(#2246),#1629,.T.);
#17571=ADVANCED_FACE('',(#2247,#1305,#1306),#1630,.T.);
#17572=ADVANCED_FACE('',(#2248),#1631,.T.);
#17573=ADVANCED_FACE('',(#2249,#1307,#1308),#1632,.T.);
#17574=ADVANCED_FACE('',(#2250,#1309,#1310),#1633,.T.);
#17575=ADVANCED_FACE('',(#2251,#1311,#1312),#1634,.F.);
#17576=ADVANCED_FACE('',(#2252),#17141,.F.);
#17577=ADVANCED_FACE('',(#2253),#17142,.F.);
#17578=ADVANCED_FACE('',(#2254),#17143,.F.);
#17579=ADVANCED_FACE('',(#2255),#1635,.T.);
#17580=ADVANCED_FACE('',(#2256),#17144,.F.);
#17581=ADVANCED_FACE('',(#2257),#1636,.T.);
#17582=ADVANCED_FACE('',(#2258),#17145,.F.);
#17583=ADVANCED_FACE('',(#2259),#1637,.F.);
#17584=ADVANCED_FACE('',(#2260),#17146,.F.);
#17585=ADVANCED_FACE('',(#2261),#1638,.F.);
#17586=ADVANCED_FACE('',(#2262),#1639,.T.);
#17587=ADVANCED_FACE('',(#2263,#1313,#1314),#1640,.T.);
#17588=ADVANCED_FACE('',(#2264),#1641,.T.);
#17589=ADVANCED_FACE('',(#2265,#1315,#1316),#1642,.T.);
#17590=ADVANCED_FACE('',(#2266,#1317,#1318),#1643,.T.);
#17591=ADVANCED_FACE('',(#2267,#1319,#1320),#1644,.F.);
#17592=ADVANCED_FACE('',(#2268),#17147,.F.);
#17593=ADVANCED_FACE('',(#2269),#1645,.F.);
#17594=ADVANCED_FACE('',(#2270),#17148,.F.);
#17595=ADVANCED_FACE('',(#2271),#1646,.F.);
#17596=ADVANCED_FACE('',(#2272),#17149,.F.);
#17597=ADVANCED_FACE('',(#2273),#17150,.F.);
#17598=ADVANCED_FACE('',(#2274,#1321,#1322),#1647,.T.);
#17599=ADVANCED_FACE('',(#2275),#1648,.T.);
#17600=ADVANCED_FACE('',(#2276,#1323,#1324),#1649,.T.);
#17601=ADVANCED_FACE('',(#2277),#1650,.T.);
#17602=ADVANCED_FACE('',(#2278),#1651,.T.);
#17603=ADVANCED_FACE('',(#2279,#1325,#1326),#1652,.F.);
#17604=ADVANCED_FACE('',(#2280),#17151,.F.);
#17605=ADVANCED_FACE('',(#2281),#17152,.F.);
#17606=ADVANCED_FACE('',(#2282),#17153,.F.);
#17607=ADVANCED_FACE('',(#2283),#1653,.F.);
#17608=ADVANCED_FACE('',(#2284),#17154,.F.);
#17609=ADVANCED_FACE('',(#2285),#1654,.F.);
#17610=ADVANCED_FACE('',(#2286),#1655,.T.);
#17611=ADVANCED_FACE('',(#2287,#1327,#1328),#1656,.T.);
#17612=ADVANCED_FACE('',(#2288),#1657,.T.);
#17613=ADVANCED_FACE('',(#2289),#1658,.T.);
#17614=ADVANCED_FACE('',(#2290,#1329,#1330),#1659,.T.);
#17615=ADVANCED_FACE('',(#2291),#1660,.T.);
#17616=ADVANCED_FACE('',(#2292,#1331,#1332),#1661,.T.);
#17617=ADVANCED_FACE('',(#2293),#1662,.F.);
#17618=ADVANCED_FACE('',(#2294),#17155,.F.);
#17619=ADVANCED_FACE('',(#2295),#1663,.F.);
#17620=ADVANCED_FACE('',(#2296),#17156,.F.);
#17621=ADVANCED_FACE('',(#2297),#1664,.F.);
#17622=ADVANCED_FACE('',(#2298),#17157,.F.);
#17623=ADVANCED_FACE('',(#2299),#17158,.F.);
#17624=ADVANCED_FACE('',(#2300,#1333,#1334),#1665,.T.);
#17625=ADVANCED_FACE('',(#2301),#1666,.T.);
#17626=ADVANCED_FACE('',(#2302,#1335,#1336),#1667,.T.);
#17627=ADVANCED_FACE('',(#2303),#1668,.T.);
#17628=ADVANCED_FACE('',(#2304),#1669,.T.);
#17629=ADVANCED_FACE('',(#2305,#1337,#1338),#1670,.F.);
#17630=ADVANCED_FACE('',(#2306),#17159,.F.);
#17631=ADVANCED_FACE('',(#2307),#17160,.F.);
#17632=ADVANCED_FACE('',(#2308),#17161,.F.);
#17633=ADVANCED_FACE('',(#2309),#1671,.F.);
#17634=ADVANCED_FACE('',(#2310),#17162,.F.);
#17635=ADVANCED_FACE('',(#2311),#1672,.F.);
#17636=ADVANCED_FACE('',(#2312),#1673,.T.);
#17637=ADVANCED_FACE('',(#2313,#1339,#1340),#1674,.T.);
#17638=ADVANCED_FACE('',(#2314),#1675,.T.);
#17639=ADVANCED_FACE('',(#2315),#1676,.T.);
#17640=ADVANCED_FACE('',(#2316,#1341,#1342),#1677,.T.);
#17641=ADVANCED_FACE('',(#2317),#1678,.T.);
#17642=ADVANCED_FACE('',(#2318,#1343,#1344),#1679,.T.);
#17643=ADVANCED_FACE('',(#2319),#1680,.F.);
#17644=ADVANCED_FACE('',(#2320),#17163,.F.);
#17645=ADVANCED_FACE('',(#2321),#17164,.F.);
#17646=ADVANCED_FACE('',(#2322),#17165,.F.);
#17647=ADVANCED_FACE('',(#2323),#17166,.F.);
#17648=ADVANCED_FACE('',(#2324),#1681,.F.);
#17649=ADVANCED_FACE('',(#2325),#17167,.F.);
#17650=ADVANCED_FACE('',(#2326),#1682,.F.);
#17651=ADVANCED_FACE('',(#2327),#17168,.F.);
#17652=ADVANCED_FACE('',(#2328),#1683,.F.);
#17653=ADVANCED_FACE('',(#2329),#17169,.F.);
#17654=ADVANCED_FACE('',(#2330),#1684,.F.);
#17655=ADVANCED_FACE('',(#2331),#17170,.F.);
#17656=ADVANCED_FACE('',(#2332,#1345),#1685,.F.);
#17657=ADVANCED_FACE('',(#2333),#17171,.F.);
#17658=ADVANCED_FACE('',(#2334),#17172,.F.);
#17659=ADVANCED_FACE('',(#2335,#1346,#1347,#1348,#1349),#1686,.F.);
#17660=ADVANCED_FACE('',(#2336),#1687,.T.);
#17661=ADVANCED_FACE('',(#2337),#1688,.T.);
#17662=ADVANCED_FACE('',(#2338),#1689,.T.);
#17663=ADVANCED_FACE('',(#2339),#1690,.T.);
#17664=ADVANCED_FACE('',(#2340,#1350,#1351,#1352,#1353),#1691,.T.);
#17665=ADVANCED_FACE('',(#2341,#1354,#1355,#1356,#1357,#1358),#1692,.F.);
#17666=ADVANCED_FACE('',(#2342),#17173,.F.);
#17667=ADVANCED_FACE('',(#2343),#17174,.F.);
#17668=ADVANCED_FACE('',(#2344),#17175,.F.);
#17669=ADVANCED_FACE('',(#2345),#17176,.F.);
#17670=ADVANCED_FACE('',(#2346),#17177,.F.);
#17671=ADVANCED_FACE('',(#2347),#17178,.F.);
#17672=ADVANCED_FACE('',(#2348),#1693,.T.);
#17673=ADVANCED_FACE('',(#2349),#17179,.F.);
#17674=ADVANCED_FACE('',(#2350),#1694,.T.);
#17675=ADVANCED_FACE('',(#2351),#17180,.F.);
#17676=ADVANCED_FACE('',(#2352),#1695,.F.);
#17677=ADVANCED_FACE('',(#2353),#17181,.F.);
#17678=ADVANCED_FACE('',(#2354),#1696,.F.);
#17679=ADVANCED_FACE('',(#2355),#17182,.F.);
#17680=ADVANCED_FACE('',(#2356,#1359),#1697,.T.);
#17681=ADVANCED_FACE('',(#2357),#17183,.F.);
#17682=ADVANCED_FACE('',(#2358),#17184,.F.);
#17683=ADVANCED_FACE('',(#2359),#17185,.F.);
#17684=ADVANCED_FACE('',(#2360,#1360,#1361),#1698,.T.);
#17685=ADVANCED_FACE('',(#2361,#1362,#1363,#1364,#1365,#1366,#1367),#1699,
 .F.);
#17686=ADVANCED_FACE('',(#2362),#1700,.T.);
#17687=ADVANCED_FACE('',(#2363),#1701,.T.);
#17688=ADVANCED_FACE('',(#2364,#1368,#1369),#1702,.T.);
#17689=ADVANCED_FACE('',(#2365,#1370,#1371,#1372,#1373,#1374,#1375),#1703,
 .T.);
#17690=ADVANCED_FACE('',(#2366),#17186,.F.);
#17691=ADVANCED_FACE('',(#2367),#17187,.F.);
#17692=ADVANCED_FACE('',(#2368),#17188,.F.);
#17693=ADVANCED_FACE('',(#2369),#17189,.T.);
#17694=ADVANCED_FACE('',(#2370,#1376),#1704,.T.);
#17695=ADVANCED_FACE('',(#2371),#17190,.F.);
#17696=ADVANCED_FACE('',(#2372),#17191,.T.);
#17697=ADVANCED_FACE('',(#2373,#1377,#1378,#1379,#1380),#1705,.T.);
#17698=ADVANCED_FACE('',(#2374,#1381,#1382,#1383,#1384),#1706,.F.);
#17699=ADVANCED_FACE('',(#2375),#17192,.F.);
#17700=ADVANCED_FACE('',(#2376),#17193,.F.);
#17701=ADVANCED_FACE('',(#2377),#17194,.F.);
#17702=ADVANCED_FACE('',(#2378),#17195,.T.);
#17703=ADVANCED_FACE('',(#2379,#1385),#1707,.F.);
#17704=ADVANCED_FACE('',(#2380),#17196,.F.);
#17705=ADVANCED_FACE('',(#2381),#17197,.T.);
#17706=ADVANCED_FACE('',(#2382,#1386,#1387,#1388,#1389),#1708,.T.);
#17707=ADVANCED_FACE('',(#2383,#1390,#1391,#1392,#1393),#1709,.F.);
#17708=ADVANCED_FACE('',(#2384),#17198,.F.);
#17709=ADVANCED_FACE('',(#2385),#1710,.F.);
#17710=ADVANCED_FACE('',(#2386),#17199,.T.);
#17711=ADVANCED_FACE('',(#2387),#1711,.T.);
#17712=ADVANCED_FACE('',(#2388,#1394),#1712,.F.);
#17713=ADVANCED_FACE('',(#2389),#17200,.F.);
#17714=ADVANCED_FACE('',(#2390),#1713,.T.);
#17715=ADVANCED_FACE('',(#2391),#17201,.T.);
#17716=ADVANCED_FACE('',(#2392,#1395),#1714,.T.);
#17717=ADVANCED_FACE('',(#2393),#1715,.F.);
#17718=ADVANCED_FACE('',(#2394),#17202,.F.);
#17719=ADVANCED_FACE('',(#2395),#1716,.F.);
#17720=ADVANCED_FACE('',(#2396),#17203,.T.);
#17721=ADVANCED_FACE('',(#2397),#1717,.T.);
#17722=ADVANCED_FACE('',(#2398,#1396),#1718,.F.);
#17723=ADVANCED_FACE('',(#2399),#17204,.F.);
#17724=ADVANCED_FACE('',(#2400),#1719,.T.);
#17725=ADVANCED_FACE('',(#2401),#17205,.T.);
#17726=ADVANCED_FACE('',(#2402,#1397),#1720,.T.);
#17727=ADVANCED_FACE('',(#2403),#1721,.F.);
#17728=ADVANCED_FACE('',(#2404),#17206,.F.);
#17729=ADVANCED_FACE('',(#2405,#1398),#1722,.T.);
#17730=ADVANCED_FACE('',(#2406),#17207,.F.);
#17731=ADVANCED_FACE('',(#2407,#1399),#1723,.T.);
#17732=ADVANCED_FACE('',(#2408),#17208,.F.);
#17733=ADVANCED_FACE('',(#2409,#1400),#1724,.T.);
#17734=ADVANCED_FACE('',(#2410),#17209,.F.);
#17735=ADVANCED_FACE('',(#2411,#1401),#1725,.T.);
#17736=ADVANCED_FACE('',(#2412),#17210,.F.);
#17737=ADVANCED_FACE('',(#2413),#17211,.F.);
#17738=ADVANCED_FACE('',(#2414),#17212,.F.);
#17739=ADVANCED_FACE('',(#2415),#17213,.F.);
#17740=ADVANCED_FACE('',(#2416),#17214,.T.);
#17741=ADVANCED_FACE('',(#2417,#1402,#1403,#1404,#1405),#1726,.T.);
#17742=ADVANCED_FACE('',(#2418,#1406,#1407,#1408,#1409),#1727,.F.);
#17743=ADVANCED_FACE('',(#2419),#1728,.F.);
#17744=ADVANCED_FACE('',(#2420),#1729,.F.);
#17745=ADVANCED_FACE('',(#2421),#1730,.F.);
#17746=ADVANCED_FACE('',(#2422),#1731,.F.);
#17747=ADVANCED_FACE('',(#2423),#1732,.F.);
#17748=ADVANCED_FACE('',(#2424),#1733,.F.);
#17749=ADVANCED_FACE('',(#2425),#1734,.F.);
#17750=ADVANCED_FACE('',(#2426),#1735,.F.);
#17751=ADVANCED_FACE('',(#2427),#1736,.F.);
#17752=ADVANCED_FACE('',(#2428),#1737,.F.);
#17753=ADVANCED_FACE('',(#2429),#1738,.F.);
#17754=ADVANCED_FACE('',(#2430),#1739,.F.);
#17755=ADVANCED_FACE('',(#2431),#1740,.F.);
#17756=ADVANCED_FACE('',(#2432),#1741,.F.);
#17757=ADVANCED_FACE('',(#2433),#1742,.F.);
#17758=ADVANCED_FACE('',(#2434),#1743,.F.);
#17759=ADVANCED_FACE('',(#2435),#1744,.F.);
#17760=ADVANCED_FACE('',(#2436),#1745,.F.);
#17761=ADVANCED_FACE('',(#2437),#1746,.F.);
#17762=ADVANCED_FACE('',(#2438),#1747,.F.);
#17763=ADVANCED_FACE('',(#2439),#1748,.F.);
#17764=ADVANCED_FACE('',(#2440),#1749,.F.);
#17765=ADVANCED_FACE('',(#2441),#1750,.F.);
#17766=ADVANCED_FACE('',(#2442),#1751,.F.);
#17767=ADVANCED_FACE('',(#2443),#1752,.F.);
#17768=ADVANCED_FACE('',(#2444),#1753,.F.);
#17769=ADVANCED_FACE('',(#2445),#1754,.F.);
#17770=ADVANCED_FACE('',(#2446),#1755,.F.);
#17771=ADVANCED_FACE('',(#2447),#1756,.F.);
#17772=ADVANCED_FACE('',(#2448),#1757,.F.);
#17773=ADVANCED_FACE('',(#2449),#1758,.F.);
#17774=ADVANCED_FACE('',(#2450),#1759,.F.);
#17775=ADVANCED_FACE('',(#2451),#1760,.F.);
#17776=ADVANCED_FACE('',(#2452),#1761,.F.);
#17777=ADVANCED_FACE('',(#2453),#1762,.F.);
#17778=ADVANCED_FACE('',(#2454),#1763,.F.);
#17779=ADVANCED_FACE('',(#2455),#1764,.F.);
#17780=ADVANCED_FACE('',(#2456),#1765,.F.);
#17781=ADVANCED_FACE('',(#2457),#1766,.F.);
#17782=ADVANCED_FACE('',(#2458),#1767,.F.);
#17783=ADVANCED_FACE('',(#2459),#1768,.F.);
#17784=ADVANCED_FACE('',(#2460),#1769,.F.);
#17785=ADVANCED_FACE('',(#2461),#1770,.F.);
#17786=ADVANCED_FACE('',(#2462),#1771,.F.);
#17787=ADVANCED_FACE('',(#2463),#1772,.F.);
#17788=ADVANCED_FACE('',(#2464),#1773,.F.);
#17789=ADVANCED_FACE('',(#2465),#1774,.F.);
#17790=ADVANCED_FACE('',(#2466),#1775,.F.);
#17791=ADVANCED_FACE('',(#2467),#1776,.F.);
#17792=ADVANCED_FACE('',(#2468),#1777,.F.);
#17793=ADVANCED_FACE('',(#2469),#1778,.F.);
#17794=ADVANCED_FACE('',(#2470),#1779,.F.);
#17795=ADVANCED_FACE('',(#2471),#1780,.F.);
#17796=ADVANCED_FACE('',(#2472),#1781,.F.);
#17797=ADVANCED_FACE('',(#2473),#1782,.F.);
#17798=ADVANCED_FACE('',(#2474),#1783,.F.);
#17799=ADVANCED_FACE('',(#2475),#1784,.F.);
#17800=ADVANCED_FACE('',(#2476),#1785,.F.);
#17801=ADVANCED_FACE('',(#2477),#1786,.F.);
#17802=ADVANCED_FACE('',(#2478),#1787,.F.);
#17803=ADVANCED_FACE('',(#2479),#1788,.F.);
#17804=ADVANCED_FACE('',(#2480),#1789,.F.);
#17805=ADVANCED_FACE('',(#2481),#1790,.F.);
#17806=ADVANCED_FACE('',(#2482),#1791,.F.);
#17807=ADVANCED_FACE('',(#2483),#1792,.F.);
#17808=ADVANCED_FACE('',(#2484),#1793,.F.);
#17809=ADVANCED_FACE('',(#2485),#1794,.F.);
#17810=ADVANCED_FACE('',(#2486),#1795,.F.);
#17811=ADVANCED_FACE('',(#2487),#1796,.F.);
#17812=ADVANCED_FACE('',(#2488),#1797,.F.);
#17813=ADVANCED_FACE('',(#2489),#1798,.F.);
#17814=ADVANCED_FACE('',(#2490),#1799,.F.);
#17815=ADVANCED_FACE('',(#2491),#1800,.F.);
#17816=ADVANCED_FACE('',(#2492),#1801,.F.);
#17817=ADVANCED_FACE('',(#2493),#1802,.F.);
#17818=ADVANCED_FACE('',(#2494),#1803,.F.);
#17819=ADVANCED_FACE('',(#2495),#1804,.F.);
#17820=ADVANCED_FACE('',(#2496),#1805,.F.);
#17821=ADVANCED_FACE('',(#2497),#1806,.F.);
#17822=ADVANCED_FACE('',(#2498),#1807,.F.);
#17823=ADVANCED_FACE('',(#2499),#1808,.F.);
#17824=ADVANCED_FACE('',(#2500),#1809,.F.);
#17825=ADVANCED_FACE('',(#2501),#1810,.F.);
#17826=ADVANCED_FACE('',(#2502),#1811,.F.);
#17827=ADVANCED_FACE('',(#2503),#1812,.F.);
#17828=ADVANCED_FACE('',(#2504),#1813,.F.);
#17829=ADVANCED_FACE('',(#2505),#1814,.F.);
#17830=ADVANCED_FACE('',(#2506),#1815,.F.);
#17831=ADVANCED_FACE('',(#2507),#1816,.F.);
#17832=ADVANCED_FACE('',(#2508),#1817,.F.);
#17833=ADVANCED_FACE('',(#2509),#1818,.F.);
#17834=ADVANCED_FACE('',(#2510),#1819,.F.);
#17835=ADVANCED_FACE('',(#2511),#1820,.F.);
#17836=ADVANCED_FACE('',(#2512),#1821,.F.);
#17837=ADVANCED_FACE('',(#2513),#1822,.F.);
#17838=ADVANCED_FACE('',(#2514),#1823,.F.);
#17839=ADVANCED_FACE('',(#2515),#1824,.F.);
#17840=ADVANCED_FACE('',(#2516),#1825,.F.);
#17841=ADVANCED_FACE('',(#2517),#1826,.F.);
#17842=ADVANCED_FACE('',(#2518),#1827,.F.);
#17843=ADVANCED_FACE('',(#2519),#1828,.F.);
#17844=ADVANCED_FACE('',(#2520),#1829,.F.);
#17845=ADVANCED_FACE('',(#2521),#1830,.F.);
#17846=ADVANCED_FACE('',(#2522),#1831,.F.);
#17847=ADVANCED_FACE('',(#2523),#1832,.F.);
#17848=ADVANCED_FACE('',(#2524),#1833,.F.);
#17849=ADVANCED_FACE('',(#2525),#1834,.F.);
#17850=ADVANCED_FACE('',(#2526),#1835,.F.);
#17851=ADVANCED_FACE('',(#2527),#1836,.F.);
#17852=ADVANCED_FACE('',(#2528),#1837,.F.);
#17853=ADVANCED_FACE('',(#2529),#1838,.F.);
#17854=ADVANCED_FACE('',(#2530),#1839,.F.);
#17855=ADVANCED_FACE('',(#2531),#1840,.F.);
#17856=ADVANCED_FACE('',(#2532),#1841,.F.);
#17857=ADVANCED_FACE('',(#2533),#1842,.F.);
#17858=ADVANCED_FACE('',(#2534),#1843,.F.);
#17859=ADVANCED_FACE('',(#2535),#1844,.F.);
#17860=ADVANCED_FACE('',(#2536),#1845,.F.);
#17861=ADVANCED_FACE('',(#2537),#1846,.F.);
#17862=ADVANCED_FACE('',(#2538),#1847,.F.);
#17863=ADVANCED_FACE('',(#2539),#1848,.F.);
#17864=ADVANCED_FACE('',(#2540),#1849,.F.);
#17865=ADVANCED_FACE('',(#2541),#1850,.F.);
#17866=ADVANCED_FACE('',(#2542),#1851,.F.);
#17867=ADVANCED_FACE('',(#2543),#1852,.F.);
#17868=ADVANCED_FACE('',(#2544),#17215,.F.);
#17869=ADVANCED_FACE('',(#2545),#17216,.F.);
#17870=ADVANCED_FACE('',(#2546),#1853,.T.);
#17871=ADVANCED_FACE('',(#2547,#1410,#1411),#1854,.T.);
#17872=ADVANCED_FACE('',(#2548),#1855,.T.);
#17873=ADVANCED_FACE('',(#2549,#1412,#1413,#1414,#1415,#1416,#1417,#1418,
#1419,#1420,#1421,#1422,#1423,#1424,#1425,#1426,#1427,#1428,#1429,#1430,
#1431,#1432,#1433,#1434,#1435,#1436,#1437,#1438),#1856,.T.);
#17874=ADVANCED_FACE('',(#2550),#1857,.T.);
#17875=ADVANCED_FACE('',(#2551),#1858,.F.);
#17876=ADVANCED_FACE('',(#2552),#945,.T.);
#17877=ADVANCED_FACE('',(#2553),#17217,.T.);
#17878=ADVANCED_FACE('',(#2554),#1859,.F.);
#17879=ADVANCED_FACE('',(#2555),#946,.T.);
#17880=ADVANCED_FACE('',(#2556),#1860,.T.);
#17881=ADVANCED_FACE('',(#2557),#1861,.F.);
#17882=ADVANCED_FACE('',(#2558),#17218,.F.);
#17883=ADVANCED_FACE('',(#2559),#17219,.F.);
#17884=ADVANCED_FACE('',(#2560),#1862,.F.);
#17885=ADVANCED_FACE('',(#2561,#1439),#1863,.T.);
#17886=ADVANCED_FACE('',(#2562,#1440),#1864,.T.);
#17887=ADVANCED_FACE('',(#2563,#1441),#1865,.T.);
#17888=ADVANCED_FACE('',(#2564),#17220,.F.);
#17889=ADVANCED_FACE('',(#2565),#17221,.F.);
#17890=ADVANCED_FACE('',(#2566),#17222,.F.);
#17891=ADVANCED_FACE('',(#2567),#17223,.F.);
#17892=ADVANCED_FACE('',(#2568),#17224,.F.);
#17893=ADVANCED_FACE('',(#2569,#1442),#1866,.T.);
#17894=ADVANCED_FACE('',(#2570),#1867,.T.);
#17895=ADVANCED_FACE('',(#2571,#1443,#1444),#1868,.T.);
#17896=ADVANCED_FACE('',(#2572),#1869,.T.);
#17897=ADVANCED_FACE('',(#2573,#1445),#1870,.T.);
#17898=ADVANCED_FACE('',(#2574),#1871,.T.);
#17899=ADVANCED_FACE('',(#2575,#1446),#1872,.T.);
#17900=ADVANCED_FACE('',(#2576),#1873,.T.);
#17901=ADVANCED_FACE('',(#2577,#1447),#1874,.T.);
#17902=ADVANCED_FACE('',(#2578),#1875,.T.);
#17903=ADVANCED_FACE('',(#2579,#1448),#1876,.T.);
#17904=ADVANCED_FACE('',(#2580),#1877,.F.);
#17905=ADVANCED_FACE('',(#2581),#1878,.F.);
#17906=ADVANCED_FACE('',(#2582),#1879,.F.);
#17907=ADVANCED_FACE('',(#2583),#1880,.F.);
#17908=ADVANCED_FACE('',(#2584),#1881,.F.);
#17909=ADVANCED_FACE('',(#2585),#1882,.F.);
#17910=ADVANCED_FACE('',(#2586),#1883,.F.);
#17911=ADVANCED_FACE('',(#2587),#1884,.F.);
#17912=ADVANCED_FACE('',(#2588),#1885,.F.);
#17913=ADVANCED_FACE('',(#2589),#1886,.T.);
#17914=ADVANCED_FACE('',(#2590),#947,.T.);
#17915=ADVANCED_FACE('',(#2591),#17225,.T.);
#17916=ADVANCED_FACE('',(#2592),#948,.T.);
#17917=ADVANCED_FACE('',(#2593,#1449),#1887,.T.);
#17918=ADVANCED_FACE('',(#2594),#949,.T.);
#17919=ADVANCED_FACE('',(#2595),#17226,.T.);
#17920=ADVANCED_FACE('',(#2596),#927,.F.);
#17921=ADVANCED_FACE('',(#2597),#17227,.T.);
#17922=ADVANCED_FACE('',(#2598),#17228,.F.);
#17923=ADVANCED_FACE('',(#2599),#950,.F.);
#17924=ADVANCED_FACE('',(#2600,#1450),#1888,.T.);
#17925=ADVANCED_FACE('',(#2601),#17229,.T.);
#17926=ADVANCED_FACE('',(#2602,#1451),#1889,.T.);
#17927=ADVANCED_FACE('',(#2603),#951,.F.);
#17928=ADVANCED_FACE('',(#2604),#928,.F.);
#17929=ADVANCED_FACE('',(#2605),#17230,.F.);
#17930=ADVANCED_FACE('',(#2606,#1452),#1890,.T.);
#17931=ADVANCED_FACE('',(#2607),#952,.T.);
#17932=ADVANCED_FACE('',(#2608),#17231,.T.);
#17933=ADVANCED_FACE('',(#2609),#953,.T.);
#17934=ADVANCED_FACE('',(#2610,#1453),#1891,.T.);
#17935=ADVANCED_FACE('',(#2611),#17232,.F.);
#17936=ADVANCED_FACE('',(#2612),#897,.T.);
#17937=ADVANCED_FACE('',(#2613),#898,.T.);
#17938=ADVANCED_FACE('',(#2614),#899,.T.);
#17939=ADVANCED_FACE('',(#2615),#900,.T.);
#17940=ADVANCED_FACE('',(#2616),#901,.T.);
#17941=ADVANCED_FACE('',(#2617),#902,.T.);
#17942=ADVANCED_FACE('',(#2618),#903,.T.);
#17943=ADVANCED_FACE('',(#2619),#904,.F.);
#17944=ADVANCED_FACE('',(#2620),#17233,.T.);
#17945=ADVANCED_FACE('',(#2621),#1892,.T.);
#17946=ADVANCED_FACE('',(#2622),#905,.F.);
#17947=ADVANCED_FACE('',(#2623),#1893,.T.);
#17948=ADVANCED_FACE('',(#2624),#906,.F.);
#17949=ADVANCED_FACE('',(#2625),#1894,.T.);
#17950=ADVANCED_FACE('',(#2626),#907,.F.);
#17951=ADVANCED_FACE('',(#2627),#1895,.T.);
#17952=ADVANCED_FACE('',(#2628),#908,.F.);
#17953=ADVANCED_FACE('',(#2629),#1896,.T.);
#17954=ADVANCED_FACE('',(#2630),#909,.F.);
#17955=ADVANCED_FACE('',(#2631),#17234,.F.);
#17956=ADVANCED_FACE('',(#2632),#1897,.T.);
#17957=ADVANCED_FACE('',(#2633),#910,.F.);
#17958=ADVANCED_FACE('',(#2634,#1454),#1898,.T.);
#17959=ADVANCED_FACE('',(#2635),#1899,.T.);
#17960=ADVANCED_FACE('',(#2636,#1455),#1900,.T.);
#17961=ADVANCED_FACE('',(#2637),#17235,.T.);
#17962=ADVANCED_FACE('',(#2638,#1456),#1901,.T.);
#17963=ADVANCED_FACE('',(#2639),#17236,.F.);
#17964=ADVANCED_FACE('',(#2640,#1457),#1902,.T.);
#17965=ADVANCED_FACE('',(#2641),#17237,.T.);
#17966=ADVANCED_FACE('',(#2642,#1458),#1903,.T.);
#17967=ADVANCED_FACE('',(#2643),#17238,.F.);
#17968=ADVANCED_FACE('',(#2644),#929,.F.);
#17969=ADVANCED_FACE('',(#2645),#17239,.T.);
#17970=ADVANCED_FACE('',(#2646),#17240,.F.);
#17971=ADVANCED_FACE('',(#2647),#954,.F.);
#17972=ADVANCED_FACE('',(#2648,#1459),#1904,.T.);
#17973=ADVANCED_FACE('',(#2649),#17241,.T.);
#17974=ADVANCED_FACE('',(#2650,#1460),#1905,.T.);
#17975=ADVANCED_FACE('',(#2651),#955,.F.);
#17976=ADVANCED_FACE('',(#2652),#930,.F.);
#17977=ADVANCED_FACE('',(#2653),#17242,.F.);
#17978=ADVANCED_FACE('',(#2654,#1461),#1906,.T.);
#17979=ADVANCED_FACE('',(#2655),#956,.T.);
#17980=ADVANCED_FACE('',(#2656),#17243,.T.);
#17981=ADVANCED_FACE('',(#2657),#957,.T.);
#17982=ADVANCED_FACE('',(#2658,#1462),#1907,.T.);
#17983=ADVANCED_FACE('',(#2659),#17244,.F.);
#17984=ADVANCED_FACE('',(#2660),#911,.T.);
#17985=ADVANCED_FACE('',(#2661),#912,.T.);
#17986=ADVANCED_FACE('',(#2662),#913,.T.);
#17987=ADVANCED_FACE('',(#2663),#914,.T.);
#17988=ADVANCED_FACE('',(#2664),#915,.T.);
#17989=ADVANCED_FACE('',(#2665),#916,.T.);
#17990=ADVANCED_FACE('',(#2666),#917,.T.);
#17991=ADVANCED_FACE('',(#2667),#918,.T.);
#17992=ADVANCED_FACE('',(#2668),#919,.F.);
#17993=ADVANCED_FACE('',(#2669),#17245,.T.);
#17994=ADVANCED_FACE('',(#2670),#1908,.T.);
#17995=ADVANCED_FACE('',(#2671),#920,.F.);
#17996=ADVANCED_FACE('',(#2672),#1909,.T.);
#17997=ADVANCED_FACE('',(#2673),#921,.F.);
#17998=ADVANCED_FACE('',(#2674),#1910,.T.);
#17999=ADVANCED_FACE('',(#2675),#922,.F.);
#18000=ADVANCED_FACE('',(#2676),#1911,.T.);
#18001=ADVANCED_FACE('',(#2677),#923,.F.);
#18002=ADVANCED_FACE('',(#2678),#1912,.T.);
#18003=ADVANCED_FACE('',(#2679),#924,.F.);
#18004=ADVANCED_FACE('',(#2680),#1913,.T.);
#18005=ADVANCED_FACE('',(#2681),#925,.F.);
#18006=ADVANCED_FACE('',(#2682),#17246,.F.);
#18007=ADVANCED_FACE('',(#2683),#1914,.T.);
#18008=ADVANCED_FACE('',(#2684),#926,.F.);
#18009=ADVANCED_FACE('',(#2685,#1463),#1915,.T.);
#18010=ADVANCED_FACE('',(#2686),#1916,.T.);
#18011=ADVANCED_FACE('',(#2687,#1464),#1917,.T.);
#18012=ADVANCED_FACE('',(#2688),#17247,.T.);
#18013=ADVANCED_FACE('',(#2689,#1465),#1918,.T.);
#18014=ADVANCED_FACE('',(#2690),#17248,.F.);
#18015=ADVANCED_FACE('',(#2691,#1466),#1919,.T.);
#18016=ADVANCED_FACE('',(#2692),#17249,.T.);
#18017=ADVANCED_FACE('',(#2693,#1467),#1920,.T.);
#18018=ADVANCED_FACE('',(#2694),#17250,.F.);
#18019=ADVANCED_FACE('',(#2695),#1921,.F.);
#18020=ADVANCED_FACE('',(#2696,#1468),#1922,.T.);
#18021=ADVANCED_FACE('',(#2697),#17251,.T.);
#18022=ADVANCED_FACE('',(#2698),#1923,.T.);
#18023=ADVANCED_FACE('',(#2699),#958,.T.);
#18024=ADVANCED_FACE('',(#2700),#17252,.T.);
#18025=ADVANCED_FACE('',(#2701),#959,.T.);
#18026=ADVANCED_FACE('',(#2702,#1469),#1924,.T.);
#18027=ADVANCED_FACE('',(#2703),#960,.T.);
#18028=ADVANCED_FACE('',(#2704),#17253,.T.);
#18029=ADVANCED_FACE('',(#2705),#1925,.F.);
#18030=ADVANCED_FACE('',(#2706),#1926,.F.);
#18031=ADVANCED_FACE('',(#2707),#1927,.F.);
#18032=ADVANCED_FACE('',(#2708),#1928,.F.);
#18033=ADVANCED_FACE('',(#2709),#1929,.F.);
#18034=ADVANCED_FACE('',(#2710),#1930,.F.);
#18035=ADVANCED_FACE('',(#2711),#1931,.F.);
#18036=ADVANCED_FACE('',(#2712),#1932,.F.);
#18037=ADVANCED_FACE('',(#2713),#1933,.F.);
#18038=ADVANCED_FACE('',(#2714),#1934,.F.);
#18039=ADVANCED_FACE('',(#2715),#1935,.F.);
#18040=ADVANCED_FACE('',(#2716),#1936,.F.);
#18041=ADVANCED_FACE('',(#2717),#1937,.F.);
#18042=ADVANCED_FACE('',(#2718),#1938,.F.);
#18043=ADVANCED_FACE('',(#2719),#1939,.F.);
#18044=ADVANCED_FACE('',(#2720),#1940,.F.);
#18045=ADVANCED_FACE('',(#2721),#1941,.F.);
#18046=ADVANCED_FACE('',(#2722),#1942,.T.);
#18047=ADVANCED_FACE('',(#2723),#961,.T.);
#18048=ADVANCED_FACE('',(#2724),#17254,.T.);
#18049=ADVANCED_FACE('',(#2725),#962,.T.);
#18050=ADVANCED_FACE('',(#2726,#1470),#1943,.T.);
#18051=ADVANCED_FACE('',(#2727),#963,.T.);
#18052=ADVANCED_FACE('',(#2728),#17255,.T.);
#18053=ADVANCED_FACE('',(#2729),#1944,.F.);
#18054=ADVANCED_FACE('',(#2730),#1945,.F.);
#18055=ADVANCED_FACE('',(#2731),#1946,.F.);
#18056=ADVANCED_FACE('',(#2732),#1947,.F.);
#18057=ADVANCED_FACE('',(#2733),#1948,.F.);
#18058=ADVANCED_FACE('',(#2734),#1949,.F.);
#18059=ADVANCED_FACE('',(#2735),#1950,.F.);
#18060=ADVANCED_FACE('',(#2736),#1951,.F.);
#18061=ADVANCED_FACE('',(#2737),#1952,.F.);
#18062=ADVANCED_FACE('',(#2738),#1953,.F.);
#18063=ADVANCED_FACE('',(#2739),#1954,.F.);
#18064=ADVANCED_FACE('',(#2740),#1955,.F.);
#18065=ADVANCED_FACE('',(#2741),#1956,.F.);
#18066=ADVANCED_FACE('',(#2742),#1957,.F.);
#18067=ADVANCED_FACE('',(#2743),#1958,.F.);
#18068=ADVANCED_FACE('',(#2744),#1959,.F.);
#18069=ADVANCED_FACE('',(#2745),#1960,.F.);
#18070=ADVANCED_FACE('',(#2746),#1961,.F.);
#18071=ADVANCED_FACE('',(#2747),#1962,.F.);
#18072=ADVANCED_FACE('',(#2748),#1963,.F.);
#18073=ADVANCED_FACE('',(#2749),#1964,.F.);
#18074=ADVANCED_FACE('',(#2750),#1965,.F.);
#18075=ADVANCED_FACE('',(#2751),#1966,.F.);
#18076=ADVANCED_FACE('',(#2752),#1967,.F.);
#18077=ADVANCED_FACE('',(#2753),#1968,.F.);
#18078=ADVANCED_FACE('',(#2754),#1969,.F.);
#18079=ADVANCED_FACE('',(#2755),#1970,.F.);
#18080=ADVANCED_FACE('',(#2756),#1971,.F.);
#18081=ADVANCED_FACE('',(#2757),#1972,.F.);
#18082=ADVANCED_FACE('',(#2758),#1973,.F.);
#18083=ADVANCED_FACE('',(#2759),#1974,.F.);
#18084=ADVANCED_FACE('',(#2760),#1975,.F.);
#18085=ADVANCED_FACE('',(#2761),#1976,.F.);
#18086=ADVANCED_FACE('',(#2762),#1977,.F.);
#18087=ADVANCED_FACE('',(#2763),#1978,.F.);
#18088=ADVANCED_FACE('',(#2764),#1979,.F.);
#18089=ADVANCED_FACE('',(#2765),#17256,.F.);
#18090=ADVANCED_FACE('',(#2766),#1980,.T.);
#18091=ADVANCED_FACE('',(#2767),#1981,.T.);
#18092=ADVANCED_FACE('',(#2768),#1982,.T.);
#18093=ADVANCED_FACE('',(#2769),#1983,.T.);
#18094=ADVANCED_FACE('',(#2770),#1984,.T.);
#18095=ADVANCED_FACE('',(#2771),#1985,.T.);
#18096=ADVANCED_FACE('',(#2772),#1986,.T.);
#18097=ADVANCED_FACE('',(#2773),#1987,.T.);
#18098=ADVANCED_FACE('',(#2774,#1471),#1988,.T.);
#18099=ADVANCED_FACE('',(#2775,#1472),#1989,.F.);
#18100=ADVANCED_FACE('',(#2776),#1990,.T.);
#18101=ADVANCED_FACE('',(#2777),#964,.T.);
#18102=ADVANCED_FACE('',(#2778),#17257,.T.);
#18103=ADVANCED_FACE('',(#2779),#965,.T.);
#18104=ADVANCED_FACE('',(#2780,#1473),#1991,.T.);
#18105=ADVANCED_FACE('',(#2781),#966,.T.);
#18106=ADVANCED_FACE('',(#2782),#17258,.T.);
#18107=ADVANCED_FACE('',(#2783),#967,.T.);
#18108=ADVANCED_FACE('',(#2784),#1992,.T.);
#18109=ADVANCED_FACE('',(#2785),#1993,.F.);
#18110=ADVANCED_FACE('',(#2786),#1994,.F.);
#18111=ADVANCED_FACE('',(#2787),#1995,.F.);
#18112=ADVANCED_FACE('',(#2788),#1996,.F.);
#18113=ADVANCED_FACE('',(#2789),#1997,.F.);
#18114=ADVANCED_FACE('',(#2790),#1998,.F.);
#18115=ADVANCED_FACE('',(#2791),#1999,.F.);
#18116=ADVANCED_FACE('',(#2792),#2000,.F.);
#18117=ADVANCED_FACE('',(#2793),#2001,.F.);
#18118=ADVANCED_FACE('',(#2794),#2002,.T.);
#18119=ADVANCED_FACE('',(#2795,#1474),#2003,.T.);
#18120=ADVANCED_FACE('',(#2796),#2004,.T.);
#18121=ADVANCED_FACE('',(#2797),#2005,.T.);
#18122=ADVANCED_FACE('',(#2798),#2006,.F.);
#18123=ADVANCED_FACE('',(#2799),#2007,.T.);
#18124=ADVANCED_FACE('',(#2800),#2008,.T.);
#18125=ADVANCED_FACE('',(#2801),#2009,.T.);
#18126=ADVANCED_FACE('',(#2802),#17259,.F.);
#18127=ADVANCED_FACE('',(#2803),#2010,.F.);
#18128=ADVANCED_FACE('',(#2804),#2011,.F.);
#18129=ADVANCED_FACE('',(#2805),#2012,.T.);
#18130=ADVANCED_FACE('',(#2806),#2013,.T.);
#18131=ADVANCED_FACE('',(#2807,#1475),#2014,.F.);
#18132=ADVANCED_FACE('',(#2808),#2015,.T.);
#18133=ADVANCED_FACE('',(#2809),#968,.T.);
#18134=ADVANCED_FACE('',(#2810),#17260,.T.);
#18135=ADVANCED_FACE('',(#2811),#969,.T.);
#18136=ADVANCED_FACE('',(#2812,#1476),#2016,.T.);
#18137=ADVANCED_FACE('',(#2813),#970,.T.);
#18138=ADVANCED_FACE('',(#2814),#17261,.T.);
#18139=ADVANCED_FACE('',(#2815),#2017,.F.);
#18140=ADVANCED_FACE('',(#2816),#2018,.F.);
#18141=ADVANCED_FACE('',(#2817),#2019,.F.);
#18142=ADVANCED_FACE('',(#2818),#2020,.F.);
#18143=ADVANCED_FACE('',(#2819),#2021,.F.);
#18144=ADVANCED_FACE('',(#2820),#2022,.F.);
#18145=ADVANCED_FACE('',(#2821),#2023,.F.);
#18146=ADVANCED_FACE('',(#2822),#17262,.F.);
#18147=ADVANCED_FACE('',(#2823),#17263,.F.);
#18148=ADVANCED_FACE('',(#2824),#17264,.F.);
#18149=ADVANCED_FACE('',(#2825),#17265,.F.);
#18150=ADVANCED_FACE('',(#2826),#17266,.F.);
#18151=ADVANCED_FACE('',(#2827),#17267,.F.);
#18152=ADVANCED_FACE('',(#2828),#17268,.F.);
#18153=ADVANCED_FACE('',(#2829),#17269,.F.);
#18154=ADVANCED_FACE('',(#2830),#17270,.F.);
#18155=ADVANCED_FACE('',(#2831),#17271,.F.);
#18156=ADVANCED_FACE('',(#2832),#17272,.F.);
#18157=ADVANCED_FACE('',(#2833),#17273,.F.);
#18158=ADVANCED_FACE('',(#2834),#17274,.F.);
#18159=ADVANCED_FACE('',(#2835),#17275,.F.);
#18160=ADVANCED_FACE('',(#2836),#17276,.F.);
#18161=ADVANCED_FACE('',(#2837),#17277,.F.);
#18162=ADVANCED_FACE('',(#2838),#17278,.F.);
#18163=ADVANCED_FACE('',(#2839),#17279,.F.);
#18164=ADVANCED_FACE('',(#2840),#2024,.T.);
#18165=ADVANCED_FACE('',(#2841),#2025,.T.);
#18166=ADVANCED_FACE('',(#2842),#2026,.T.);
#18167=ADVANCED_FACE('',(#2843),#2027,.T.);
#18168=ADVANCED_FACE('',(#2844,#1477,#1478,#1479,#1480,#1481,#1482,#1483,
#1484,#1485,#1486,#1487,#1488,#1489,#1490,#1491,#1492,#1493,#1494),#2028,
 .T.);
#18169=ADVANCED_FACE('',(#2845,#1495,#1496,#1497,#1498,#1499,#1500,#1501,
#1502,#1503,#1504,#1505,#1506,#1507,#1508,#1509,#1510,#1511,#1512),#2029,
 .F.);
#18170=ADVANCED_FACE('',(#2846),#2030,.T.);
#18171=ADVANCED_FACE('',(#2847),#17280,.F.);
#18172=ADVANCED_FACE('',(#2848),#2031,.T.);
#18173=ADVANCED_FACE('',(#2849),#17281,.F.);
#18174=ADVANCED_FACE('',(#2850),#2032,.T.);
#18175=ADVANCED_FACE('',(#2851),#17282,.F.);
#18176=ADVANCED_FACE('',(#2852),#2033,.T.);
#18177=ADVANCED_FACE('',(#2853),#17283,.F.);
#18178=ADVANCED_FACE('',(#2854),#17284,.T.);
#18179=ADVANCED_FACE('',(#2855),#17285,.F.);
#18180=ADVANCED_FACE('',(#2856,#1513),#2034,.T.);
#18181=ADVANCED_FACE('',(#2857,#1514),#2035,.F.);
#18182=ADVANCED_FACE('',(#2858),#17286,.T.);
#18183=ADVANCED_FACE('',(#2859),#17287,.F.);
#18184=ADVANCED_FACE('',(#2860,#1515,#1516,#1517,#1518,#1519),#2036,.T.);
#18185=ADVANCED_FACE('',(#2861,#1520),#2037,.F.);
#18186=ADVANCED_FACE('',(#2862),#2038,.T.);
#18187=ADVANCED_FACE('',(#2863),#17288,.F.);
#18188=ADVANCED_FACE('',(#2864),#2039,.T.);
#18189=ADVANCED_FACE('',(#2865),#17289,.F.);
#18190=ADVANCED_FACE('',(#2866),#2040,.T.);
#18191=ADVANCED_FACE('',(#2867),#17290,.F.);
#18192=ADVANCED_FACE('',(#2868),#2041,.T.);
#18193=ADVANCED_FACE('',(#2869),#17291,.F.);
#18194=ADVANCED_FACE('',(#2870),#17292,.T.);
#18195=ADVANCED_FACE('',(#2871),#17293,.F.);
#18196=ADVANCED_FACE('',(#2872,#1521),#2042,.T.);
#18197=ADVANCED_FACE('',(#2873,#1522),#2043,.F.);
#18198=ADVANCED_FACE('',(#2874),#17294,.T.);
#18199=ADVANCED_FACE('',(#2875),#17295,.F.);
#18200=ADVANCED_FACE('',(#2876,#1523,#1524,#1525,#1526,#1527),#2044,.T.);
#18201=ADVANCED_FACE('',(#2877,#1528),#2045,.F.);
#18202=ADVANCED_FACE('',(#2878),#17296,.F.);
#18203=ADVANCED_FACE('',(#2879),#2046,.T.);
#18204=ADVANCED_FACE('',(#2880),#17297,.F.);
#18205=ADVANCED_FACE('',(#2881),#2047,.T.);
#18206=ADVANCED_FACE('',(#2882),#17298,.F.);
#18207=ADVANCED_FACE('',(#2883),#2048,.T.);
#18208=ADVANCED_FACE('',(#2884),#17299,.F.);
#18209=ADVANCED_FACE('',(#2885),#17300,.T.);
#18210=ADVANCED_FACE('',(#2886,#1529,#1530,#1531,#1532),#2049,.T.);
#18211=ADVANCED_FACE('',(#2887,#1533),#2050,.F.);
#18212=ADVANCED_FACE('',(#2888),#17301,.F.);
#18213=ADVANCED_FACE('',(#2889),#17302,.F.);
#18214=ADVANCED_FACE('',(#2890),#17303,.T.);
#18215=ADVANCED_FACE('',(#2891,#1534,#1535),#2051,.T.);
#18216=ADVANCED_FACE('',(#2892,#1536,#1537),#2052,.F.);
#18217=ADVANCED_FACE('',(#2893),#17304,.F.);
#18218=ADVANCED_FACE('',(#2894),#17305,.F.);
#18219=ADVANCED_FACE('',(#2895),#2053,.T.);
#18220=ADVANCED_FACE('',(#2896),#2054,.T.);
#18221=ADVANCED_FACE('',(#2897),#2055,.T.);
#18222=ADVANCED_FACE('',(#2898),#2056,.T.);
#18223=ADVANCED_FACE('',(#2899,#1538,#1539),#2057,.F.);
#18224=ADVANCED_FACE('',(#2900),#2058,.T.);
#18225=ADVANCED_FACE('',(#2901),#2059,.T.);
#18226=ADVANCED_FACE('',(#2902),#2060,.T.);
#18227=ADVANCED_FACE('',(#2903),#2061,.T.);
#18228=ADVANCED_FACE('',(#2904),#2062,.T.);
#18229=ADVANCED_FACE('',(#2905),#2063,.T.);
#18230=ADVANCED_FACE('',(#2906,#1540,#1541),#2064,.T.);
#18231=ADVANCED_FACE('',(#2907),#2065,.F.);
#18232=ADVANCED_FACE('',(#2908),#2066,.F.);
#18233=ADVANCED_FACE('',(#2909),#2067,.F.);
#18234=ADVANCED_FACE('',(#2910),#2068,.F.);
#18235=ADVANCED_FACE('',(#2911),#2069,.F.);
#18236=ADVANCED_FACE('',(#2912),#2070,.F.);
#18237=ADVANCED_FACE('',(#2913,#1542),#2071,.T.);
#18238=ADVANCED_FACE('',(#2914),#17306,.T.);
#18239=ADVANCED_FACE('',(#2915,#1543),#2072,.T.);
#18240=ADVANCED_FACE('',(#2916),#17307,.T.);
#18241=ADVANCED_FACE('',(#2917,#1544),#2073,.T.);
#18242=ADVANCED_FACE('',(#2918),#17308,.T.);
#18243=ADVANCED_FACE('',(#2919,#1545),#2074,.T.);
#18244=ADVANCED_FACE('',(#2920),#17309,.T.);
#18245=ADVANCED_FACE('',(#2921,#1546),#2075,.T.);
#18246=ADVANCED_FACE('',(#2922),#17310,.T.);
#18247=ADVANCED_FACE('',(#2923,#1547),#2076,.T.);
#18248=ADVANCED_FACE('',(#2924,#1548),#17311,.F.);
#18249=ADVANCED_FACE('',(#2925),#2077,.F.);
#18250=ADVANCED_FACE('',(#2926),#2078,.F.);
#18251=ADVANCED_FACE('',(#2927),#2079,.F.);
#18252=ADVANCED_FACE('',(#2928),#2080,.F.);
#18253=ADVANCED_FACE('',(#2929,#1549),#2081,.T.);
#18254=ADVANCED_FACE('',(#2930,#1550),#17312,.T.);
#18255=ADVANCED_FACE('',(#2931,#1551),#2082,.T.);
#18256=ADVANCED_FACE('',(#2932,#1552),#17313,.F.);
#18257=ADVANCED_FACE('',(#2933),#17314,.F.);
#18258=ADVANCED_FACE('',(#2934),#17315,.F.);
#18259=ADVANCED_FACE('',(#2935),#17316,.F.);
#18260=ADVANCED_FACE('',(#2936),#17317,.F.);
#18261=ADVANCED_FACE('',(#2937),#17318,.F.);
#18262=ADVANCED_FACE('',(#2938),#17319,.F.);
#18263=ADVANCED_FACE('',(#2939),#17320,.F.);
#18264=ADVANCED_FACE('',(#2940),#17321,.F.);
#18265=ADVANCED_FACE('',(#2941),#17322,.F.);
#18266=ADVANCED_FACE('',(#2942),#17323,.F.);
#18267=ADVANCED_FACE('',(#2943),#17324,.F.);
#18268=ADVANCED_FACE('',(#2944),#17325,.F.);
#18269=ADVANCED_FACE('',(#2945),#17326,.F.);
#18270=ADVANCED_FACE('',(#2946),#17327,.F.);
#18271=ADVANCED_FACE('',(#2947),#17328,.F.);
#18272=ADVANCED_FACE('',(#2948),#17329,.F.);
#18273=ADVANCED_FACE('',(#2949),#17330,.F.);
#18274=ADVANCED_FACE('',(#2950),#17331,.F.);
#18275=ADVANCED_FACE('',(#2951),#17332,.F.);
#18276=ADVANCED_FACE('',(#2952),#11,.F.);
#18277=ADVANCED_FACE('',(#2953),#12,.F.);
#18278=ADVANCED_FACE('',(#2954,#1553,#1554,#1555,#1556),#2083,.T.);
#18279=ADVANCED_FACE('',(#2955),#17333,.F.);
#18280=ADVANCED_FACE('',(#2956),#17334,.F.);
#18281=ADVANCED_FACE('',(#2957),#17335,.F.);
#18282=ADVANCED_FACE('',(#2958),#2084,.F.);
#18283=ADVANCED_FACE('',(#2959,#1557,#1558,#1559,#1560),#2085,.F.);
#18284=ADVANCED_FACE('',(#2960),#17336,.T.);
#18285=ADVANCED_FACE('',(#2961),#17337,.F.);
#18286=ADVANCED_FACE('',(#2962),#17338,.T.);
#18287=ADVANCED_FACE('',(#2963,#1561),#2086,.F.);
#18288=ADVANCED_FACE('',(#2964),#2087,.F.);
#18289=ADVANCED_FACE('',(#2965),#2088,.F.);
#18290=ADVANCED_FACE('',(#2966),#2089,.F.);
#18291=ADVANCED_FACE('',(#2967),#2090,.F.);
#18292=ADVANCED_FACE('',(#2968),#2091,.F.);
#18293=ADVANCED_FACE('',(#2969),#2092,.F.);
#18294=ADVANCED_FACE('',(#2970),#2093,.F.);
#18295=ADVANCED_FACE('',(#2971),#2094,.F.);
#18296=ADVANCED_FACE('',(#2972,#1562),#2095,.T.);
#18297=ADVANCED_FACE('',(#2973),#17339,.T.);
#18298=ADVANCED_FACE('',(#2974),#2096,.F.);
#18299=ADVANCED_FACE('',(#2975),#2097,.T.);
#18300=ADVANCED_FACE('',(#2976),#971,.T.);
#18301=ADVANCED_FACE('',(#2977),#17340,.T.);
#18302=ADVANCED_FACE('',(#2978),#972,.T.);
#18303=ADVANCED_FACE('',(#2979,#1563),#2098,.T.);
#18304=ADVANCED_FACE('',(#2980),#973,.T.);
#18305=ADVANCED_FACE('',(#2981),#17341,.T.);
#18306=ADVANCED_FACE('',(#2982),#2099,.T.);
#18307=ADVANCED_FACE('',(#2983),#974,.T.);
#18308=ADVANCED_FACE('',(#2984),#17342,.T.);
#18309=ADVANCED_FACE('',(#2985),#975,.T.);
#18310=ADVANCED_FACE('',(#2986,#1564),#2100,.T.);
#18311=ADVANCED_FACE('',(#2987),#976,.T.);
#18312=ADVANCED_FACE('',(#2988),#17343,.T.);
#18313=ADVANCED_FACE('',(#2989),#977,.T.);
#18314=ADVANCED_FACE('',(#2990),#2101,.T.);
#18315=ADVANCED_FACE('',(#2991),#2102,.F.);
#18316=ADVANCED_FACE('',(#2992),#2103,.F.);
#18317=ADVANCED_FACE('',(#2993),#2104,.F.);
#18318=ADVANCED_FACE('',(#2994),#2105,.F.);
#18319=ADVANCED_FACE('',(#2995),#2106,.F.);
#18320=ADVANCED_FACE('',(#2996),#2107,.F.);
#18321=ADVANCED_FACE('',(#2997),#2108,.F.);
#18322=ADVANCED_FACE('',(#2998),#2109,.F.);
#18323=ADVANCED_FACE('',(#2999),#17344,.T.);
#18324=ADVANCED_FACE('',(#3000),#17345,.T.);
#18325=ADVANCED_FACE('',(#3001),#17346,.T.);
#18326=ADVANCED_FACE('',(#3002),#17347,.T.);
#18327=ADVANCED_FACE('',(#3003),#17348,.T.);
#18328=ADVANCED_FACE('',(#3004),#17349,.T.);
#18329=ADVANCED_FACE('',(#3005),#17350,.T.);
#18330=ADVANCED_FACE('',(#3006),#17351,.T.);
#18331=ADVANCED_FACE('',(#3007),#17352,.T.);
#18332=ADVANCED_FACE('',(#3008),#17353,.T.);
#18333=ADVANCED_FACE('',(#3009),#17354,.T.);
#18334=ADVANCED_FACE('',(#3010),#17355,.T.);
#18335=ADVANCED_FACE('',(#3011),#17356,.T.);
#18336=ADVANCED_FACE('',(#3012),#17357,.T.);
#18337=ADVANCED_FACE('',(#3013),#17358,.T.);
#18338=ADVANCED_FACE('',(#3014),#17359,.T.);
#18339=ADVANCED_FACE('',(#3015),#17360,.T.);
#18340=ADVANCED_FACE('',(#3016),#17361,.T.);
#18341=ADVANCED_FACE('',(#3017),#17362,.T.);
#18342=ADVANCED_FACE('',(#3018),#17363,.T.);
#18343=ADVANCED_FACE('',(#3019),#17364,.T.);
#18344=ADVANCED_FACE('',(#3020),#17365,.T.);
#18345=ADVANCED_FACE('',(#3021),#17366,.T.);
#18346=ADVANCED_FACE('',(#3022),#17367,.T.);
#18347=ADVANCED_FACE('',(#3023),#17368,.T.);
#18348=ADVANCED_FACE('',(#3024),#17369,.T.);
#18349=ADVANCED_FACE('',(#3025),#17370,.T.);
#18350=ADVANCED_FACE('',(#3026),#17371,.T.);
#18351=ADVANCED_FACE('',(#3027),#17372,.T.);
#18352=ADVANCED_FACE('',(#3028),#17373,.T.);
#18353=ADVANCED_FACE('',(#3029),#17374,.T.);
#18354=ADVANCED_FACE('',(#3030),#17375,.T.);
#18355=ADVANCED_FACE('',(#3031),#17376,.T.);
#18356=ADVANCED_FACE('',(#3032),#17377,.T.);
#18357=ADVANCED_FACE('',(#3033),#17378,.T.);
#18358=ADVANCED_FACE('',(#3034),#17379,.T.);
#18359=ADVANCED_FACE('',(#3035),#17380,.T.);
#18360=ADVANCED_FACE('',(#3036),#17381,.T.);
#18361=ADVANCED_FACE('',(#3037),#17382,.T.);
#18362=ADVANCED_FACE('',(#3038),#17383,.T.);
#18363=ADVANCED_FACE('',(#3039),#17384,.T.);
#18364=ADVANCED_FACE('',(#3040),#17385,.T.);
#18365=ADVANCED_FACE('',(#3041),#17386,.T.);
#18366=ADVANCED_FACE('',(#3042),#17387,.T.);
#18367=ADVANCED_FACE('',(#3043),#17388,.T.);
#18368=ADVANCED_FACE('',(#3044),#17389,.T.);
#18369=ADVANCED_FACE('',(#3045),#17390,.T.);
#18370=ADVANCED_FACE('',(#3046),#17391,.T.);
#18371=ADVANCED_FACE('',(#3047),#17392,.T.);
#18372=ADVANCED_FACE('',(#3048),#17393,.T.);
#18373=ADVANCED_FACE('',(#3049),#17394,.T.);
#18374=ADVANCED_FACE('',(#3050),#17395,.T.);
#18375=ADVANCED_FACE('',(#3051),#17396,.T.);
#18376=ADVANCED_FACE('',(#3052),#17397,.T.);
#18377=ADVANCED_FACE('',(#3053),#17398,.T.);
#18378=ADVANCED_FACE('',(#3054),#17399,.T.);
#18379=ADVANCED_FACE('',(#3055),#17400,.T.);
#18380=ADVANCED_FACE('',(#3056),#17401,.T.);
#18381=ADVANCED_FACE('',(#3057),#17402,.T.);
#18382=ADVANCED_FACE('',(#3058),#17403,.T.);
#18383=ADVANCED_FACE('',(#3059),#17404,.T.);
#18384=ADVANCED_FACE('',(#3060),#17405,.T.);
#18385=ADVANCED_FACE('',(#3061),#17406,.T.);
#18386=ADVANCED_FACE('',(#3062),#17407,.T.);
#18387=ADVANCED_FACE('',(#3063),#17408,.T.);
#18388=ADVANCED_FACE('',(#3064),#17409,.T.);
#18389=ADVANCED_FACE('',(#3065),#17410,.T.);
#18390=ADVANCED_FACE('',(#3066),#17411,.T.);
#18391=ADVANCED_FACE('',(#3067),#17412,.T.);
#18392=ADVANCED_FACE('',(#3068),#17413,.T.);
#18393=ADVANCED_FACE('',(#3069),#17414,.T.);
#18394=ADVANCED_FACE('',(#3070),#17415,.T.);
#18395=ADVANCED_FACE('',(#3071),#17416,.T.);
#18396=ADVANCED_FACE('',(#3072),#17417,.T.);
#18397=ADVANCED_FACE('',(#3073),#17418,.T.);
#18398=ADVANCED_FACE('',(#3074),#17419,.T.);
#18399=ADVANCED_FACE('',(#3075),#17420,.T.);
#18400=ADVANCED_FACE('',(#3076),#17421,.T.);
#18401=ADVANCED_FACE('',(#3077),#17422,.T.);
#18402=ADVANCED_FACE('',(#3078),#17423,.T.);
#18403=ADVANCED_FACE('',(#3079),#17424,.T.);
#18404=ADVANCED_FACE('',(#3080),#17425,.T.);
#18405=ADVANCED_FACE('',(#3081),#17426,.T.);
#18406=ADVANCED_FACE('',(#3082),#17427,.T.);
#18407=ADVANCED_FACE('',(#3083),#17428,.T.);
#18408=ADVANCED_FACE('',(#3084),#17429,.T.);
#18409=ADVANCED_FACE('',(#3085),#17430,.T.);
#18410=ADVANCED_FACE('',(#3086),#17431,.T.);
#18411=ADVANCED_FACE('',(#3087),#17432,.T.);
#18412=ADVANCED_FACE('',(#3088),#17433,.T.);
#18413=ADVANCED_FACE('',(#3089),#17434,.T.);
#18414=ADVANCED_FACE('',(#3090),#17435,.T.);
#18415=ADVANCED_FACE('',(#3091),#17436,.T.);
#18416=ADVANCED_FACE('',(#3092),#17437,.T.);
#18417=ADVANCED_FACE('',(#3093),#17438,.T.);
#18418=ADVANCED_FACE('',(#3094),#17439,.T.);
#18419=ADVANCED_FACE('',(#3095),#17440,.T.);
#18420=ADVANCED_FACE('',(#3096),#17441,.T.);
#18421=ADVANCED_FACE('',(#3097),#17442,.T.);
#18422=ADVANCED_FACE('',(#3098),#17443,.T.);
#18423=ADVANCED_FACE('',(#3099),#17444,.T.);
#18424=ADVANCED_FACE('',(#3100),#17445,.T.);
#18425=ADVANCED_FACE('',(#3101),#17446,.T.);
#18426=ADVANCED_FACE('',(#3102),#17447,.T.);
#18427=ADVANCED_FACE('',(#3103),#17448,.T.);
#18428=ADVANCED_FACE('',(#3104),#17449,.T.);
#18429=ADVANCED_FACE('',(#3105),#17450,.T.);
#18430=ADVANCED_FACE('',(#3106),#17451,.T.);
#18431=ADVANCED_FACE('',(#3107),#17452,.T.);
#18432=ADVANCED_FACE('',(#3108),#17453,.T.);
#18433=ADVANCED_FACE('',(#3109),#17454,.T.);
#18434=ADVANCED_FACE('',(#3110),#17455,.T.);
#18435=ADVANCED_FACE('',(#3111),#17456,.T.);
#18436=ADVANCED_FACE('',(#3112),#17457,.T.);
#18437=ADVANCED_FACE('',(#3113),#17458,.T.);
#18438=ADVANCED_FACE('',(#3114),#17459,.T.);
#18439=ADVANCED_FACE('',(#3115),#17460,.T.);
#18440=ADVANCED_FACE('',(#3116),#17461,.T.);
#18441=ADVANCED_FACE('',(#3117),#17462,.T.);
#18442=ADVANCED_FACE('',(#3118),#17463,.T.);
#18443=ADVANCED_FACE('',(#3119),#17464,.T.);
#18444=ADVANCED_FACE('',(#3120),#17465,.T.);
#18445=ADVANCED_FACE('',(#3121),#17466,.T.);
#18446=ADVANCED_FACE('',(#3122),#17467,.T.);
#18447=ADVANCED_FACE('',(#3123),#17468,.T.);
#18448=ADVANCED_FACE('',(#3124),#17469,.T.);
#18449=ADVANCED_FACE('',(#3125,#1565),#2110,.T.);
#18450=ADVANCED_FACE('',(#3126),#17470,.T.);
#18451=ADVANCED_FACE('',(#3127),#2111,.F.);
#18452=ADVANCED_FACE('',(#3128),#13,.F.);
#18453=ADVANCED_FACE('',(#3129),#17471,.T.);
#18454=ADVANCED_FACE('',(#3130),#14,.F.);
#18455=ADVANCED_FACE('',(#3131),#2112,.F.);
#18456=ADVANCED_FACE('',(#3132),#2113,.T.);
#18457=ADVANCED_FACE('',(#3133),#2114,.F.);
#18458=ADVANCED_FACE('',(#3134),#2115,.F.);
#18459=ADVANCED_FACE('',(#3135),#2116,.F.);
#18460=ADVANCED_FACE('',(#3136,#1566),#17472,.T.);
#18461=ADVANCED_FACE('',(#3137),#2117,.T.);
#18462=ADVANCED_FACE('',(#3138,#1567),#2118,.F.);
#18463=ADVANCED_FACE('',(#3139),#17473,.T.);
#18464=ADVANCED_FACE('',(#3140,#1568),#2119,.T.);
#18465=ADVANCED_FACE('',(#3141),#17474,.T.);
#18466=ADVANCED_FACE('',(#3142),#17475,.F.);
#18467=ADVANCED_FACE('',(#3143),#17476,.T.);
#18468=ADVANCED_FACE('',(#3144,#1569),#2120,.T.);
#18469=ADVANCED_FACE('',(#3145,#1570),#2121,.F.);
#18470=ADVANCED_FACE('',(#3146),#2122,.T.);
#18471=ADVANCED_FACE('',(#3147),#17477,.F.);
#18472=ADVANCED_FACE('',(#3148),#2123,.T.);
#18473=ADVANCED_FACE('',(#3149,#1571),#17478,.F.);
#18474=ADVANCED_FACE('',(#3150,#1572),#17479,.T.);
#18475=ADVANCED_FACE('',(#3151,#1573),#2124,.T.);
#18476=ADVANCED_FACE('',(#3152,#1574),#2125,.F.);
#18477=ADVANCED_FACE('',(#3153),#17480,.F.);
#18478=ADVANCED_FACE('',(#3154),#2126,.T.);
#18479=ADVANCED_FACE('',(#3155),#17481,.F.);
#18480=ADVANCED_FACE('',(#3156),#2127,.T.);
#18481=ADVANCED_FACE('',(#3157),#2128,.F.);
#18482=ADVANCED_FACE('',(#3158),#2129,.F.);
#18483=ADVANCED_FACE('',(#3159),#2130,.F.);
#18484=ADVANCED_FACE('',(#3160,#1575,#1576),#2131,.T.);
#18485=ADVANCED_FACE('',(#3161,#1577,#1578),#2132,.F.);
#18486=ADVANCED_FACE('',(#3162),#17482,.T.);
#18487=ADVANCED_FACE('',(#3163,#1579),#17483,.F.);
#18488=ADVANCED_FACE('',(#3164,#1580),#17484,.T.);
#18489=ADVANCED_FACE('',(#3165),#2133,.F.);
#18490=ADVANCED_FACE('',(#3166),#17485,.F.);
#18491=ADVANCED_FACE('',(#3167),#17486,.T.);
#18492=ADVANCED_FACE('',(#3168,#1581),#2134,.T.);
#18493=ADVANCED_FACE('',(#3169,#1582),#2135,.F.);
#18494=ADVANCED_FACE('',(#3170),#17487,.F.);
#18495=ADVANCED_FACE('',(#3171),#17488,.T.);
#18496=ADVANCED_FACE('',(#3172,#1583),#2136,.T.);
#18497=ADVANCED_FACE('',(#3173,#1584),#2137,.F.);
#18498=ADVANCED_FACE('',(#3174),#2138,.F.);
#18499=ADVANCED_FACE('',(#3175),#2139,.T.);
#18500=ADVANCED_FACE('',(#3176),#2140,.T.);
#18501=ADVANCED_FACE('',(#3177),#2141,.T.);
#18502=ADVANCED_FACE('',(#3178),#2142,.T.);
#18503=ADVANCED_FACE('',(#3179),#2143,.T.);
#18504=ADVANCED_FACE('',(#3180),#2144,.F.);
#18505=ADVANCED_FACE('',(#3181),#2145,.T.);
#18506=ADVANCED_FACE('',(#3182),#2146,.T.);
#18507=ADVANCED_FACE('',(#3183),#2147,.T.);
#18508=ADVANCED_FACE('',(#3184),#2148,.F.);
#18509=ADVANCED_FACE('',(#3185),#2149,.F.);
#18510=ADVANCED_FACE('',(#3186),#2150,.F.);
#18511=ADVANCED_FACE('',(#3187),#2151,.F.);
#18512=ADVANCED_FACE('',(#3188),#2152,.F.);
#18513=ADVANCED_FACE('',(#3189),#2153,.F.);
#18514=ADVANCED_FACE('',(#3190),#2154,.F.);
#18515=ADVANCED_FACE('',(#3191,#1585),#2155,.T.);
#18516=ADVANCED_FACE('',(#3192),#978,.T.);
#18517=ADVANCED_FACE('',(#3193),#17489,.T.);
#18518=ADVANCED_FACE('',(#3194),#979,.T.);
#18519=ADVANCED_FACE('',(#3195),#2156,.T.);
#18520=ADVANCED_FACE('',(#3196),#17490,.F.);
#18521=ADVANCED_FACE('',(#3197),#17491,.T.);
#18522=ADVANCED_FACE('',(#3198,#1586),#2157,.T.);
#18523=ADVANCED_FACE('',(#3199,#1587),#2158,.F.);
#18524=ADVANCED_FACE('',(#3200),#2159,.T.);
#18525=ADVANCED_FACE('',(#3201),#980,.T.);
#18526=ADVANCED_FACE('',(#3202),#17492,.T.);
#18527=ADVANCED_FACE('',(#3203),#981,.T.);
#18528=ADVANCED_FACE('',(#3204,#1588),#2160,.T.);
#18529=ADVANCED_FACE('',(#3205),#982,.T.);
#18530=ADVANCED_FACE('',(#3206),#17493,.T.);
#18531=ADVANCED_FACE('',(#3207),#983,.T.);
#18532=ADVANCED_FACE('',(#3208),#2161,.T.);
#18533=ADVANCED_FACE('',(#3209),#2162,.F.);
#18534=ADVANCED_FACE('',(#3210),#2163,.F.);
#18535=ADVANCED_FACE('',(#3211),#2164,.F.);
#18536=ADVANCED_FACE('',(#3212),#2165,.F.);
#18537=ADVANCED_FACE('',(#3213),#2166,.F.);
#18538=ADVANCED_FACE('',(#3214),#2167,.F.);
#18539=ADVANCED_FACE('',(#3215),#2168,.F.);
#18540=ADVANCED_FACE('',(#3216),#2169,.F.);
#18541=CLOSED_SHELL('',(#17494,#17495,#17496,#17497,#17498,#17499,#17500,
#17501,#17502,#17503,#17504,#17505,#17506,#17507,#17508,#17509,#17510,#17511,
#17512,#17513,#17514,#17515,#17516,#17517,#17518,#17519,#17520,#17521,#17522,
#17523,#17524,#17525,#17526,#17527));
#18542=CLOSED_SHELL('',(#17528,#17529,#17530,#17531,#17532,#17533));
#18543=CLOSED_SHELL('',(#17534,#17535,#17536,#17537,#17538,#17539));
#18544=CLOSED_SHELL('',(#17540,#17541,#17542,#17543,#17544,#17545,#17546,
#17547,#17548,#17549,#17550,#17551,#17552,#17553,#17554,#17555,#17556,#17557,
#17558,#17559));
#18545=CLOSED_SHELL('',(#17560,#17561,#17562,#17563,#17564,#17565,#17566,
#17567,#17568,#17569,#17570,#17571,#17572,#17573,#17574,#17575));
#18546=CLOSED_SHELL('',(#17576,#17577,#17578,#17579,#17580,#17581,#17582,
#17583,#17584,#17585,#17586,#17587,#17588,#17589,#17590,#17591));
#18547=CLOSED_SHELL('',(#17592,#17593,#17594,#17595,#17596,#17597,#17598,
#17599,#17600,#17601,#17602,#17603));
#18548=CLOSED_SHELL('',(#17604,#17605,#17606,#17607,#17608,#17609,#17610,
#17611,#17612,#17613,#17614,#17615,#17616,#17617));
#18549=CLOSED_SHELL('',(#17618,#17619,#17620,#17621,#17622,#17623,#17624,
#17625,#17626,#17627,#17628,#17629));
#18550=CLOSED_SHELL('',(#17630,#17631,#17632,#17633,#17634,#17635,#17636,
#17637,#17638,#17639,#17640,#17641,#17642,#17643));
#18551=CLOSED_SHELL('',(#17644,#17645,#17646,#17647,#17648,#17649,#17650,
#17651,#17652,#17653,#17654,#17655,#17656,#17657,#17658,#17659,#17660,#17661,
#17662,#17663,#17664,#17665));
#18552=CLOSED_SHELL('',(#17666,#17667,#17668,#17669,#17670,#17671,#17672,
#17673,#17674,#17675,#17676,#17677,#17678,#17679,#17680,#17681,#17682,#17683,
#17684,#17685,#17686,#17687,#17688,#17689));
#18553=CLOSED_SHELL('',(#17690,#17691,#17692,#17693,#17694,#17695,#17696,
#17697,#17698));
#18554=CLOSED_SHELL('',(#17699,#17700,#17701,#17702,#17703,#17704,#17705,
#17706,#17707));
#18555=CLOSED_SHELL('',(#17708,#17709,#17710,#17711,#17712));
#18556=CLOSED_SHELL('',(#17713,#17714,#17715,#17716,#17717));
#18557=CLOSED_SHELL('',(#17718,#17719,#17720,#17721,#17722));
#18558=CLOSED_SHELL('',(#17723,#17724,#17725,#17726,#17727));
#18559=CLOSED_SHELL('',(#17728,#17729,#17730,#17731,#17732,#17733,#17734,
#17735,#17736,#17737,#17738,#17739,#17740,#17741,#17742));
#18560=CLOSED_SHELL('',(#17743,#17744,#17745,#17746,#17747,#17748,#17749,
#17750,#17751,#17752,#17753,#17754,#17755,#17756,#17757,#17758,#17759,#17760,
#17761,#17762,#17763,#17764,#17765,#17766,#17767,#17768,#17769,#17770,#17771,
#17772,#17773,#17774,#17775,#17776,#17777,#17778,#17779,#17780,#17781,#17782,
#17783,#17784,#17785,#17786,#17787,#17788,#17789,#17790,#17791,#17792,#17793,
#17794,#17795,#17796,#17797,#17798,#17799,#17800,#17801,#17802,#17803,#17804,
#17805,#17806,#17807,#17808,#17809,#17810,#17811,#17812,#17813,#17814,#17815,
#17816,#17817,#17818,#17819,#17820,#17821,#17822,#17823,#17824,#17825,#17826,
#17827,#17828,#17829,#17830,#17831,#17832,#17833,#17834,#17835,#17836,#17837,
#17838,#17839,#17840,#17841,#17842,#17843,#17844,#17845,#17846,#17847,#17848,
#17849,#17850,#17851,#17852,#17853,#17854,#17855,#17856,#17857,#17858,#17859,
#17860,#17861,#17862,#17863,#17864,#17865,#17866,#17867,#17868,#17869,#17870,
#17871,#17872,#17873,#17874,#17875));
#18561=CLOSED_SHELL('',(#17876,#17877,#17878,#17879,#17880));
#18562=CLOSED_SHELL('',(#17881,#17882,#17883,#17884,#17885,#17886,#17887,
#17888,#17889,#17890,#17891,#17892,#17893,#17894,#17895,#17896,#17897,#17898,
#17899,#17900,#17901,#17902,#17903));
#18563=CLOSED_SHELL('',(#17904,#17905,#17906,#17907,#17908,#17909,#17910,
#17911));
#18564=CLOSED_SHELL('',(#17912,#17913,#17914,#17915,#17916,#17917,#17918,
#17919));
#18565=CLOSED_SHELL('',(#17920,#17921,#17922,#17923,#17924,#17925,#17926,
#17927));
#18566=CLOSED_SHELL('',(#17928,#17929,#17930,#17931,#17932,#17933,#17934,
#17935));
#18567=CLOSED_SHELL('',(#17936));
#18568=CLOSED_SHELL('',(#17937));
#18569=CLOSED_SHELL('',(#17938));
#18570=CLOSED_SHELL('',(#17939));
#18571=CLOSED_SHELL('',(#17940));
#18572=CLOSED_SHELL('',(#17941));
#18573=CLOSED_SHELL('',(#17942));
#18574=CLOSED_SHELL('',(#17943,#17944,#17945,#17946,#17947,#17948,#17949,
#17950,#17951,#17952,#17953,#17954,#17955,#17956,#17957,#17958,#17959));
#18575=CLOSED_SHELL('',(#17960,#17961,#17962,#17963));
#18576=CLOSED_SHELL('',(#17964,#17965,#17966,#17967));
#18577=CLOSED_SHELL('',(#17968,#17969,#17970,#17971,#17972,#17973,#17974,
#17975));
#18578=CLOSED_SHELL('',(#17976,#17977,#17978,#17979,#17980,#17981,#17982,
#17983));
#18579=CLOSED_SHELL('',(#17984));
#18580=CLOSED_SHELL('',(#17985));
#18581=CLOSED_SHELL('',(#17986));
#18582=CLOSED_SHELL('',(#17987));
#18583=CLOSED_SHELL('',(#17988));
#18584=CLOSED_SHELL('',(#17989));
#18585=CLOSED_SHELL('',(#17990));
#18586=CLOSED_SHELL('',(#17991));
#18587=CLOSED_SHELL('',(#17992,#17993,#17994,#17995,#17996,#17997,#17998,
#17999,#18000,#18001,#18002,#18003,#18004,#18005,#18006,#18007,#18008,#18009,
#18010));
#18588=CLOSED_SHELL('',(#18011,#18012,#18013,#18014));
#18589=CLOSED_SHELL('',(#18015,#18016,#18017,#18018));
#18590=CLOSED_SHELL('',(#18019,#18020,#18021,#18022,#18023,#18024,#18025,
#18026,#18027,#18028));
#18591=CLOSED_SHELL('',(#18029,#18030,#18031,#18032,#18033,#18034,#18035,
#18036));
#18592=CLOSED_SHELL('',(#18037,#18038,#18039,#18040,#18041,#18042,#18043,
#18044));
#18593=CLOSED_SHELL('',(#18045,#18046,#18047,#18048,#18049,#18050,#18051,
#18052));
#18594=CLOSED_SHELL('',(#18053,#18054,#18055,#18056,#18057,#18058,#18059,
#18060,#18061,#18062,#18063,#18064,#18065,#18066,#18067,#18068,#18069,#18070,
#18071,#18072,#18073,#18074,#18075,#18076,#18077,#18078,#18079,#18080,#18081,
#18082,#18083,#18084,#18085,#18086,#18087,#18088,#18089,#18090,#18091,#18092,
#18093,#18094,#18095,#18096,#18097,#18098,#18099));
#18595=CLOSED_SHELL('',(#18100,#18101,#18102,#18103,#18104,#18105,#18106,
#18107,#18108));
#18596=CLOSED_SHELL('',(#18109,#18110,#18111,#18112,#18113,#18114,#18115,
#18116));
#18597=CLOSED_SHELL('',(#18117,#18118,#18119,#18120,#18121,#18122,#18123,
#18124,#18125,#18126,#18127,#18128,#18129,#18130));
#18598=CLOSED_SHELL('',(#18131,#18132,#18133,#18134,#18135,#18136,#18137,
#18138,#18139,#18140,#18141,#18142,#18143,#18144,#18145));
#18599=CLOSED_SHELL('',(#18146,#18147,#18148,#18149,#18150,#18151,#18152,
#18153,#18154,#18155,#18156,#18157,#18158,#18159,#18160,#18161,#18162,#18163,
#18164,#18165,#18166,#18167,#18168,#18169));
#18600=CLOSED_SHELL('',(#18170,#18171,#18172,#18173,#18174,#18175,#18176,
#18177,#18178,#18179,#18180,#18181,#18182,#18183,#18184,#18185));
#18601=CLOSED_SHELL('',(#18186,#18187,#18188,#18189,#18190,#18191,#18192,
#18193,#18194,#18195,#18196,#18197,#18198,#18199,#18200,#18201));
#18602=CLOSED_SHELL('',(#18202,#18203,#18204,#18205,#18206,#18207,#18208,
#18209,#18210,#18211));
#18603=CLOSED_SHELL('',(#18212,#18213,#18214,#18215,#18216));
#18604=CLOSED_SHELL('',(#18217,#18218,#18219,#18220,#18221,#18222,#18223,
#18224,#18225,#18226,#18227,#18228,#18229,#18230,#18231));
#18605=CLOSED_SHELL('',(#18232,#18233,#18234,#18235,#18236,#18237,#18238,
#18239,#18240,#18241,#18242,#18243,#18244,#18245,#18246,#18247,#18248));
#18606=CLOSED_SHELL('',(#18249,#18250,#18251,#18252,#18253,#18254,#18255,
#18256));
#18607=CLOSED_SHELL('',(#18257,#18258,#18259,#18260,#18261,#18262,#18263,
#18264,#18265,#18266,#18267,#18268,#18269,#18270,#18271,#18272,#18273,#18274,
#18275,#18276,#18277,#18278,#18279,#18280,#18281,#18282,#18283,#18284,#18285,
#18286,#18287));
#18608=CLOSED_SHELL('',(#18288,#18289,#18290,#18291,#18292,#18293,#18294,
#18295));
#18609=CLOSED_SHELL('',(#18296,#18297,#18298,#18299,#18300,#18301,#18302,
#18303,#18304,#18305));
#18610=CLOSED_SHELL('',(#18306,#18307,#18308,#18309,#18310,#18311,#18312,
#18313,#18314));
#18611=CLOSED_SHELL('',(#18315,#18316,#18317,#18318,#18319,#18320,#18321,
#18322));
#18612=CLOSED_SHELL('',(#18323,#18324,#18325,#18326,#18327,#18328,#18329,
#18330,#18331,#18332,#18333,#18334,#18335,#18336,#18337,#18338,#18339,#18340,
#18341,#18342,#18343,#18344,#18345,#18346,#18347,#18348,#18349,#18350,#18351,
#18352,#18353,#18354,#18355,#18356,#18357,#18358,#18359,#18360,#18361,#18362,
#18363,#18364,#18365,#18366,#18367,#18368,#18369,#18370,#18371,#18372,#18373,
#18374,#18375,#18376,#18377,#18378,#18379,#18380,#18381,#18382,#18383,#18384,
#18385,#18386,#18387,#18388,#18389,#18390,#18391,#18392,#18393,#18394,#18395,
#18396,#18397,#18398,#18399,#18400,#18401,#18402,#18403,#18404,#18405,#18406,
#18407,#18408,#18409,#18410,#18411,#18412,#18413,#18414,#18415,#18416,#18417,
#18418,#18419,#18420,#18421,#18422,#18423,#18424,#18425,#18426,#18427,#18428,
#18429,#18430,#18431,#18432,#18433,#18434,#18435,#18436,#18437,#18438,#18439,
#18440,#18441,#18442,#18443,#18444,#18445,#18446,#18447,#18448,#18449,#18450,
#18451,#18452,#18453,#18454,#18455,#18456,#18457,#18458,#18459,#18460,#18461,
#18462,#18463,#18464,#18465));
#18613=CLOSED_SHELL('',(#18466,#18467,#18468,#18469));
#18614=CLOSED_SHELL('',(#18470,#18471,#18472,#18473,#18474,#18475,#18476));
#18615=CLOSED_SHELL('',(#18477,#18478,#18479,#18480,#18481,#18482,#18483,
#18484,#18485,#18486,#18487,#18488,#18489));
#18616=CLOSED_SHELL('',(#18490,#18491,#18492,#18493));
#18617=CLOSED_SHELL('',(#18494,#18495,#18496,#18497));
#18618=CLOSED_SHELL('',(#18498,#18499,#18500,#18501,#18502,#18503,#18504,
#18505,#18506,#18507));
#18619=CLOSED_SHELL('',(#18508,#18509,#18510,#18511,#18512,#18513,#18514,
#18515,#18516,#18517,#18518,#18519));
#18620=CLOSED_SHELL('',(#18520,#18521,#18522,#18523));
#18621=CLOSED_SHELL('',(#18524,#18525,#18526,#18527,#18528,#18529,#18530,
#18531,#18532));
#18622=CLOSED_SHELL('',(#18533,#18534,#18535,#18536,#18537,#18538,#18539,
#18540));
#18623=DERIVED_UNIT_ELEMENT(#18743,1.);
#18624=DERIVED_UNIT_ELEMENT(#43523,-3.);
#18625=DERIVED_UNIT_ELEMENT(#18743,1.);
#18626=DERIVED_UNIT_ELEMENT(#43523,-3.);
#18627=DERIVED_UNIT_ELEMENT(#18743,1.);
#18628=DERIVED_UNIT_ELEMENT(#43523,-3.);
#18629=DERIVED_UNIT_ELEMENT(#18743,1.);
#18630=DERIVED_UNIT_ELEMENT(#43523,-3.);
#18631=DERIVED_UNIT_ELEMENT(#18743,1.);
#18632=DERIVED_UNIT_ELEMENT(#43523,-3.);
#18633=DERIVED_UNIT_ELEMENT(#18743,1.);
#18634=DERIVED_UNIT_ELEMENT(#43523,-3.);
#18635=DERIVED_UNIT_ELEMENT(#18743,1.);
#18636=DERIVED_UNIT_ELEMENT(#43523,-3.);
#18637=DERIVED_UNIT_ELEMENT(#18743,1.);
#18638=DERIVED_UNIT_ELEMENT(#43523,-3.);
#18639=DERIVED_UNIT_ELEMENT(#18743,1.);
#18640=DERIVED_UNIT_ELEMENT(#43523,-3.);
#18641=DERIVED_UNIT_ELEMENT(#18743,1.);
#18642=DERIVED_UNIT_ELEMENT(#43523,-3.);
#18643=DERIVED_UNIT_ELEMENT(#18743,1.);
#18644=DERIVED_UNIT_ELEMENT(#43523,-3.);
#18645=DERIVED_UNIT_ELEMENT(#18743,1.);
#18646=DERIVED_UNIT_ELEMENT(#43523,-3.);
#18647=DERIVED_UNIT_ELEMENT(#18743,1.);
#18648=DERIVED_UNIT_ELEMENT(#43523,-3.);
#18649=DERIVED_UNIT_ELEMENT(#18743,1.);
#18650=DERIVED_UNIT_ELEMENT(#43523,-3.);
#18651=DERIVED_UNIT_ELEMENT(#18743,1.);
#18652=DERIVED_UNIT_ELEMENT(#43523,-3.);
#18653=DERIVED_UNIT_ELEMENT(#18743,1.);
#18654=DERIVED_UNIT_ELEMENT(#43523,-3.);
#18655=DERIVED_UNIT_ELEMENT(#18743,1.);
#18656=DERIVED_UNIT_ELEMENT(#43523,-3.);
#18657=DERIVED_UNIT_ELEMENT(#18743,1.);
#18658=DERIVED_UNIT_ELEMENT(#43523,-3.);
#18659=DERIVED_UNIT_ELEMENT(#18743,1.);
#18660=DERIVED_UNIT_ELEMENT(#43523,-3.);
#18661=DERIVED_UNIT_ELEMENT(#18743,1.);
#18662=DERIVED_UNIT_ELEMENT(#43523,-3.);
#18663=DERIVED_UNIT_ELEMENT(#18743,1.);
#18664=DERIVED_UNIT_ELEMENT(#43523,-3.);
#18665=DERIVED_UNIT_ELEMENT(#18743,1.);
#18666=DERIVED_UNIT_ELEMENT(#43523,-3.);
#18667=DERIVED_UNIT_ELEMENT(#18743,1.);
#18668=DERIVED_UNIT_ELEMENT(#43523,-3.);
#18669=DERIVED_UNIT_ELEMENT(#18743,1.);
#18670=DERIVED_UNIT_ELEMENT(#43523,-3.);
#18671=DERIVED_UNIT_ELEMENT(#18743,1.);
#18672=DERIVED_UNIT_ELEMENT(#43523,-3.);
#18673=DERIVED_UNIT_ELEMENT(#18743,1.);
#18674=DERIVED_UNIT_ELEMENT(#43523,-3.);
#18675=DERIVED_UNIT_ELEMENT(#18743,1.);
#18676=DERIVED_UNIT_ELEMENT(#43523,-3.);
#18677=DERIVED_UNIT_ELEMENT(#18743,1.);
#18678=DERIVED_UNIT_ELEMENT(#43523,-3.);
#18679=DERIVED_UNIT_ELEMENT(#18743,1.);
#18680=DERIVED_UNIT_ELEMENT(#43523,-3.);
#18681=DERIVED_UNIT_ELEMENT(#18743,1.);
#18682=DERIVED_UNIT_ELEMENT(#43523,-3.);
#18683=DERIVED_UNIT_ELEMENT(#18743,1.);
#18684=DERIVED_UNIT_ELEMENT(#43523,-3.);
#18685=DERIVED_UNIT_ELEMENT(#18743,1.);
#18686=DERIVED_UNIT_ELEMENT(#43523,-3.);
#18687=DERIVED_UNIT_ELEMENT(#18743,1.);
#18688=DERIVED_UNIT_ELEMENT(#43523,-3.);
#18689=DERIVED_UNIT_ELEMENT(#18743,1.);
#18690=DERIVED_UNIT_ELEMENT(#43523,-3.);
#18691=DERIVED_UNIT_ELEMENT(#18743,1.);
#18692=DERIVED_UNIT_ELEMENT(#43523,-3.);
#18693=DERIVED_UNIT_ELEMENT(#18743,1.);
#18694=DERIVED_UNIT_ELEMENT(#43523,-3.);
#18695=DERIVED_UNIT_ELEMENT(#18743,1.);
#18696=DERIVED_UNIT_ELEMENT(#43523,-3.);
#18697=DERIVED_UNIT_ELEMENT(#18743,1.);
#18698=DERIVED_UNIT_ELEMENT(#43523,-3.);
#18699=DERIVED_UNIT_ELEMENT(#18743,1.);
#18700=DERIVED_UNIT_ELEMENT(#43523,-3.);
#18701=DERIVED_UNIT_ELEMENT(#18743,1.);
#18702=DERIVED_UNIT_ELEMENT(#43523,-3.);
#18703=DERIVED_UNIT_ELEMENT(#18743,1.);
#18704=DERIVED_UNIT_ELEMENT(#43523,-3.);
#18705=DERIVED_UNIT_ELEMENT(#18743,1.);
#18706=DERIVED_UNIT_ELEMENT(#43523,-3.);
#18707=DERIVED_UNIT_ELEMENT(#18743,1.);
#18708=DERIVED_UNIT_ELEMENT(#43523,-3.);
#18709=DERIVED_UNIT_ELEMENT(#18743,1.);
#18710=DERIVED_UNIT_ELEMENT(#43523,-3.);
#18711=DERIVED_UNIT_ELEMENT(#18743,1.);
#18712=DERIVED_UNIT_ELEMENT(#43523,-3.);
#18713=DERIVED_UNIT_ELEMENT(#18743,1.);
#18714=DERIVED_UNIT_ELEMENT(#43523,-3.);
#18715=DERIVED_UNIT_ELEMENT(#18743,1.);
#18716=DERIVED_UNIT_ELEMENT(#43523,-3.);
#18717=DERIVED_UNIT_ELEMENT(#18743,1.);
#18718=DERIVED_UNIT_ELEMENT(#43523,-3.);
#18719=DERIVED_UNIT_ELEMENT(#18743,1.);
#18720=DERIVED_UNIT_ELEMENT(#43523,-3.);
#18721=DERIVED_UNIT_ELEMENT(#18743,1.);
#18722=DERIVED_UNIT_ELEMENT(#43523,-3.);
#18723=DERIVED_UNIT_ELEMENT(#18743,1.);
#18724=DERIVED_UNIT_ELEMENT(#43523,-3.);
#18725=DERIVED_UNIT_ELEMENT(#18743,1.);
#18726=DERIVED_UNIT_ELEMENT(#43523,-3.);
#18727=DERIVED_UNIT_ELEMENT(#18743,1.);
#18728=DERIVED_UNIT_ELEMENT(#43523,-3.);
#18729=DERIVED_UNIT_ELEMENT(#18743,1.);
#18730=DERIVED_UNIT_ELEMENT(#43523,-3.);
#18731=DERIVED_UNIT_ELEMENT(#18743,1.);
#18732=DERIVED_UNIT_ELEMENT(#43523,-3.);
#18733=DERIVED_UNIT_ELEMENT(#18743,1.);
#18734=DERIVED_UNIT_ELEMENT(#43523,-3.);
#18735=DERIVED_UNIT_ELEMENT(#18743,1.);
#18736=DERIVED_UNIT_ELEMENT(#43523,-3.);
#18737=DERIVED_UNIT_ELEMENT(#18743,1.);
#18738=DERIVED_UNIT_ELEMENT(#43523,-3.);
#18739=DERIVED_UNIT_ELEMENT(#18743,1.);
#18740=DERIVED_UNIT_ELEMENT(#43523,-3.);
#18741=DERIVED_UNIT_ELEMENT(#18743,1.);
#18742=DERIVED_UNIT_ELEMENT(#43523,-3.);
#18743=(
MASS_UNIT()
NAMED_UNIT(*)
SI_UNIT(.KILO.,.GRAM.)
);
#18744=DERIVED_UNIT((#18623,#18624));
#18745=DERIVED_UNIT((#18625,#18626));
#18746=DERIVED_UNIT((#18627,#18628));
#18747=DERIVED_UNIT((#18629,#18630));
#18748=DERIVED_UNIT((#18631,#18632));
#18749=DERIVED_UNIT((#18633,#18634));
#18750=DERIVED_UNIT((#18635,#18636));
#18751=DERIVED_UNIT((#18637,#18638));
#18752=DERIVED_UNIT((#18639,#18640));
#18753=DERIVED_UNIT((#18641,#18642));
#18754=DERIVED_UNIT((#18643,#18644));
#18755=DERIVED_UNIT((#18645,#18646));
#18756=DERIVED_UNIT((#18647,#18648));
#18757=DERIVED_UNIT((#18649,#18650));
#18758=DERIVED_UNIT((#18651,#18652));
#18759=DERIVED_UNIT((#18653,#18654));
#18760=DERIVED_UNIT((#18655,#18656));
#18761=DERIVED_UNIT((#18657,#18658));
#18762=DERIVED_UNIT((#18659,#18660));
#18763=DERIVED_UNIT((#18661,#18662));
#18764=DERIVED_UNIT((#18663,#18664));
#18765=DERIVED_UNIT((#18665,#18666));
#18766=DERIVED_UNIT((#18667,#18668));
#18767=DERIVED_UNIT((#18669,#18670));
#18768=DERIVED_UNIT((#18671,#18672));
#18769=DERIVED_UNIT((#18673,#18674));
#18770=DERIVED_UNIT((#18675,#18676));
#18771=DERIVED_UNIT((#18677,#18678));
#18772=DERIVED_UNIT((#18679,#18680));
#18773=DERIVED_UNIT((#18681,#18682));
#18774=DERIVED_UNIT((#18683,#18684));
#18775=DERIVED_UNIT((#18685,#18686));
#18776=DERIVED_UNIT((#18687,#18688));
#18777=DERIVED_UNIT((#18689,#18690));
#18778=DERIVED_UNIT((#18691,#18692));
#18779=DERIVED_UNIT((#18693,#18694));
#18780=DERIVED_UNIT((#18695,#18696));
#18781=DERIVED_UNIT((#18697,#18698));
#18782=DERIVED_UNIT((#18699,#18700));
#18783=DERIVED_UNIT((#18701,#18702));
#18784=DERIVED_UNIT((#18703,#18704));
#18785=DERIVED_UNIT((#18705,#18706));
#18786=DERIVED_UNIT((#18707,#18708));
#18787=DERIVED_UNIT((#18709,#18710));
#18788=DERIVED_UNIT((#18711,#18712));
#18789=DERIVED_UNIT((#18713,#18714));
#18790=DERIVED_UNIT((#18715,#18716));
#18791=DERIVED_UNIT((#18717,#18718));
#18792=DERIVED_UNIT((#18719,#18720));
#18793=DERIVED_UNIT((#18721,#18722));
#18794=DERIVED_UNIT((#18723,#18724));
#18795=DERIVED_UNIT((#18725,#18726));
#18796=DERIVED_UNIT((#18727,#18728));
#18797=DERIVED_UNIT((#18729,#18730));
#18798=DERIVED_UNIT((#18731,#18732));
#18799=DERIVED_UNIT((#18733,#18734));
#18800=DERIVED_UNIT((#18735,#18736));
#18801=DERIVED_UNIT((#18737,#18738));
#18802=DERIVED_UNIT((#18739,#18740));
#18803=DERIVED_UNIT((#18741,#18742));
#18804=MEASURE_REPRESENTATION_ITEM('density measure',
POSITIVE_RATIO_MEASURE(7850.),#18744);
#18805=MEASURE_REPRESENTATION_ITEM('density measure',
POSITIVE_RATIO_MEASURE(7850.),#18745);
#18806=MEASURE_REPRESENTATION_ITEM('density measure',
POSITIVE_RATIO_MEASURE(7850.),#18746);
#18807=MEASURE_REPRESENTATION_ITEM('density measure',
POSITIVE_RATIO_MEASURE(7850.),#18747);
#18808=MEASURE_REPRESENTATION_ITEM('density measure',
POSITIVE_RATIO_MEASURE(7850.),#18748);
#18809=MEASURE_REPRESENTATION_ITEM('density measure',
POSITIVE_RATIO_MEASURE(7850.),#18749);
#18810=MEASURE_REPRESENTATION_ITEM('density measure',
POSITIVE_RATIO_MEASURE(7850.),#18750);
#18811=MEASURE_REPRESENTATION_ITEM('density measure',
POSITIVE_RATIO_MEASURE(7850.),#18751);
#18812=MEASURE_REPRESENTATION_ITEM('density measure',
POSITIVE_RATIO_MEASURE(7850.),#18752);
#18813=MEASURE_REPRESENTATION_ITEM('density measure',
POSITIVE_RATIO_MEASURE(7850.),#18753);
#18814=MEASURE_REPRESENTATION_ITEM('density measure',
POSITIVE_RATIO_MEASURE(7850.),#18754);
#18815=MEASURE_REPRESENTATION_ITEM('density measure',
POSITIVE_RATIO_MEASURE(7850.),#18755);
#18816=MEASURE_REPRESENTATION_ITEM('density measure',
POSITIVE_RATIO_MEASURE(7850.),#18756);
#18817=MEASURE_REPRESENTATION_ITEM('density measure',
POSITIVE_RATIO_MEASURE(7850.),#18757);
#18818=MEASURE_REPRESENTATION_ITEM('density measure',
POSITIVE_RATIO_MEASURE(7850.),#18758);
#18819=MEASURE_REPRESENTATION_ITEM('density measure',
POSITIVE_RATIO_MEASURE(7850.),#18759);
#18820=MEASURE_REPRESENTATION_ITEM('density measure',
POSITIVE_RATIO_MEASURE(7850.),#18760);
#18821=MEASURE_REPRESENTATION_ITEM('density measure',
POSITIVE_RATIO_MEASURE(7850.),#18761);
#18822=MEASURE_REPRESENTATION_ITEM('density measure',
POSITIVE_RATIO_MEASURE(7850.),#18762);
#18823=MEASURE_REPRESENTATION_ITEM('density measure',
POSITIVE_RATIO_MEASURE(7850.),#18763);
#18824=MEASURE_REPRESENTATION_ITEM('density measure',
POSITIVE_RATIO_MEASURE(7850.),#18764);
#18825=MEASURE_REPRESENTATION_ITEM('density measure',
POSITIVE_RATIO_MEASURE(7850.),#18765);
#18826=MEASURE_REPRESENTATION_ITEM('density measure',
POSITIVE_RATIO_MEASURE(7850.),#18766);
#18827=MEASURE_REPRESENTATION_ITEM('density measure',
POSITIVE_RATIO_MEASURE(7850.),#18767);
#18828=MEASURE_REPRESENTATION_ITEM('density measure',
POSITIVE_RATIO_MEASURE(7850.),#18768);
#18829=MEASURE_REPRESENTATION_ITEM('density measure',
POSITIVE_RATIO_MEASURE(7850.),#18769);
#18830=MEASURE_REPRESENTATION_ITEM('density measure',
POSITIVE_RATIO_MEASURE(7850.),#18770);
#18831=MEASURE_REPRESENTATION_ITEM('density measure',
POSITIVE_RATIO_MEASURE(7850.),#18771);
#18832=MEASURE_REPRESENTATION_ITEM('density measure',
POSITIVE_RATIO_MEASURE(7850.),#18772);
#18833=MEASURE_REPRESENTATION_ITEM('density measure',
POSITIVE_RATIO_MEASURE(7850.),#18773);
#18834=MEASURE_REPRESENTATION_ITEM('density measure',
POSITIVE_RATIO_MEASURE(7850.),#18774);
#18835=MEASURE_REPRESENTATION_ITEM('density measure',
POSITIVE_RATIO_MEASURE(7850.),#18775);
#18836=MEASURE_REPRESENTATION_ITEM('density measure',
POSITIVE_RATIO_MEASURE(7850.),#18776);
#18837=MEASURE_REPRESENTATION_ITEM('density measure',
POSITIVE_RATIO_MEASURE(7850.),#18777);
#18838=MEASURE_REPRESENTATION_ITEM('density measure',
POSITIVE_RATIO_MEASURE(7850.),#18778);
#18839=MEASURE_REPRESENTATION_ITEM('density measure',
POSITIVE_RATIO_MEASURE(7850.),#18779);
#18840=MEASURE_REPRESENTATION_ITEM('density measure',
POSITIVE_RATIO_MEASURE(7850.),#18780);
#18841=MEASURE_REPRESENTATION_ITEM('density measure',
POSITIVE_RATIO_MEASURE(7850.),#18781);
#18842=MEASURE_REPRESENTATION_ITEM('density measure',
POSITIVE_RATIO_MEASURE(7850.),#18782);
#18843=MEASURE_REPRESENTATION_ITEM('density measure',
POSITIVE_RATIO_MEASURE(7850.),#18783);
#18844=MEASURE_REPRESENTATION_ITEM('density measure',
POSITIVE_RATIO_MEASURE(7850.),#18784);
#18845=MEASURE_REPRESENTATION_ITEM('density measure',
POSITIVE_RATIO_MEASURE(7850.),#18785);
#18846=MEASURE_REPRESENTATION_ITEM('density measure',
POSITIVE_RATIO_MEASURE(7850.),#18786);
#18847=MEASURE_REPRESENTATION_ITEM('density measure',
POSITIVE_RATIO_MEASURE(7850.),#18787);
#18848=MEASURE_REPRESENTATION_ITEM('density measure',
POSITIVE_RATIO_MEASURE(7850.),#18788);
#18849=MEASURE_REPRESENTATION_ITEM('density measure',
POSITIVE_RATIO_MEASURE(7850.),#18789);
#18850=MEASURE_REPRESENTATION_ITEM('density measure',
POSITIVE_RATIO_MEASURE(7850.),#18790);
#18851=MEASURE_REPRESENTATION_ITEM('density measure',
POSITIVE_RATIO_MEASURE(7850.),#18791);
#18852=MEASURE_REPRESENTATION_ITEM('density measure',
POSITIVE_RATIO_MEASURE(7850.),#18792);
#18853=MEASURE_REPRESENTATION_ITEM('density measure',
POSITIVE_RATIO_MEASURE(7850.),#18793);
#18854=MEASURE_REPRESENTATION_ITEM('density measure',
POSITIVE_RATIO_MEASURE(7850.),#18794);
#18855=MEASURE_REPRESENTATION_ITEM('density measure',
POSITIVE_RATIO_MEASURE(7850.),#18795);
#18856=MEASURE_REPRESENTATION_ITEM('density measure',
POSITIVE_RATIO_MEASURE(7850.),#18796);
#18857=MEASURE_REPRESENTATION_ITEM('density measure',
POSITIVE_RATIO_MEASURE(7850.),#18797);
#18858=MEASURE_REPRESENTATION_ITEM('density measure',
POSITIVE_RATIO_MEASURE(7850.),#18798);
#18859=MEASURE_REPRESENTATION_ITEM('density measure',
POSITIVE_RATIO_MEASURE(7850.),#18799);
#18860=MEASURE_REPRESENTATION_ITEM('density measure',
POSITIVE_RATIO_MEASURE(7850.),#18800);
#18861=MEASURE_REPRESENTATION_ITEM('density measure',
POSITIVE_RATIO_MEASURE(7850.),#18801);
#18862=MEASURE_REPRESENTATION_ITEM('density measure',
POSITIVE_RATIO_MEASURE(7850.),#18802);
#18863=MEASURE_REPRESENTATION_ITEM('density measure',
POSITIVE_RATIO_MEASURE(7850.),#18803);
#18864=PROPERTY_DEFINITION_REPRESENTATION(#19164,#18984);
#18865=PROPERTY_DEFINITION_REPRESENTATION(#19165,#18985);
#18866=PROPERTY_DEFINITION_REPRESENTATION(#19166,#18986);
#18867=PROPERTY_DEFINITION_REPRESENTATION(#19167,#18987);
#18868=PROPERTY_DEFINITION_REPRESENTATION(#19168,#18988);
#18869=PROPERTY_DEFINITION_REPRESENTATION(#19169,#18989);
#18870=PROPERTY_DEFINITION_REPRESENTATION(#19170,#18990);
#18871=PROPERTY_DEFINITION_REPRESENTATION(#19171,#18991);
#18872=PROPERTY_DEFINITION_REPRESENTATION(#19172,#18992);
#18873=PROPERTY_DEFINITION_REPRESENTATION(#19173,#18993);
#18874=PROPERTY_DEFINITION_REPRESENTATION(#19174,#18994);
#18875=PROPERTY_DEFINITION_REPRESENTATION(#19175,#18995);
#18876=PROPERTY_DEFINITION_REPRESENTATION(#19176,#18996);
#18877=PROPERTY_DEFINITION_REPRESENTATION(#19177,#18997);
#18878=PROPERTY_DEFINITION_REPRESENTATION(#19178,#18998);
#18879=PROPERTY_DEFINITION_REPRESENTATION(#19179,#18999);
#18880=PROPERTY_DEFINITION_REPRESENTATION(#19180,#19000);
#18881=PROPERTY_DEFINITION_REPRESENTATION(#19181,#19001);
#18882=PROPERTY_DEFINITION_REPRESENTATION(#19182,#19002);
#18883=PROPERTY_DEFINITION_REPRESENTATION(#19183,#19003);
#18884=PROPERTY_DEFINITION_REPRESENTATION(#19184,#19004);
#18885=PROPERTY_DEFINITION_REPRESENTATION(#19185,#19005);
#18886=PROPERTY_DEFINITION_REPRESENTATION(#19186,#19006);
#18887=PROPERTY_DEFINITION_REPRESENTATION(#19187,#19007);
#18888=PROPERTY_DEFINITION_REPRESENTATION(#19188,#19008);
#18889=PROPERTY_DEFINITION_REPRESENTATION(#19189,#19009);
#18890=PROPERTY_DEFINITION_REPRESENTATION(#19190,#19010);
#18891=PROPERTY_DEFINITION_REPRESENTATION(#19191,#19011);
#18892=PROPERTY_DEFINITION_REPRESENTATION(#19192,#19012);
#18893=PROPERTY_DEFINITION_REPRESENTATION(#19193,#19013);
#18894=PROPERTY_DEFINITION_REPRESENTATION(#19194,#19014);
#18895=PROPERTY_DEFINITION_REPRESENTATION(#19195,#19015);
#18896=PROPERTY_DEFINITION_REPRESENTATION(#19196,#19016);
#18897=PROPERTY_DEFINITION_REPRESENTATION(#19197,#19017);
#18898=PROPERTY_DEFINITION_REPRESENTATION(#19198,#19018);
#18899=PROPERTY_DEFINITION_REPRESENTATION(#19199,#19019);
#18900=PROPERTY_DEFINITION_REPRESENTATION(#19200,#19020);
#18901=PROPERTY_DEFINITION_REPRESENTATION(#19201,#19021);
#18902=PROPERTY_DEFINITION_REPRESENTATION(#19202,#19022);
#18903=PROPERTY_DEFINITION_REPRESENTATION(#19203,#19023);
#18904=PROPERTY_DEFINITION_REPRESENTATION(#19204,#19024);
#18905=PROPERTY_DEFINITION_REPRESENTATION(#19205,#19025);
#18906=PROPERTY_DEFINITION_REPRESENTATION(#19206,#19026);
#18907=PROPERTY_DEFINITION_REPRESENTATION(#19207,#19027);
#18908=PROPERTY_DEFINITION_REPRESENTATION(#19208,#19028);
#18909=PROPERTY_DEFINITION_REPRESENTATION(#19209,#19029);
#18910=PROPERTY_DEFINITION_REPRESENTATION(#19210,#19030);
#18911=PROPERTY_DEFINITION_REPRESENTATION(#19211,#19031);
#18912=PROPERTY_DEFINITION_REPRESENTATION(#19212,#19032);
#18913=PROPERTY_DEFINITION_REPRESENTATION(#19213,#19033);
#18914=PROPERTY_DEFINITION_REPRESENTATION(#19214,#19034);
#18915=PROPERTY_DEFINITION_REPRESENTATION(#19215,#19035);
#18916=PROPERTY_DEFINITION_REPRESENTATION(#19216,#19036);
#18917=PROPERTY_DEFINITION_REPRESENTATION(#19217,#19037);
#18918=PROPERTY_DEFINITION_REPRESENTATION(#19218,#19038);
#18919=PROPERTY_DEFINITION_REPRESENTATION(#19219,#19039);
#18920=PROPERTY_DEFINITION_REPRESENTATION(#19220,#19040);
#18921=PROPERTY_DEFINITION_REPRESENTATION(#19221,#19041);
#18922=PROPERTY_DEFINITION_REPRESENTATION(#19222,#19042);
#18923=PROPERTY_DEFINITION_REPRESENTATION(#19223,#19043);
#18924=PROPERTY_DEFINITION_REPRESENTATION(#19224,#19044);
#18925=PROPERTY_DEFINITION_REPRESENTATION(#19225,#19045);
#18926=PROPERTY_DEFINITION_REPRESENTATION(#19226,#19046);
#18927=PROPERTY_DEFINITION_REPRESENTATION(#19227,#19047);
#18928=PROPERTY_DEFINITION_REPRESENTATION(#19228,#19048);
#18929=PROPERTY_DEFINITION_REPRESENTATION(#19229,#19049);
#18930=PROPERTY_DEFINITION_REPRESENTATION(#19230,#19050);
#18931=PROPERTY_DEFINITION_REPRESENTATION(#19231,#19051);
#18932=PROPERTY_DEFINITION_REPRESENTATION(#19232,#19052);
#18933=PROPERTY_DEFINITION_REPRESENTATION(#19233,#19053);
#18934=PROPERTY_DEFINITION_REPRESENTATION(#19234,#19054);
#18935=PROPERTY_DEFINITION_REPRESENTATION(#19235,#19055);
#18936=PROPERTY_DEFINITION_REPRESENTATION(#19236,#19056);
#18937=PROPERTY_DEFINITION_REPRESENTATION(#19237,#19057);
#18938=PROPERTY_DEFINITION_REPRESENTATION(#19238,#19058);
#18939=PROPERTY_DEFINITION_REPRESENTATION(#19239,#19059);
#18940=PROPERTY_DEFINITION_REPRESENTATION(#19240,#19060);
#18941=PROPERTY_DEFINITION_REPRESENTATION(#19241,#19061);
#18942=PROPERTY_DEFINITION_REPRESENTATION(#19242,#19062);
#18943=PROPERTY_DEFINITION_REPRESENTATION(#19243,#19063);
#18944=PROPERTY_DEFINITION_REPRESENTATION(#19244,#19064);
#18945=PROPERTY_DEFINITION_REPRESENTATION(#19245,#19065);
#18946=PROPERTY_DEFINITION_REPRESENTATION(#19246,#19066);
#18947=PROPERTY_DEFINITION_REPRESENTATION(#19247,#19067);
#18948=PROPERTY_DEFINITION_REPRESENTATION(#19248,#19068);
#18949=PROPERTY_DEFINITION_REPRESENTATION(#19249,#19069);
#18950=PROPERTY_DEFINITION_REPRESENTATION(#19250,#19070);
#18951=PROPERTY_DEFINITION_REPRESENTATION(#19251,#19071);
#18952=PROPERTY_DEFINITION_REPRESENTATION(#19252,#19072);
#18953=PROPERTY_DEFINITION_REPRESENTATION(#19253,#19073);
#18954=PROPERTY_DEFINITION_REPRESENTATION(#19254,#19074);
#18955=PROPERTY_DEFINITION_REPRESENTATION(#19255,#19075);
#18956=PROPERTY_DEFINITION_REPRESENTATION(#19256,#19076);
#18957=PROPERTY_DEFINITION_REPRESENTATION(#19257,#19077);
#18958=PROPERTY_DEFINITION_REPRESENTATION(#19258,#19078);
#18959=PROPERTY_DEFINITION_REPRESENTATION(#19259,#19079);
#18960=PROPERTY_DEFINITION_REPRESENTATION(#19260,#19080);
#18961=PROPERTY_DEFINITION_REPRESENTATION(#19261,#19081);
#18962=PROPERTY_DEFINITION_REPRESENTATION(#19262,#19082);
#18963=PROPERTY_DEFINITION_REPRESENTATION(#19263,#19083);
#18964=PROPERTY_DEFINITION_REPRESENTATION(#19264,#19084);
#18965=PROPERTY_DEFINITION_REPRESENTATION(#19265,#19085);
#18966=PROPERTY_DEFINITION_REPRESENTATION(#19266,#19086);
#18967=PROPERTY_DEFINITION_REPRESENTATION(#19267,#19087);
#18968=PROPERTY_DEFINITION_REPRESENTATION(#19268,#19088);
#18969=PROPERTY_DEFINITION_REPRESENTATION(#19269,#19089);
#18970=PROPERTY_DEFINITION_REPRESENTATION(#19270,#19090);
#18971=PROPERTY_DEFINITION_REPRESENTATION(#19271,#19091);
#18972=PROPERTY_DEFINITION_REPRESENTATION(#19272,#19092);
#18973=PROPERTY_DEFINITION_REPRESENTATION(#19273,#19093);
#18974=PROPERTY_DEFINITION_REPRESENTATION(#19274,#19094);
#18975=PROPERTY_DEFINITION_REPRESENTATION(#19275,#19095);
#18976=PROPERTY_DEFINITION_REPRESENTATION(#19276,#19096);
#18977=PROPERTY_DEFINITION_REPRESENTATION(#19277,#19097);
#18978=PROPERTY_DEFINITION_REPRESENTATION(#19278,#19098);
#18979=PROPERTY_DEFINITION_REPRESENTATION(#19279,#19099);
#18980=PROPERTY_DEFINITION_REPRESENTATION(#19280,#19100);
#18981=PROPERTY_DEFINITION_REPRESENTATION(#19281,#19101);
#18982=PROPERTY_DEFINITION_REPRESENTATION(#19282,#19102);
#18983=PROPERTY_DEFINITION_REPRESENTATION(#19283,#19103);
#18984=REPRESENTATION('material name',(#19104),#43456);
#18985=REPRESENTATION('density',(#18804),#43456);
#18986=REPRESENTATION('material name',(#19105),#43457);
#18987=REPRESENTATION('density',(#18805),#43457);
#18988=REPRESENTATION('material name',(#19106),#43458);
#18989=REPRESENTATION('density',(#18806),#43458);
#18990=REPRESENTATION('material name',(#19107),#43459);
#18991=REPRESENTATION('density',(#18807),#43459);
#18992=REPRESENTATION('material name',(#19108),#43460);
#18993=REPRESENTATION('density',(#18808),#43460);
#18994=REPRESENTATION('material name',(#19109),#43461);
#18995=REPRESENTATION('density',(#18809),#43461);
#18996=REPRESENTATION('material name',(#19110),#43462);
#18997=REPRESENTATION('density',(#18810),#43462);
#18998=REPRESENTATION('material name',(#19111),#43463);
#18999=REPRESENTATION('density',(#18811),#43463);
#19000=REPRESENTATION('material name',(#19112),#43464);
#19001=REPRESENTATION('density',(#18812),#43464);
#19002=REPRESENTATION('material name',(#19113),#43465);
#19003=REPRESENTATION('density',(#18813),#43465);
#19004=REPRESENTATION('material name',(#19114),#43466);
#19005=REPRESENTATION('density',(#18814),#43466);
#19006=REPRESENTATION('material name',(#19115),#43467);
#19007=REPRESENTATION('density',(#18815),#43467);
#19008=REPRESENTATION('material name',(#19116),#43468);
#19009=REPRESENTATION('density',(#18816),#43468);
#19010=REPRESENTATION('material name',(#19117),#43469);
#19011=REPRESENTATION('density',(#18817),#43469);
#19012=REPRESENTATION('material name',(#19118),#43470);
#19013=REPRESENTATION('density',(#18818),#43470);
#19014=REPRESENTATION('material name',(#19119),#43471);
#19015=REPRESENTATION('density',(#18819),#43471);
#19016=REPRESENTATION('material name',(#19120),#43472);
#19017=REPRESENTATION('density',(#18820),#43472);
#19018=REPRESENTATION('material name',(#19121),#43473);
#19019=REPRESENTATION('density',(#18821),#43473);
#19020=REPRESENTATION('material name',(#19122),#43474);
#19021=REPRESENTATION('density',(#18822),#43474);
#19022=REPRESENTATION('material name',(#19123),#43475);
#19023=REPRESENTATION('density',(#18823),#43475);
#19024=REPRESENTATION('material name',(#19124),#43476);
#19025=REPRESENTATION('density',(#18824),#43476);
#19026=REPRESENTATION('material name',(#19125),#43477);
#19027=REPRESENTATION('density',(#18825),#43477);
#19028=REPRESENTATION('material name',(#19126),#43478);
#19029=REPRESENTATION('density',(#18826),#43478);
#19030=REPRESENTATION('material name',(#19127),#43480);
#19031=REPRESENTATION('density',(#18827),#43480);
#19032=REPRESENTATION('material name',(#19128),#43481);
#19033=REPRESENTATION('density',(#18828),#43481);
#19034=REPRESENTATION('material name',(#19129),#43482);
#19035=REPRESENTATION('density',(#18829),#43482);
#19036=REPRESENTATION('material name',(#19130),#43483);
#19037=REPRESENTATION('density',(#18830),#43483);
#19038=REPRESENTATION('material name',(#19131),#43484);
#19039=REPRESENTATION('density',(#18831),#43484);
#19040=REPRESENTATION('material name',(#19132),#43486);
#19041=REPRESENTATION('density',(#18832),#43486);
#19042=REPRESENTATION('material name',(#19133),#43487);
#19043=REPRESENTATION('density',(#18833),#43487);
#19044=REPRESENTATION('material name',(#19134),#43488);
#19045=REPRESENTATION('density',(#18834),#43488);
#19046=REPRESENTATION('material name',(#19135),#43489);
#19047=REPRESENTATION('density',(#18835),#43489);
#19048=REPRESENTATION('material name',(#19136),#43490);
#19049=REPRESENTATION('density',(#18836),#43490);
#19050=REPRESENTATION('material name',(#19137),#43491);
#19051=REPRESENTATION('density',(#18837),#43491);
#19052=REPRESENTATION('material name',(#19138),#43492);
#19053=REPRESENTATION('density',(#18838),#43492);
#19054=REPRESENTATION('material name',(#19139),#43493);
#19055=REPRESENTATION('density',(#18839),#43493);
#19056=REPRESENTATION('material name',(#19140),#43494);
#19057=REPRESENTATION('density',(#18840),#43494);
#19058=REPRESENTATION('material name',(#19141),#43495);
#19059=REPRESENTATION('density',(#18841),#43495);
#19060=REPRESENTATION('material name',(#19142),#43496);
#19061=REPRESENTATION('density',(#18842),#43496);
#19062=REPRESENTATION('material name',(#19143),#43498);
#19063=REPRESENTATION('density',(#18843),#43498);
#19064=REPRESENTATION('material name',(#19144),#43499);
#19065=REPRESENTATION('density',(#18844),#43499);
#19066=REPRESENTATION('material name',(#19145),#43500);
#19067=REPRESENTATION('density',(#18845),#43500);
#19068=REPRESENTATION('material name',(#19146),#43501);
#19069=REPRESENTATION('density',(#18846),#43501);
#19070=REPRESENTATION('material name',(#19147),#43502);
#19071=REPRESENTATION('density',(#18847),#43502);
#19072=REPRESENTATION('material name',(#19148),#43503);
#19073=REPRESENTATION('density',(#18848),#43503);
#19074=REPRESENTATION('material name',(#19149),#43505);
#19075=REPRESENTATION('density',(#18849),#43505);
#19076=REPRESENTATION('material name',(#19150),#43506);
#19077=REPRESENTATION('density',(#18850),#43506);
#19078=REPRESENTATION('material name',(#19151),#43507);
#19079=REPRESENTATION('density',(#18851),#43507);
#19080=REPRESENTATION('material name',(#19152),#43508);
#19081=REPRESENTATION('density',(#18852),#43508);
#19082=REPRESENTATION('material name',(#19153),#43509);
#19083=REPRESENTATION('density',(#18853),#43509);
#19084=REPRESENTATION('material name',(#19154),#43511);
#19085=REPRESENTATION('density',(#18854),#43511);
#19086=REPRESENTATION('material name',(#19155),#43512);
#19087=REPRESENTATION('density',(#18855),#43512);
#19088=REPRESENTATION('material name',(#19156),#43513);
#19089=REPRESENTATION('density',(#18856),#43513);
#19090=REPRESENTATION('material name',(#19157),#43514);
#19091=REPRESENTATION('density',(#18857),#43514);
#19092=REPRESENTATION('material name',(#19158),#43515);
#19093=REPRESENTATION('density',(#18858),#43515);
#19094=REPRESENTATION('material name',(#19159),#43516);
#19095=REPRESENTATION('density',(#18859),#43516);
#19096=REPRESENTATION('material name',(#19160),#43517);
#19097=REPRESENTATION('density',(#18860),#43517);
#19098=REPRESENTATION('material name',(#19161),#43518);
#19099=REPRESENTATION('density',(#18861),#43518);
#19100=REPRESENTATION('material name',(#19162),#43519);
#19101=REPRESENTATION('density',(#18862),#43519);
#19102=REPRESENTATION('material name',(#19163),#43520);
#19103=REPRESENTATION('density',(#18863),#43520);
#19104=DESCRIPTIVE_REPRESENTATION_ITEM('Steel','Steel');
#19105=DESCRIPTIVE_REPRESENTATION_ITEM('Steel','Steel');
#19106=DESCRIPTIVE_REPRESENTATION_ITEM('Steel','Steel');
#19107=DESCRIPTIVE_REPRESENTATION_ITEM('Steel','Steel');
#19108=DESCRIPTIVE_REPRESENTATION_ITEM('Steel','Steel');
#19109=DESCRIPTIVE_REPRESENTATION_ITEM('Steel','Steel');
#19110=DESCRIPTIVE_REPRESENTATION_ITEM('Steel','Steel');
#19111=DESCRIPTIVE_REPRESENTATION_ITEM('Steel','Steel');
#19112=DESCRIPTIVE_REPRESENTATION_ITEM('Steel','Steel');
#19113=DESCRIPTIVE_REPRESENTATION_ITEM('Steel','Steel');
#19114=DESCRIPTIVE_REPRESENTATION_ITEM('Steel','Steel');
#19115=DESCRIPTIVE_REPRESENTATION_ITEM('Steel','Steel');
#19116=DESCRIPTIVE_REPRESENTATION_ITEM('Steel','Steel');
#19117=DESCRIPTIVE_REPRESENTATION_ITEM('Steel','Steel');
#19118=DESCRIPTIVE_REPRESENTATION_ITEM('Steel','Steel');
#19119=DESCRIPTIVE_REPRESENTATION_ITEM('Steel','Steel');
#19120=DESCRIPTIVE_REPRESENTATION_ITEM('Steel','Steel');
#19121=DESCRIPTIVE_REPRESENTATION_ITEM('Steel','Steel');
#19122=DESCRIPTIVE_REPRESENTATION_ITEM('Steel','Steel');
#19123=DESCRIPTIVE_REPRESENTATION_ITEM('Steel','Steel');
#19124=DESCRIPTIVE_REPRESENTATION_ITEM('Steel','Steel');
#19125=DESCRIPTIVE_REPRESENTATION_ITEM('Steel','Steel');
#19126=DESCRIPTIVE_REPRESENTATION_ITEM('Steel','Steel');
#19127=DESCRIPTIVE_REPRESENTATION_ITEM('Steel','Steel');
#19128=DESCRIPTIVE_REPRESENTATION_ITEM('Steel','Steel');
#19129=DESCRIPTIVE_REPRESENTATION_ITEM('Steel','Steel');
#19130=DESCRIPTIVE_REPRESENTATION_ITEM('Steel','Steel');
#19131=DESCRIPTIVE_REPRESENTATION_ITEM('Steel','Steel');
#19132=DESCRIPTIVE_REPRESENTATION_ITEM('Steel','Steel');
#19133=DESCRIPTIVE_REPRESENTATION_ITEM('Steel','Steel');
#19134=DESCRIPTIVE_REPRESENTATION_ITEM('Steel','Steel');
#19135=DESCRIPTIVE_REPRESENTATION_ITEM('Steel','Steel');
#19136=DESCRIPTIVE_REPRESENTATION_ITEM('Steel','Steel');
#19137=DESCRIPTIVE_REPRESENTATION_ITEM('Steel','Steel');
#19138=DESCRIPTIVE_REPRESENTATION_ITEM('Steel','Steel');
#19139=DESCRIPTIVE_REPRESENTATION_ITEM('Steel','Steel');
#19140=DESCRIPTIVE_REPRESENTATION_ITEM('Steel','Steel');
#19141=DESCRIPTIVE_REPRESENTATION_ITEM('Steel','Steel');
#19142=DESCRIPTIVE_REPRESENTATION_ITEM('Steel','Steel');
#19143=DESCRIPTIVE_REPRESENTATION_ITEM('Steel','Steel');
#19144=DESCRIPTIVE_REPRESENTATION_ITEM('Steel','Steel');
#19145=DESCRIPTIVE_REPRESENTATION_ITEM('Steel','Steel');
#19146=DESCRIPTIVE_REPRESENTATION_ITEM('Steel','Steel');
#19147=DESCRIPTIVE_REPRESENTATION_ITEM('Steel','Steel');
#19148=DESCRIPTIVE_REPRESENTATION_ITEM('Steel','Steel');
#19149=DESCRIPTIVE_REPRESENTATION_ITEM('Steel','Steel');
#19150=DESCRIPTIVE_REPRESENTATION_ITEM('Steel','Steel');
#19151=DESCRIPTIVE_REPRESENTATION_ITEM('Steel','Steel');
#19152=DESCRIPTIVE_REPRESENTATION_ITEM('Steel','Steel');
#19153=DESCRIPTIVE_REPRESENTATION_ITEM('Steel','Steel');
#19154=DESCRIPTIVE_REPRESENTATION_ITEM('Steel','Steel');
#19155=DESCRIPTIVE_REPRESENTATION_ITEM('Steel','Steel');
#19156=DESCRIPTIVE_REPRESENTATION_ITEM('Steel','Steel');
#19157=DESCRIPTIVE_REPRESENTATION_ITEM('Steel','Steel');
#19158=DESCRIPTIVE_REPRESENTATION_ITEM('Steel','Steel');
#19159=DESCRIPTIVE_REPRESENTATION_ITEM('Steel','Steel');
#19160=DESCRIPTIVE_REPRESENTATION_ITEM('Steel','Steel');
#19161=DESCRIPTIVE_REPRESENTATION_ITEM('Steel','Steel');
#19162=DESCRIPTIVE_REPRESENTATION_ITEM('Steel','Steel');
#19163=DESCRIPTIVE_REPRESENTATION_ITEM('Steel','Steel');
#19164=PROPERTY_DEFINITION('material property','material name',#43864);
#19165=PROPERTY_DEFINITION('material property','density of part',#43864);
#19166=PROPERTY_DEFINITION('material property','material name',#43865);
#19167=PROPERTY_DEFINITION('material property','density of part',#43865);
#19168=PROPERTY_DEFINITION('material property','material name',#43866);
#19169=PROPERTY_DEFINITION('material property','density of part',#43866);
#19170=PROPERTY_DEFINITION('material property','material name',#43867);
#19171=PROPERTY_DEFINITION('material property','density of part',#43867);
#19172=PROPERTY_DEFINITION('material property','material name',#43868);
#19173=PROPERTY_DEFINITION('material property','density of part',#43868);
#19174=PROPERTY_DEFINITION('material property','material name',#43869);
#19175=PROPERTY_DEFINITION('material property','density of part',#43869);
#19176=PROPERTY_DEFINITION('material property','material name',#43870);
#19177=PROPERTY_DEFINITION('material property','density of part',#43870);
#19178=PROPERTY_DEFINITION('material property','material name',#43871);
#19179=PROPERTY_DEFINITION('material property','density of part',#43871);
#19180=PROPERTY_DEFINITION('material property','material name',#43872);
#19181=PROPERTY_DEFINITION('material property','density of part',#43872);
#19182=PROPERTY_DEFINITION('material property','material name',#43873);
#19183=PROPERTY_DEFINITION('material property','density of part',#43873);
#19184=PROPERTY_DEFINITION('material property','material name',#43874);
#19185=PROPERTY_DEFINITION('material property','density of part',#43874);
#19186=PROPERTY_DEFINITION('material property','material name',#43875);
#19187=PROPERTY_DEFINITION('material property','density of part',#43875);
#19188=PROPERTY_DEFINITION('material property','material name',#43876);
#19189=PROPERTY_DEFINITION('material property','density of part',#43876);
#19190=PROPERTY_DEFINITION('material property','material name',#43877);
#19191=PROPERTY_DEFINITION('material property','density of part',#43877);
#19192=PROPERTY_DEFINITION('material property','material name',#43878);
#19193=PROPERTY_DEFINITION('material property','density of part',#43878);
#19194=PROPERTY_DEFINITION('material property','material name',#43879);
#19195=PROPERTY_DEFINITION('material property','density of part',#43879);
#19196=PROPERTY_DEFINITION('material property','material name',#43880);
#19197=PROPERTY_DEFINITION('material property','density of part',#43880);
#19198=PROPERTY_DEFINITION('material property','material name',#43881);
#19199=PROPERTY_DEFINITION('material property','density of part',#43881);
#19200=PROPERTY_DEFINITION('material property','material name',#43882);
#19201=PROPERTY_DEFINITION('material property','density of part',#43882);
#19202=PROPERTY_DEFINITION('material property','material name',#43883);
#19203=PROPERTY_DEFINITION('material property','density of part',#43883);
#19204=PROPERTY_DEFINITION('material property','material name',#43884);
#19205=PROPERTY_DEFINITION('material property','density of part',#43884);
#19206=PROPERTY_DEFINITION('material property','material name',#43885);
#19207=PROPERTY_DEFINITION('material property','density of part',#43885);
#19208=PROPERTY_DEFINITION('material property','material name',#43886);
#19209=PROPERTY_DEFINITION('material property','density of part',#43886);
#19210=PROPERTY_DEFINITION('material property','material name',#43888);
#19211=PROPERTY_DEFINITION('material property','density of part',#43888);
#19212=PROPERTY_DEFINITION('material property','material name',#43889);
#19213=PROPERTY_DEFINITION('material property','density of part',#43889);
#19214=PROPERTY_DEFINITION('material property','material name',#43890);
#19215=PROPERTY_DEFINITION('material property','density of part',#43890);
#19216=PROPERTY_DEFINITION('material property','material name',#43891);
#19217=PROPERTY_DEFINITION('material property','density of part',#43891);
#19218=PROPERTY_DEFINITION('material property','material name',#43892);
#19219=PROPERTY_DEFINITION('material property','density of part',#43892);
#19220=PROPERTY_DEFINITION('material property','material name',#43894);
#19221=PROPERTY_DEFINITION('material property','density of part',#43894);
#19222=PROPERTY_DEFINITION('material property','material name',#43895);
#19223=PROPERTY_DEFINITION('material property','density of part',#43895);
#19224=PROPERTY_DEFINITION('material property','material name',#43896);
#19225=PROPERTY_DEFINITION('material property','density of part',#43896);
#19226=PROPERTY_DEFINITION('material property','material name',#43897);
#19227=PROPERTY_DEFINITION('material property','density of part',#43897);
#19228=PROPERTY_DEFINITION('material property','material name',#43898);
#19229=PROPERTY_DEFINITION('material property','density of part',#43898);
#19230=PROPERTY_DEFINITION('material property','material name',#43899);
#19231=PROPERTY_DEFINITION('material property','density of part',#43899);
#19232=PROPERTY_DEFINITION('material property','material name',#43900);
#19233=PROPERTY_DEFINITION('material property','density of part',#43900);
#19234=PROPERTY_DEFINITION('material property','material name',#43901);
#19235=PROPERTY_DEFINITION('material property','density of part',#43901);
#19236=PROPERTY_DEFINITION('material property','material name',#43902);
#19237=PROPERTY_DEFINITION('material property','density of part',#43902);
#19238=PROPERTY_DEFINITION('material property','material name',#43903);
#19239=PROPERTY_DEFINITION('material property','density of part',#43903);
#19240=PROPERTY_DEFINITION('material property','material name',#43904);
#19241=PROPERTY_DEFINITION('material property','density of part',#43904);
#19242=PROPERTY_DEFINITION('material property','material name',#43906);
#19243=PROPERTY_DEFINITION('material property','density of part',#43906);
#19244=PROPERTY_DEFINITION('material property','material name',#43907);
#19245=PROPERTY_DEFINITION('material property','density of part',#43907);
#19246=PROPERTY_DEFINITION('material property','material name',#43908);
#19247=PROPERTY_DEFINITION('material property','density of part',#43908);
#19248=PROPERTY_DEFINITION('material property','material name',#43909);
#19249=PROPERTY_DEFINITION('material property','density of part',#43909);
#19250=PROPERTY_DEFINITION('material property','material name',#43910);
#19251=PROPERTY_DEFINITION('material property','density of part',#43910);
#19252=PROPERTY_DEFINITION('material property','material name',#43911);
#19253=PROPERTY_DEFINITION('material property','density of part',#43911);
#19254=PROPERTY_DEFINITION('material property','material name',#43913);
#19255=PROPERTY_DEFINITION('material property','density of part',#43913);
#19256=PROPERTY_DEFINITION('material property','material name',#43914);
#19257=PROPERTY_DEFINITION('material property','density of part',#43914);
#19258=PROPERTY_DEFINITION('material property','material name',#43915);
#19259=PROPERTY_DEFINITION('material property','density of part',#43915);
#19260=PROPERTY_DEFINITION('material property','material name',#43916);
#19261=PROPERTY_DEFINITION('material property','density of part',#43916);
#19262=PROPERTY_DEFINITION('material property','material name',#43917);
#19263=PROPERTY_DEFINITION('material property','density of part',#43917);
#19264=PROPERTY_DEFINITION('material property','material name',#43919);
#19265=PROPERTY_DEFINITION('material property','density of part',#43919);
#19266=PROPERTY_DEFINITION('material property','material name',#43920);
#19267=PROPERTY_DEFINITION('material property','density of part',#43920);
#19268=PROPERTY_DEFINITION('material property','material name',#43921);
#19269=PROPERTY_DEFINITION('material property','density of part',#43921);
#19270=PROPERTY_DEFINITION('material property','material name',#43922);
#19271=PROPERTY_DEFINITION('material property','density of part',#43922);
#19272=PROPERTY_DEFINITION('material property','material name',#43923);
#19273=PROPERTY_DEFINITION('material property','density of part',#43923);
#19274=PROPERTY_DEFINITION('material property','material name',#43924);
#19275=PROPERTY_DEFINITION('material property','density of part',#43924);
#19276=PROPERTY_DEFINITION('material property','material name',#43925);
#19277=PROPERTY_DEFINITION('material property','density of part',#43925);
#19278=PROPERTY_DEFINITION('material property','material name',#43926);
#19279=PROPERTY_DEFINITION('material property','density of part',#43926);
#19280=PROPERTY_DEFINITION('material property','material name',#43927);
#19281=PROPERTY_DEFINITION('material property','density of part',#43927);
#19282=PROPERTY_DEFINITION('material property','material name',#43928);
#19283=PROPERTY_DEFINITION('material property','density of part',#43928);
#19284=AXIS2_PLACEMENT_3D('',#26452,#21196,#21197);
#19285=AXIS2_PLACEMENT_3D('',#26453,#21198,#21199);
#19286=AXIS2_PLACEMENT_3D('',#26454,#21200,#21201);
#19287=AXIS2_PLACEMENT_3D('',#26455,#21202,#21203);
#19288=AXIS2_PLACEMENT_3D('',#26457,#21204,#21205);
#19289=AXIS2_PLACEMENT_3D('',#26460,#21207,#21208);
#19290=AXIS2_PLACEMENT_3D('',#26461,#21209,#21210);
#19291=AXIS2_PLACEMENT_3D('',#26470,#21215,#21216);
#19292=AXIS2_PLACEMENT_3D('',#26476,#21220,#21221);
#19293=AXIS2_PLACEMENT_3D('',#26482,#21225,#21226);
#19294=AXIS2_PLACEMENT_3D('',#26488,#21230,#21231);
#19295=AXIS2_PLACEMENT_3D('',#26494,#21235,#21236);
#19296=AXIS2_PLACEMENT_3D('',#26496,#21237,#21238);
#19297=AXIS2_PLACEMENT_3D('',#26499,#21240,#21241);
#19298=AXIS2_PLACEMENT_3D('',#26500,#21242,#21243);
#19299=AXIS2_PLACEMENT_3D('',#26501,#21244,#21245);
#19300=AXIS2_PLACEMENT_3D('',#26503,#21246,#21247);
#19301=AXIS2_PLACEMENT_3D('',#26506,#21249,#21250);
#19302=AXIS2_PLACEMENT_3D('',#26507,#21251,#21252);
#19303=AXIS2_PLACEMENT_3D('',#26508,#21253,#21254);
#19304=AXIS2_PLACEMENT_3D('',#26510,#21255,#21256);
#19305=AXIS2_PLACEMENT_3D('',#26513,#21258,#21259);
#19306=AXIS2_PLACEMENT_3D('',#26514,#21260,#21261);
#19307=AXIS2_PLACEMENT_3D('',#26515,#21262,#21263);
#19308=AXIS2_PLACEMENT_3D('',#26517,#21264,#21265);
#19309=AXIS2_PLACEMENT_3D('',#26520,#21267,#21268);
#19310=AXIS2_PLACEMENT_3D('',#26521,#21269,#21270);
#19311=AXIS2_PLACEMENT_3D('',#26522,#21271,#21272);
#19312=AXIS2_PLACEMENT_3D('',#26524,#21273,#21274);
#19313=AXIS2_PLACEMENT_3D('',#26527,#21276,#21277);
#19314=AXIS2_PLACEMENT_3D('',#26528,#21278,#21279);
#19315=AXIS2_PLACEMENT_3D('',#26530,#21280,#21281);
#19316=AXIS2_PLACEMENT_3D('',#26533,#21283,#21284);
#19317=AXIS2_PLACEMENT_3D('',#26534,#21285,#21286);
#19318=AXIS2_PLACEMENT_3D('',#26536,#21287,#21288);
#19319=AXIS2_PLACEMENT_3D('',#26539,#21290,#21291);
#19320=AXIS2_PLACEMENT_3D('',#26540,#21292,#21293);
#19321=AXIS2_PLACEMENT_3D('',#26542,#21294,#21295);
#19322=AXIS2_PLACEMENT_3D('',#26545,#21297,#21298);
#19323=AXIS2_PLACEMENT_3D('',#26546,#21299,#21300);
#19324=AXIS2_PLACEMENT_3D('',#26548,#21301,#21302);
#19325=AXIS2_PLACEMENT_3D('',#26551,#21304,#21305);
#19326=AXIS2_PLACEMENT_3D('',#26552,#21306,#21307);
#19327=AXIS2_PLACEMENT_3D('',#26554,#21308,#21309);
#19328=AXIS2_PLACEMENT_3D('',#26557,#21311,#21312);
#19329=AXIS2_PLACEMENT_3D('',#26558,#21313,#21314);
#19330=AXIS2_PLACEMENT_3D('',#26560,#21315,#21316);
#19331=AXIS2_PLACEMENT_3D('',#26563,#21318,#21319);
#19332=AXIS2_PLACEMENT_3D('',#26564,#21320,#21321);
#19333=AXIS2_PLACEMENT_3D('',#26566,#21322,#21323);
#19334=AXIS2_PLACEMENT_3D('',#26569,#21325,#21326);
#19335=AXIS2_PLACEMENT_3D('',#26570,#21327,#21328);
#19336=AXIS2_PLACEMENT_3D('',#26572,#21329,#21330);
#19337=AXIS2_PLACEMENT_3D('',#26575,#21332,#21333);
#19338=AXIS2_PLACEMENT_3D('',#26576,#21334,#21335);
#19339=AXIS2_PLACEMENT_3D('',#26578,#21336,#21337);
#19340=AXIS2_PLACEMENT_3D('',#26581,#21339,#21340);
#19341=AXIS2_PLACEMENT_3D('',#26582,#21341,#21342);
#19342=AXIS2_PLACEMENT_3D('',#26584,#21343,#21344);
#19343=AXIS2_PLACEMENT_3D('',#26587,#21346,#21347);
#19344=AXIS2_PLACEMENT_3D('',#26588,#21348,#21349);
#19345=AXIS2_PLACEMENT_3D('',#26590,#21350,#21351);
#19346=AXIS2_PLACEMENT_3D('',#26593,#21353,#21354);
#19347=AXIS2_PLACEMENT_3D('',#26594,#21355,#21356);
#19348=AXIS2_PLACEMENT_3D('',#26596,#21357,#21358);
#19349=AXIS2_PLACEMENT_3D('',#26599,#21360,#21361);
#19350=AXIS2_PLACEMENT_3D('',#26600,#21362,#21363);
#19351=AXIS2_PLACEMENT_3D('',#26602,#21364,#21365);
#19352=AXIS2_PLACEMENT_3D('',#26605,#21367,#21368);
#19353=AXIS2_PLACEMENT_3D('',#26606,#21369,#21370);
#19354=AXIS2_PLACEMENT_3D('',#26608,#21371,#21372);
#19355=AXIS2_PLACEMENT_3D('',#26611,#21374,#21375);
#19356=AXIS2_PLACEMENT_3D('',#26612,#21376,#21377);
#19357=AXIS2_PLACEMENT_3D('',#26618,#21381,#21382);
#19358=AXIS2_PLACEMENT_3D('',#26624,#21386,#21387);
#19359=AXIS2_PLACEMENT_3D('',#26627,#21390,#21391);
#19360=AXIS2_PLACEMENT_3D('',#26628,#21392,#21393);
#19361=AXIS2_PLACEMENT_3D('',#26629,#21394,#21395);
#19362=AXIS2_PLACEMENT_3D('',#26630,#21396,#21397);
#19363=AXIS2_PLACEMENT_3D('',#26639,#21402,#21403);
#19364=AXIS2_PLACEMENT_3D('',#26645,#21407,#21408);
#19365=AXIS2_PLACEMENT_3D('',#26651,#21412,#21413);
#19366=AXIS2_PLACEMENT_3D('',#26654,#21416,#21417);
#19367=AXIS2_PLACEMENT_3D('',#26655,#21418,#21419);
#19368=AXIS2_PLACEMENT_3D('',#26656,#21420,#21421);
#19369=AXIS2_PLACEMENT_3D('',#26657,#21422,#21423);
#19370=AXIS2_PLACEMENT_3D('',#26666,#21428,#21429);
#19371=AXIS2_PLACEMENT_3D('',#26672,#21433,#21434);
#19372=AXIS2_PLACEMENT_3D('',#26678,#21438,#21439);
#19373=AXIS2_PLACEMENT_3D('',#26681,#21442,#21443);
#19374=AXIS2_PLACEMENT_3D('',#26682,#21444,#21445);
#19375=AXIS2_PLACEMENT_3D('',#26683,#21446,#21447);
#19376=AXIS2_PLACEMENT_3D('',#26684,#21448,#21449);
#19377=AXIS2_PLACEMENT_3D('',#26686,#21450,#21451);
#19378=AXIS2_PLACEMENT_3D('',#26689,#21453,#21454);
#19379=AXIS2_PLACEMENT_3D('',#26690,#21455,#21456);
#19380=AXIS2_PLACEMENT_3D('',#26692,#21457,#21458);
#19381=AXIS2_PLACEMENT_3D('',#26695,#21460,#21461);
#19382=AXIS2_PLACEMENT_3D('',#26696,#21462,#21463);
#19383=AXIS2_PLACEMENT_3D('',#26698,#21464,#21465);
#19384=AXIS2_PLACEMENT_3D('',#26701,#21467,#21468);
#19385=AXIS2_PLACEMENT_3D('',#26702,#21469,#21470);
#19386=AXIS2_PLACEMENT_3D('',#26704,#21471,#21472);
#19387=AXIS2_PLACEMENT_3D('',#26707,#21474,#21475);
#19388=AXIS2_PLACEMENT_3D('',#26708,#21476,#21477);
#19389=AXIS2_PLACEMENT_3D('',#26710,#21478,#21479);
#19390=AXIS2_PLACEMENT_3D('',#26713,#21481,#21482);
#19391=AXIS2_PLACEMENT_3D('',#26714,#21483,#21484);
#19392=AXIS2_PLACEMENT_3D('',#26716,#21485,#21486);
#19393=AXIS2_PLACEMENT_3D('',#26719,#21488,#21489);
#19394=AXIS2_PLACEMENT_3D('',#26720,#21490,#21491);
#19395=AXIS2_PLACEMENT_3D('',#26722,#21492,#21493);
#19396=AXIS2_PLACEMENT_3D('',#26725,#21495,#21496);
#19397=AXIS2_PLACEMENT_3D('',#26726,#21497,#21498);
#19398=AXIS2_PLACEMENT_3D('',#26728,#21499,#21500);
#19399=AXIS2_PLACEMENT_3D('',#26731,#21502,#21503);
#19400=AXIS2_PLACEMENT_3D('',#26732,#21504,#21505);
#19401=AXIS2_PLACEMENT_3D('',#26741,#21510,#21511);
#19402=AXIS2_PLACEMENT_3D('',#26747,#21515,#21516);
#19403=AXIS2_PLACEMENT_3D('',#26753,#21520,#21521);
#19404=AXIS2_PLACEMENT_3D('',#26756,#21524,#21525);
#19405=AXIS2_PLACEMENT_3D('',#26758,#21526,#21527);
#19406=AXIS2_PLACEMENT_3D('',#26761,#21529,#21530);
#19407=AXIS2_PLACEMENT_3D('',#26762,#21531,#21532);
#19408=AXIS2_PLACEMENT_3D('',#26764,#21533,#21534);
#19409=AXIS2_PLACEMENT_3D('',#26767,#21536,#21537);
#19410=AXIS2_PLACEMENT_3D('',#26768,#21538,#21539);
#19411=AXIS2_PLACEMENT_3D('',#26777,#21544,#21545);
#19412=AXIS2_PLACEMENT_3D('',#26783,#21549,#21550);
#19413=AXIS2_PLACEMENT_3D('',#26789,#21554,#21555);
#19414=AXIS2_PLACEMENT_3D('',#26792,#21558,#21559);
#19415=AXIS2_PLACEMENT_3D('',#26793,#21560,#21561);
#19416=AXIS2_PLACEMENT_3D('',#26794,#21562,#21563);
#19417=AXIS2_PLACEMENT_3D('',#26795,#21564,#21565);
#19418=AXIS2_PLACEMENT_3D('',#26797,#21566,#21567);
#19419=AXIS2_PLACEMENT_3D('',#26800,#21569,#21570);
#19420=AXIS2_PLACEMENT_3D('',#26801,#21571,#21572);
#19421=AXIS2_PLACEMENT_3D('',#26803,#21573,#21574);
#19422=AXIS2_PLACEMENT_3D('',#26806,#21576,#21577);
#19423=AXIS2_PLACEMENT_3D('',#26807,#21578,#21579);
#19424=AXIS2_PLACEMENT_3D('',#26809,#21580,#21581);
#19425=AXIS2_PLACEMENT_3D('',#26812,#21583,#21584);
#19426=AXIS2_PLACEMENT_3D('',#26813,#21585,#21586);
#19427=AXIS2_PLACEMENT_3D('',#26814,#21587,#21588);
#19428=AXIS2_PLACEMENT_3D('',#26816,#21589,#21590);
#19429=AXIS2_PLACEMENT_3D('',#26819,#21592,#21593);
#19430=AXIS2_PLACEMENT_3D('',#26820,#21594,#21595);
#19431=AXIS2_PLACEMENT_3D('',#26821,#21596,#21597);
#19432=AXIS2_PLACEMENT_3D('',#26823,#21598,#21599);
#19433=AXIS2_PLACEMENT_3D('',#26826,#21601,#21602);
#19434=AXIS2_PLACEMENT_3D('',#26827,#21603,#21604);
#19435=AXIS2_PLACEMENT_3D('',#26828,#21605,#21606);
#19436=AXIS2_PLACEMENT_3D('',#26830,#21607,#21608);
#19437=AXIS2_PLACEMENT_3D('',#26833,#21610,#21611);
#19438=AXIS2_PLACEMENT_3D('',#26834,#21612,#21613);
#19439=AXIS2_PLACEMENT_3D('',#26835,#21614,#21615);
#19440=AXIS2_PLACEMENT_3D('',#26844,#21620,#21621);
#19441=AXIS2_PLACEMENT_3D('',#26850,#21625,#21626);
#19442=AXIS2_PLACEMENT_3D('',#26856,#21630,#21631);
#19443=AXIS2_PLACEMENT_3D('',#26859,#21634,#21635);
#19444=AXIS2_PLACEMENT_3D('',#26860,#21636,#21637);
#19445=AXIS2_PLACEMENT_3D('',#26861,#21638,#21639);
#19446=AXIS2_PLACEMENT_3D('',#26862,#21640,#21641);
#19447=AXIS2_PLACEMENT_3D('',#26864,#21642,#21643);
#19448=AXIS2_PLACEMENT_3D('',#26867,#21645,#21646);
#19449=AXIS2_PLACEMENT_3D('',#26868,#21647,#21648);
#19450=AXIS2_PLACEMENT_3D('',#26870,#21649,#21650);
#19451=AXIS2_PLACEMENT_3D('',#26873,#21652,#21653);
#19452=AXIS2_PLACEMENT_3D('',#26874,#21654,#21655);
#19453=AXIS2_PLACEMENT_3D('',#26876,#21656,#21657);
#19454=AXIS2_PLACEMENT_3D('',#26879,#21659,#21660);
#19455=AXIS2_PLACEMENT_3D('',#26880,#21661,#21662);
#19456=AXIS2_PLACEMENT_3D('',#26881,#21663,#21664);
#19457=AXIS2_PLACEMENT_3D('',#26883,#21665,#21666);
#19458=AXIS2_PLACEMENT_3D('',#26886,#21668,#21669);
#19459=AXIS2_PLACEMENT_3D('',#26887,#21670,#21671);
#19460=AXIS2_PLACEMENT_3D('',#26888,#21672,#21673);
#19461=AXIS2_PLACEMENT_3D('',#26890,#21674,#21675);
#19462=AXIS2_PLACEMENT_3D('',#26893,#21677,#21678);
#19463=AXIS2_PLACEMENT_3D('',#26894,#21679,#21680);
#19464=AXIS2_PLACEMENT_3D('',#26895,#21681,#21682);
#19465=AXIS2_PLACEMENT_3D('',#26897,#21683,#21684);
#19466=AXIS2_PLACEMENT_3D('',#26900,#21686,#21687);
#19467=AXIS2_PLACEMENT_3D('',#26901,#21688,#21689);
#19468=AXIS2_PLACEMENT_3D('',#26902,#21690,#21691);
#19469=AXIS2_PLACEMENT_3D('',#26911,#21696,#21697);
#19470=AXIS2_PLACEMENT_3D('',#26917,#21701,#21702);
#19471=AXIS2_PLACEMENT_3D('',#26923,#21706,#21707);
#19472=AXIS2_PLACEMENT_3D('',#26926,#21710,#21711);
#19473=AXIS2_PLACEMENT_3D('',#26927,#21712,#21713);
#19474=AXIS2_PLACEMENT_3D('',#26928,#21714,#21715);
#19475=AXIS2_PLACEMENT_3D('',#26929,#21716,#21717);
#19476=AXIS2_PLACEMENT_3D('',#26931,#21718,#21719);
#19477=AXIS2_PLACEMENT_3D('',#26934,#21721,#21722);
#19478=AXIS2_PLACEMENT_3D('',#26935,#21723,#21724);
#19479=AXIS2_PLACEMENT_3D('',#26936,#21725,#21726);
#19480=AXIS2_PLACEMENT_3D('',#26938,#21727,#21728);
#19481=AXIS2_PLACEMENT_3D('',#26941,#21730,#21731);
#19482=AXIS2_PLACEMENT_3D('',#26942,#21732,#21733);
#19483=AXIS2_PLACEMENT_3D('',#26943,#21734,#21735);
#19484=AXIS2_PLACEMENT_3D('',#26945,#21736,#21737);
#19485=AXIS2_PLACEMENT_3D('',#26948,#21739,#21740);
#19486=AXIS2_PLACEMENT_3D('',#26949,#21741,#21742);
#19487=AXIS2_PLACEMENT_3D('',#26951,#21743,#21744);
#19488=AXIS2_PLACEMENT_3D('',#26954,#21746,#21747);
#19489=AXIS2_PLACEMENT_3D('',#26955,#21748,#21749);
#19490=AXIS2_PLACEMENT_3D('',#26964,#21754,#21755);
#19491=AXIS2_PLACEMENT_3D('',#26970,#21759,#21760);
#19492=AXIS2_PLACEMENT_3D('',#26976,#21764,#21765);
#19493=AXIS2_PLACEMENT_3D('',#26979,#21768,#21769);
#19494=AXIS2_PLACEMENT_3D('',#26980,#21770,#21771);
#19495=AXIS2_PLACEMENT_3D('',#26981,#21772,#21773);
#19496=AXIS2_PLACEMENT_3D('',#26982,#21774,#21775);
#19497=AXIS2_PLACEMENT_3D('',#26984,#21776,#21777);
#19498=AXIS2_PLACEMENT_3D('',#26987,#21779,#21780);
#19499=AXIS2_PLACEMENT_3D('',#26988,#21781,#21782);
#19500=AXIS2_PLACEMENT_3D('',#26990,#21783,#21784);
#19501=AXIS2_PLACEMENT_3D('',#26993,#21786,#21787);
#19502=AXIS2_PLACEMENT_3D('',#26994,#21788,#21789);
#19503=AXIS2_PLACEMENT_3D('',#26996,#21790,#21791);
#19504=AXIS2_PLACEMENT_3D('',#27000,#21793,#21794);
#19505=AXIS2_PLACEMENT_3D('',#27004,#21796,#21797);
#19506=AXIS2_PLACEMENT_3D('',#27007,#21799,#21800);
#19507=AXIS2_PLACEMENT_3D('',#27008,#21801,#21802);
#19508=AXIS2_PLACEMENT_3D('',#27010,#21804,#21805);
#19509=AXIS2_PLACEMENT_3D('',#27012,#21806,#21807);
#19510=AXIS2_PLACEMENT_3D('',#27016,#21809,#21810);
#19511=AXIS2_PLACEMENT_3D('',#27020,#21812,#21813);
#19512=AXIS2_PLACEMENT_3D('',#27023,#21815,#21816);
#19513=AXIS2_PLACEMENT_3D('',#27024,#21817,#21818);
#19514=AXIS2_PLACEMENT_3D('',#27026,#21820,#21821);
#19515=AXIS2_PLACEMENT_3D('',#27037,#21828,#21829);
#19516=AXIS2_PLACEMENT_3D('',#27043,#21833,#21834);
#19517=AXIS2_PLACEMENT_3D('',#27049,#21838,#21839);
#19518=AXIS2_PLACEMENT_3D('',#27055,#21843,#21844);
#19519=AXIS2_PLACEMENT_3D('',#27061,#21848,#21849);
#19520=AXIS2_PLACEMENT_3D('',#27064,#21852,#21853);
#19521=AXIS2_PLACEMENT_3D('',#27065,#21854,#21855);
#19522=AXIS2_PLACEMENT_3D('',#27066,#21856,#21857);
#19523=AXIS2_PLACEMENT_3D('',#27067,#21858,#21859);
#19524=AXIS2_PLACEMENT_3D('',#27069,#21860,#21861);
#19525=AXIS2_PLACEMENT_3D('',#27072,#21863,#21864);
#19526=AXIS2_PLACEMENT_3D('',#27073,#21865,#21866);
#19527=AXIS2_PLACEMENT_3D('',#27074,#21867,#21868);
#19528=AXIS2_PLACEMENT_3D('',#27076,#21869,#21870);
#19529=AXIS2_PLACEMENT_3D('',#27079,#21872,#21873);
#19530=AXIS2_PLACEMENT_3D('',#27080,#21874,#21875);
#19531=AXIS2_PLACEMENT_3D('',#27081,#21876,#21877);
#19532=AXIS2_PLACEMENT_3D('',#27083,#21878,#21879);
#19533=AXIS2_PLACEMENT_3D('',#27086,#21881,#21882);
#19534=AXIS2_PLACEMENT_3D('',#27087,#21883,#21884);
#19535=AXIS2_PLACEMENT_3D('',#27089,#21885,#21886);
#19536=AXIS2_PLACEMENT_3D('',#27092,#21888,#21889);
#19537=AXIS2_PLACEMENT_3D('',#27093,#21890,#21891);
#19538=AXIS2_PLACEMENT_3D('',#27102,#21896,#21897);
#19539=AXIS2_PLACEMENT_3D('',#27108,#21901,#21902);
#19540=AXIS2_PLACEMENT_3D('',#27114,#21906,#21907);
#19541=AXIS2_PLACEMENT_3D('',#27117,#21910,#21911);
#19542=AXIS2_PLACEMENT_3D('',#27118,#21912,#21913);
#19543=AXIS2_PLACEMENT_3D('',#27119,#21914,#21915);
#19544=AXIS2_PLACEMENT_3D('',#27120,#21916,#21917);
#19545=AXIS2_PLACEMENT_3D('',#27122,#21918,#21919);
#19546=AXIS2_PLACEMENT_3D('',#27125,#21921,#21922);
#19547=AXIS2_PLACEMENT_3D('',#27126,#21923,#21924);
#19548=AXIS2_PLACEMENT_3D('',#27128,#21925,#21926);
#19549=AXIS2_PLACEMENT_3D('',#27131,#21928,#21929);
#19550=AXIS2_PLACEMENT_3D('',#27132,#21930,#21931);
#19551=AXIS2_PLACEMENT_3D('',#27134,#21932,#21933);
#19552=AXIS2_PLACEMENT_3D('',#27138,#21935,#21936);
#19553=AXIS2_PLACEMENT_3D('',#27142,#21938,#21939);
#19554=AXIS2_PLACEMENT_3D('',#27145,#21941,#21942);
#19555=AXIS2_PLACEMENT_3D('',#27146,#21943,#21944);
#19556=AXIS2_PLACEMENT_3D('',#27148,#21946,#21947);
#19557=AXIS2_PLACEMENT_3D('',#27150,#21948,#21949);
#19558=AXIS2_PLACEMENT_3D('',#27154,#21951,#21952);
#19559=AXIS2_PLACEMENT_3D('',#27158,#21954,#21955);
#19560=AXIS2_PLACEMENT_3D('',#27161,#21957,#21958);
#19561=AXIS2_PLACEMENT_3D('',#27162,#21959,#21960);
#19562=AXIS2_PLACEMENT_3D('',#27164,#21962,#21963);
#19563=AXIS2_PLACEMENT_3D('',#27175,#21970,#21971);
#19564=AXIS2_PLACEMENT_3D('',#27181,#21975,#21976);
#19565=AXIS2_PLACEMENT_3D('',#27187,#21980,#21981);
#19566=AXIS2_PLACEMENT_3D('',#27193,#21985,#21986);
#19567=AXIS2_PLACEMENT_3D('',#27199,#21990,#21991);
#19568=AXIS2_PLACEMENT_3D('',#27202,#21994,#21995);
#19569=AXIS2_PLACEMENT_3D('',#27203,#21996,#21997);
#19570=AXIS2_PLACEMENT_3D('',#27204,#21998,#21999);
#19571=AXIS2_PLACEMENT_3D('',#27205,#22000,#22001);
#19572=AXIS2_PLACEMENT_3D('',#27207,#22002,#22003);
#19573=AXIS2_PLACEMENT_3D('',#27210,#22005,#22006);
#19574=AXIS2_PLACEMENT_3D('',#27211,#22007,#22008);
#19575=AXIS2_PLACEMENT_3D('',#27213,#22009,#22010);
#19576=AXIS2_PLACEMENT_3D('',#27216,#22012,#22013);
#19577=AXIS2_PLACEMENT_3D('',#27217,#22014,#22015);
#19578=AXIS2_PLACEMENT_3D('',#27219,#22016,#22017);
#19579=AXIS2_PLACEMENT_3D('',#27222,#22019,#22020);
#19580=AXIS2_PLACEMENT_3D('',#27223,#22021,#22022);
#19581=AXIS2_PLACEMENT_3D('',#27225,#22023,#22024);
#19582=AXIS2_PLACEMENT_3D('',#27228,#22026,#22027);
#19583=AXIS2_PLACEMENT_3D('',#27229,#22028,#22029);
#19584=AXIS2_PLACEMENT_3D('',#27230,#22030,#22031);
#19585=AXIS2_PLACEMENT_3D('',#27232,#22032,#22033);
#19586=AXIS2_PLACEMENT_3D('',#27235,#22035,#22036);
#19587=AXIS2_PLACEMENT_3D('',#27236,#22037,#22038);
#19588=AXIS2_PLACEMENT_3D('',#27237,#22039,#22040);
#19589=AXIS2_PLACEMENT_3D('',#27239,#22041,#22042);
#19590=AXIS2_PLACEMENT_3D('',#27242,#22044,#22045);
#19591=AXIS2_PLACEMENT_3D('',#27243,#22046,#22047);
#19592=AXIS2_PLACEMENT_3D('',#27244,#22048,#22049);
#19593=AXIS2_PLACEMENT_3D('',#27246,#22050,#22051);
#19594=AXIS2_PLACEMENT_3D('',#27249,#22053,#22054);
#19595=AXIS2_PLACEMENT_3D('',#27250,#22055,#22056);
#19596=AXIS2_PLACEMENT_3D('',#27251,#22057,#22058);
#19597=AXIS2_PLACEMENT_3D('',#27253,#22059,#22060);
#19598=AXIS2_PLACEMENT_3D('',#27256,#22062,#22063);
#19599=AXIS2_PLACEMENT_3D('',#27257,#22064,#22065);
#19600=AXIS2_PLACEMENT_3D('',#27259,#22066,#22067);
#19601=AXIS2_PLACEMENT_3D('',#27260,#22068,#22069);
#19602=AXIS2_PLACEMENT_3D('',#27263,#22071,#22072);
#19603=AXIS2_PLACEMENT_3D('',#27264,#22073,#22074);
#19604=AXIS2_PLACEMENT_3D('',#27266,#22075,#22076);
#19605=AXIS2_PLACEMENT_3D('',#27269,#22078,#22079);
#19606=AXIS2_PLACEMENT_3D('',#27270,#22080,#22081);
#19607=AXIS2_PLACEMENT_3D('',#27271,#22082,#22083);
#19608=AXIS2_PLACEMENT_3D('',#27280,#22088,#22089);
#19609=AXIS2_PLACEMENT_3D('',#27286,#22093,#22094);
#19610=AXIS2_PLACEMENT_3D('',#27292,#22098,#22099);
#19611=AXIS2_PLACEMENT_3D('',#27295,#22102,#22103);
#19612=AXIS2_PLACEMENT_3D('',#27296,#22104,#22105);
#19613=AXIS2_PLACEMENT_3D('',#27297,#22106,#22107);
#19614=AXIS2_PLACEMENT_3D('',#27298,#22108,#22109);
#19615=AXIS2_PLACEMENT_3D('',#27300,#22110,#22111);
#19616=AXIS2_PLACEMENT_3D('',#27303,#22113,#22114);
#19617=AXIS2_PLACEMENT_3D('',#27304,#22115,#22116);
#19618=AXIS2_PLACEMENT_3D('',#27306,#22117,#22118);
#19619=AXIS2_PLACEMENT_3D('',#27309,#22120,#22121);
#19620=AXIS2_PLACEMENT_3D('',#27310,#22122,#22123);
#19621=AXIS2_PLACEMENT_3D('',#27312,#22124,#22125);
#19622=AXIS2_PLACEMENT_3D('',#27315,#22127,#22128);
#19623=AXIS2_PLACEMENT_3D('',#27316,#22129,#22130);
#19624=AXIS2_PLACEMENT_3D('',#27318,#22131,#22132);
#19625=AXIS2_PLACEMENT_3D('',#27321,#22134,#22135);
#19626=AXIS2_PLACEMENT_3D('',#27322,#22136,#22137);
#19627=AXIS2_PLACEMENT_3D('',#27324,#22138,#22139);
#19628=AXIS2_PLACEMENT_3D('',#27327,#22141,#22142);
#19629=AXIS2_PLACEMENT_3D('',#27328,#22143,#22144);
#19630=AXIS2_PLACEMENT_3D('',#27330,#22145,#22146);
#19631=AXIS2_PLACEMENT_3D('',#27333,#22148,#22149);
#19632=AXIS2_PLACEMENT_3D('',#27334,#22150,#22151);
#19633=AXIS2_PLACEMENT_3D('',#27335,#22152,#22153);
#19634=AXIS2_PLACEMENT_3D('',#27337,#22154,#22155);
#19635=AXIS2_PLACEMENT_3D('',#27340,#22157,#22158);
#19636=AXIS2_PLACEMENT_3D('',#27341,#22159,#22160);
#19637=AXIS2_PLACEMENT_3D('',#27342,#22161,#22162);
#19638=AXIS2_PLACEMENT_3D('',#27344,#22163,#22164);
#19639=AXIS2_PLACEMENT_3D('',#27347,#22166,#22167);
#19640=AXIS2_PLACEMENT_3D('',#27348,#22168,#22169);
#19641=AXIS2_PLACEMENT_3D('',#27349,#22170,#22171);
#19642=AXIS2_PLACEMENT_3D('',#27351,#22172,#22173);
#19643=AXIS2_PLACEMENT_3D('',#27354,#22175,#22176);
#19644=AXIS2_PLACEMENT_3D('',#27355,#22177,#22178);
#19645=AXIS2_PLACEMENT_3D('',#27356,#22179,#22180);
#19646=AXIS2_PLACEMENT_3D('',#27358,#22181,#22182);
#19647=AXIS2_PLACEMENT_3D('',#27361,#22184,#22185);
#19648=AXIS2_PLACEMENT_3D('',#27362,#22186,#22187);
#19649=AXIS2_PLACEMENT_3D('',#27364,#22188,#22189);
#19650=AXIS2_PLACEMENT_3D('',#27365,#22190,#22191);
#19651=AXIS2_PLACEMENT_3D('',#27367,#22192,#22193);
#19652=AXIS2_PLACEMENT_3D('',#27369,#22195,#22196);
#19653=AXIS2_PLACEMENT_3D('',#27374,#22198,#22199);
#19654=AXIS2_PLACEMENT_3D('',#27377,#22201,#22202);
#19655=AXIS2_PLACEMENT_3D('',#27378,#22203,#22204);
#19656=AXIS2_PLACEMENT_3D('',#27383,#22206,#22207);
#19657=AXIS2_PLACEMENT_3D('',#27386,#22209,#22210);
#19658=AXIS2_PLACEMENT_3D('',#27387,#22211,#22212);
#19659=AXIS2_PLACEMENT_3D('',#27393,#22216,#22217);
#19660=AXIS2_PLACEMENT_3D('',#27398,#22221,#22222);
#19661=AXIS2_PLACEMENT_3D('',#27400,#22224,#22225);
#19662=AXIS2_PLACEMENT_3D('',#27404,#22228,#22229);
#19663=AXIS2_PLACEMENT_3D('',#27406,#22231,#22232);
#19664=AXIS2_PLACEMENT_3D('',#27407,#22233,#22234);
#19665=AXIS2_PLACEMENT_3D('',#27408,#22235,#22236);
#19666=AXIS2_PLACEMENT_3D('',#27410,#22237,#22238);
#19667=AXIS2_PLACEMENT_3D('',#27413,#22240,#22241);
#19668=AXIS2_PLACEMENT_3D('',#27414,#22242,#22243);
#19669=AXIS2_PLACEMENT_3D('',#27416,#22244,#22245);
#19670=AXIS2_PLACEMENT_3D('',#27419,#22247,#22248);
#19671=AXIS2_PLACEMENT_3D('',#27420,#22249,#22250);
#19672=AXIS2_PLACEMENT_3D('',#27422,#22251,#22252);
#19673=AXIS2_PLACEMENT_3D('',#27425,#22254,#22255);
#19674=AXIS2_PLACEMENT_3D('',#27426,#22256,#22257);
#19675=AXIS2_PLACEMENT_3D('',#27428,#22258,#22259);
#19676=AXIS2_PLACEMENT_3D('',#27431,#22261,#22262);
#19677=AXIS2_PLACEMENT_3D('',#27432,#22263,#22264);
#19678=AXIS2_PLACEMENT_3D('',#27434,#22265,#22266);
#19679=AXIS2_PLACEMENT_3D('',#27435,#22267,#22268);
#19680=AXIS2_PLACEMENT_3D('',#27438,#22270,#22271);
#19681=AXIS2_PLACEMENT_3D('',#27439,#22272,#22273);
#19682=AXIS2_PLACEMENT_3D('',#27441,#22274,#22275);
#19683=AXIS2_PLACEMENT_3D('',#27444,#22277,#22278);
#19684=AXIS2_PLACEMENT_3D('',#27445,#22279,#22280);
#19685=AXIS2_PLACEMENT_3D('',#27446,#22281,#22282);
#19686=AXIS2_PLACEMENT_3D('',#27447,#22283,#22284);
#19687=AXIS2_PLACEMENT_3D('',#27448,#22285,#22286);
#19688=AXIS2_PLACEMENT_3D('',#27450,#22287,#22288);
#19689=AXIS2_PLACEMENT_3D('',#27453,#22290,#22291);
#19690=AXIS2_PLACEMENT_3D('',#27454,#22292,#22293);
#19691=AXIS2_PLACEMENT_3D('',#27456,#22294,#22295);
#19692=AXIS2_PLACEMENT_3D('',#27459,#22297,#22298);
#19693=AXIS2_PLACEMENT_3D('',#27460,#22299,#22300);
#19694=AXIS2_PLACEMENT_3D('',#27462,#22301,#22302);
#19695=AXIS2_PLACEMENT_3D('',#27465,#22304,#22305);
#19696=AXIS2_PLACEMENT_3D('',#27466,#22306,#22307);
#19697=AXIS2_PLACEMENT_3D('',#27468,#22308,#22309);
#19698=AXIS2_PLACEMENT_3D('',#27471,#22311,#22312);
#19699=AXIS2_PLACEMENT_3D('',#27472,#22313,#22314);
#19700=AXIS2_PLACEMENT_3D('',#27474,#22315,#22316);
#19701=AXIS2_PLACEMENT_3D('',#27475,#22317,#22318);
#19702=AXIS2_PLACEMENT_3D('',#27477,#22319,#22320);
#19703=AXIS2_PLACEMENT_3D('',#27479,#22322,#22323);
#19704=AXIS2_PLACEMENT_3D('',#27481,#22324,#22325);
#19705=AXIS2_PLACEMENT_3D('',#27484,#22327,#22328);
#19706=AXIS2_PLACEMENT_3D('',#27485,#22329,#22330);
#19707=AXIS2_PLACEMENT_3D('',#27486,#22331,#22332);
#19708=AXIS2_PLACEMENT_3D('',#27487,#22333,#22334);
#19709=AXIS2_PLACEMENT_3D('',#27488,#22335,#22336);
#19710=AXIS2_PLACEMENT_3D('',#27490,#22337,#22338);
#19711=AXIS2_PLACEMENT_3D('',#27493,#22340,#22341);
#19712=AXIS2_PLACEMENT_3D('',#27494,#22342,#22343);
#19713=AXIS2_PLACEMENT_3D('',#27495,#22344,#22345);
#19714=AXIS2_PLACEMENT_3D('',#27497,#22346,#22347);
#19715=AXIS2_PLACEMENT_3D('',#27500,#22349,#22350);
#19716=AXIS2_PLACEMENT_3D('',#27501,#22351,#22352);
#19717=AXIS2_PLACEMENT_3D('',#27502,#22353,#22354);
#19718=AXIS2_PLACEMENT_3D('',#27503,#22355,#22356);
#19719=AXIS2_PLACEMENT_3D('',#27504,#22357,#22358);
#19720=AXIS2_PLACEMENT_3D('',#27506,#22359,#22360);
#19721=AXIS2_PLACEMENT_3D('',#27509,#22362,#22363);
#19722=AXIS2_PLACEMENT_3D('',#27510,#22364,#22365);
#19723=AXIS2_PLACEMENT_3D('',#27511,#22366,#22367);
#19724=AXIS2_PLACEMENT_3D('',#27513,#22368,#22369);
#19725=AXIS2_PLACEMENT_3D('',#27516,#22371,#22372);
#19726=AXIS2_PLACEMENT_3D('',#27517,#22373,#22374);
#19727=AXIS2_PLACEMENT_3D('',#27518,#22375,#22376);
#19728=AXIS2_PLACEMENT_3D('',#27519,#22377,#22378);
#19729=AXIS2_PLACEMENT_3D('',#27520,#22379,#22380);
#19730=AXIS2_PLACEMENT_3D('',#27522,#22381,#22382);
#19731=AXIS2_PLACEMENT_3D('',#27525,#22384,#22385);
#19732=AXIS2_PLACEMENT_3D('',#27526,#22386,#22387);
#19733=AXIS2_PLACEMENT_3D('',#27527,#22388,#22389);
#19734=AXIS2_PLACEMENT_3D('',#27529,#22390,#22391);
#19735=AXIS2_PLACEMENT_3D('',#27532,#22393,#22394);
#19736=AXIS2_PLACEMENT_3D('',#27533,#22395,#22396);
#19737=AXIS2_PLACEMENT_3D('',#27534,#22397,#22398);
#19738=AXIS2_PLACEMENT_3D('',#27535,#22399,#22400);
#19739=AXIS2_PLACEMENT_3D('',#27536,#22401,#22402);
#19740=AXIS2_PLACEMENT_3D('',#27538,#22403,#22404);
#19741=AXIS2_PLACEMENT_3D('',#27541,#22406,#22407);
#19742=AXIS2_PLACEMENT_3D('',#27542,#22408,#22409);
#19743=AXIS2_PLACEMENT_3D('',#27543,#22410,#22411);
#19744=AXIS2_PLACEMENT_3D('',#27545,#22412,#22413);
#19745=AXIS2_PLACEMENT_3D('',#27548,#22415,#22416);
#19746=AXIS2_PLACEMENT_3D('',#27549,#22417,#22418);
#19747=AXIS2_PLACEMENT_3D('',#27550,#22419,#22420);
#19748=AXIS2_PLACEMENT_3D('',#27551,#22421,#22422);
#19749=AXIS2_PLACEMENT_3D('',#27552,#22423,#22424);
#19750=AXIS2_PLACEMENT_3D('',#27554,#22425,#22426);
#19751=AXIS2_PLACEMENT_3D('',#27557,#22428,#22429);
#19752=AXIS2_PLACEMENT_3D('',#27558,#22430,#22431);
#19753=AXIS2_PLACEMENT_3D('',#27560,#22432,#22433);
#19754=AXIS2_PLACEMENT_3D('',#27561,#22434,#22435);
#19755=AXIS2_PLACEMENT_3D('',#27563,#22436,#22437);
#19756=AXIS2_PLACEMENT_3D('',#27566,#22439,#22440);
#19757=AXIS2_PLACEMENT_3D('',#27567,#22441,#22442);
#19758=AXIS2_PLACEMENT_3D('',#27569,#22443,#22444);
#19759=AXIS2_PLACEMENT_3D('',#27570,#22445,#22446);
#19760=AXIS2_PLACEMENT_3D('',#27572,#22447,#22448);
#19761=AXIS2_PLACEMENT_3D('',#27575,#22450,#22451);
#19762=AXIS2_PLACEMENT_3D('',#27576,#22452,#22453);
#19763=AXIS2_PLACEMENT_3D('',#27578,#22454,#22455);
#19764=AXIS2_PLACEMENT_3D('',#27579,#22456,#22457);
#19765=AXIS2_PLACEMENT_3D('',#27581,#22458,#22459);
#19766=AXIS2_PLACEMENT_3D('',#27584,#22461,#22462);
#19767=AXIS2_PLACEMENT_3D('',#27585,#22463,#22464);
#19768=AXIS2_PLACEMENT_3D('',#27587,#22465,#22466);
#19769=AXIS2_PLACEMENT_3D('',#27588,#22467,#22468);
#19770=AXIS2_PLACEMENT_3D('',#27590,#22469,#22470);
#19771=AXIS2_PLACEMENT_3D('',#27592,#22472,#22473);
#19772=AXIS2_PLACEMENT_3D('',#27594,#22474,#22475);
#19773=AXIS2_PLACEMENT_3D('',#27596,#22477,#22478);
#19774=AXIS2_PLACEMENT_3D('',#27598,#22479,#22480);
#19775=AXIS2_PLACEMENT_3D('',#27600,#22482,#22483);
#19776=AXIS2_PLACEMENT_3D('',#27602,#22484,#22485);
#19777=AXIS2_PLACEMENT_3D('',#27604,#22487,#22488);
#19778=AXIS2_PLACEMENT_3D('',#27606,#22489,#22490);
#19779=AXIS2_PLACEMENT_3D('',#27609,#22492,#22493);
#19780=AXIS2_PLACEMENT_3D('',#27610,#22494,#22495);
#19781=AXIS2_PLACEMENT_3D('',#27611,#22496,#22497);
#19782=AXIS2_PLACEMENT_3D('',#27612,#22498,#22499);
#19783=AXIS2_PLACEMENT_3D('',#27613,#22500,#22501);
#19784=AXIS2_PLACEMENT_3D('',#27622,#22506,#22507);
#19785=AXIS2_PLACEMENT_3D('',#27628,#22511,#22512);
#19786=AXIS2_PLACEMENT_3D('',#27634,#22516,#22517);
#19787=AXIS2_PLACEMENT_3D('',#27637,#22520,#22521);
#19788=AXIS2_PLACEMENT_3D('',#27638,#22522,#22523);
#19789=AXIS2_PLACEMENT_3D('',#27647,#22528,#22529);
#19790=AXIS2_PLACEMENT_3D('',#27653,#22533,#22534);
#19791=AXIS2_PLACEMENT_3D('',#27659,#22538,#22539);
#19792=AXIS2_PLACEMENT_3D('',#27662,#22542,#22543);
#19793=AXIS2_PLACEMENT_3D('',#27663,#22544,#22545);
#19794=AXIS2_PLACEMENT_3D('',#27672,#22550,#22551);
#19795=AXIS2_PLACEMENT_3D('',#27678,#22555,#22556);
#19796=AXIS2_PLACEMENT_3D('',#27684,#22560,#22561);
#19797=AXIS2_PLACEMENT_3D('',#27687,#22564,#22565);
#19798=AXIS2_PLACEMENT_3D('',#27688,#22566,#22567);
#19799=AXIS2_PLACEMENT_3D('',#27697,#22572,#22573);
#19800=AXIS2_PLACEMENT_3D('',#27703,#22577,#22578);
#19801=AXIS2_PLACEMENT_3D('',#27709,#22582,#22583);
#19802=AXIS2_PLACEMENT_3D('',#27712,#22586,#22587);
#19803=AXIS2_PLACEMENT_3D('',#27713,#22588,#22589);
#19804=AXIS2_PLACEMENT_3D('',#27722,#22594,#22595);
#19805=AXIS2_PLACEMENT_3D('',#27728,#22599,#22600);
#19806=AXIS2_PLACEMENT_3D('',#27734,#22604,#22605);
#19807=AXIS2_PLACEMENT_3D('',#27737,#22608,#22609);
#19808=AXIS2_PLACEMENT_3D('',#27738,#22610,#22611);
#19809=AXIS2_PLACEMENT_3D('',#27747,#22616,#22617);
#19810=AXIS2_PLACEMENT_3D('',#27753,#22621,#22622);
#19811=AXIS2_PLACEMENT_3D('',#27759,#22626,#22627);
#19812=AXIS2_PLACEMENT_3D('',#27762,#22630,#22631);
#19813=AXIS2_PLACEMENT_3D('',#27763,#22632,#22633);
#19814=AXIS2_PLACEMENT_3D('',#27772,#22638,#22639);
#19815=AXIS2_PLACEMENT_3D('',#27778,#22643,#22644);
#19816=AXIS2_PLACEMENT_3D('',#27784,#22648,#22649);
#19817=AXIS2_PLACEMENT_3D('',#27787,#22652,#22653);
#19818=AXIS2_PLACEMENT_3D('',#27788,#22654,#22655);
#19819=AXIS2_PLACEMENT_3D('',#27797,#22660,#22661);
#19820=AXIS2_PLACEMENT_3D('',#27803,#22665,#22666);
#19821=AXIS2_PLACEMENT_3D('',#27809,#22670,#22671);
#19822=AXIS2_PLACEMENT_3D('',#27812,#22674,#22675);
#19823=AXIS2_PLACEMENT_3D('',#27813,#22676,#22677);
#19824=AXIS2_PLACEMENT_3D('',#27822,#22682,#22683);
#19825=AXIS2_PLACEMENT_3D('',#27828,#22687,#22688);
#19826=AXIS2_PLACEMENT_3D('',#27834,#22692,#22693);
#19827=AXIS2_PLACEMENT_3D('',#27837,#22696,#22697);
#19828=AXIS2_PLACEMENT_3D('',#27838,#22698,#22699);
#19829=AXIS2_PLACEMENT_3D('',#27847,#22704,#22705);
#19830=AXIS2_PLACEMENT_3D('',#27853,#22709,#22710);
#19831=AXIS2_PLACEMENT_3D('',#27859,#22714,#22715);
#19832=AXIS2_PLACEMENT_3D('',#27862,#22718,#22719);
#19833=AXIS2_PLACEMENT_3D('',#27863,#22720,#22721);
#19834=AXIS2_PLACEMENT_3D('',#27872,#22726,#22727);
#19835=AXIS2_PLACEMENT_3D('',#27878,#22731,#22732);
#19836=AXIS2_PLACEMENT_3D('',#27884,#22736,#22737);
#19837=AXIS2_PLACEMENT_3D('',#27887,#22740,#22741);
#19838=AXIS2_PLACEMENT_3D('',#27888,#22742,#22743);
#19839=AXIS2_PLACEMENT_3D('',#27897,#22748,#22749);
#19840=AXIS2_PLACEMENT_3D('',#27903,#22753,#22754);
#19841=AXIS2_PLACEMENT_3D('',#27909,#22758,#22759);
#19842=AXIS2_PLACEMENT_3D('',#27912,#22762,#22763);
#19843=AXIS2_PLACEMENT_3D('',#27913,#22764,#22765);
#19844=AXIS2_PLACEMENT_3D('',#27922,#22770,#22771);
#19845=AXIS2_PLACEMENT_3D('',#27928,#22775,#22776);
#19846=AXIS2_PLACEMENT_3D('',#27934,#22780,#22781);
#19847=AXIS2_PLACEMENT_3D('',#27937,#22784,#22785);
#19848=AXIS2_PLACEMENT_3D('',#27938,#22786,#22787);
#19849=AXIS2_PLACEMENT_3D('',#27947,#22792,#22793);
#19850=AXIS2_PLACEMENT_3D('',#27953,#22797,#22798);
#19851=AXIS2_PLACEMENT_3D('',#27959,#22802,#22803);
#19852=AXIS2_PLACEMENT_3D('',#27962,#22806,#22807);
#19853=AXIS2_PLACEMENT_3D('',#27963,#22808,#22809);
#19854=AXIS2_PLACEMENT_3D('',#27972,#22814,#22815);
#19855=AXIS2_PLACEMENT_3D('',#27978,#22819,#22820);
#19856=AXIS2_PLACEMENT_3D('',#27984,#22824,#22825);
#19857=AXIS2_PLACEMENT_3D('',#27987,#22828,#22829);
#19858=AXIS2_PLACEMENT_3D('',#27988,#22830,#22831);
#19859=AXIS2_PLACEMENT_3D('',#27997,#22836,#22837);
#19860=AXIS2_PLACEMENT_3D('',#28003,#22841,#22842);
#19861=AXIS2_PLACEMENT_3D('',#28009,#22846,#22847);
#19862=AXIS2_PLACEMENT_3D('',#28012,#22850,#22851);
#19863=AXIS2_PLACEMENT_3D('',#28013,#22852,#22853);
#19864=AXIS2_PLACEMENT_3D('',#28022,#22858,#22859);
#19865=AXIS2_PLACEMENT_3D('',#28028,#22863,#22864);
#19866=AXIS2_PLACEMENT_3D('',#28034,#22868,#22869);
#19867=AXIS2_PLACEMENT_3D('',#28037,#22872,#22873);
#19868=AXIS2_PLACEMENT_3D('',#28038,#22874,#22875);
#19869=AXIS2_PLACEMENT_3D('',#28047,#22880,#22881);
#19870=AXIS2_PLACEMENT_3D('',#28053,#22885,#22886);
#19871=AXIS2_PLACEMENT_3D('',#28059,#22890,#22891);
#19872=AXIS2_PLACEMENT_3D('',#28062,#22894,#22895);
#19873=AXIS2_PLACEMENT_3D('',#28063,#22896,#22897);
#19874=AXIS2_PLACEMENT_3D('',#28072,#22902,#22903);
#19875=AXIS2_PLACEMENT_3D('',#28078,#22907,#22908);
#19876=AXIS2_PLACEMENT_3D('',#28084,#22912,#22913);
#19877=AXIS2_PLACEMENT_3D('',#28087,#22916,#22917);
#19878=AXIS2_PLACEMENT_3D('',#28088,#22918,#22919);
#19879=AXIS2_PLACEMENT_3D('',#28097,#22924,#22925);
#19880=AXIS2_PLACEMENT_3D('',#28103,#22929,#22930);
#19881=AXIS2_PLACEMENT_3D('',#28109,#22934,#22935);
#19882=AXIS2_PLACEMENT_3D('',#28112,#22938,#22939);
#19883=AXIS2_PLACEMENT_3D('',#28113,#22940,#22941);
#19884=AXIS2_PLACEMENT_3D('',#28122,#22946,#22947);
#19885=AXIS2_PLACEMENT_3D('',#28128,#22951,#22952);
#19886=AXIS2_PLACEMENT_3D('',#28134,#22956,#22957);
#19887=AXIS2_PLACEMENT_3D('',#28137,#22960,#22961);
#19888=AXIS2_PLACEMENT_3D('',#28138,#22962,#22963);
#19889=AXIS2_PLACEMENT_3D('',#28147,#22968,#22969);
#19890=AXIS2_PLACEMENT_3D('',#28153,#22973,#22974);
#19891=AXIS2_PLACEMENT_3D('',#28159,#22978,#22979);
#19892=AXIS2_PLACEMENT_3D('',#28162,#22982,#22983);
#19893=AXIS2_PLACEMENT_3D('',#28163,#22984,#22985);
#19894=AXIS2_PLACEMENT_3D('',#28172,#22990,#22991);
#19895=AXIS2_PLACEMENT_3D('',#28178,#22995,#22996);
#19896=AXIS2_PLACEMENT_3D('',#28184,#23000,#23001);
#19897=AXIS2_PLACEMENT_3D('',#28187,#23004,#23005);
#19898=AXIS2_PLACEMENT_3D('',#28188,#23006,#23007);
#19899=AXIS2_PLACEMENT_3D('',#28197,#23012,#23013);
#19900=AXIS2_PLACEMENT_3D('',#28203,#23017,#23018);
#19901=AXIS2_PLACEMENT_3D('',#28209,#23022,#23023);
#19902=AXIS2_PLACEMENT_3D('',#28212,#23026,#23027);
#19903=AXIS2_PLACEMENT_3D('',#28213,#23028,#23029);
#19904=AXIS2_PLACEMENT_3D('',#28222,#23034,#23035);
#19905=AXIS2_PLACEMENT_3D('',#28228,#23039,#23040);
#19906=AXIS2_PLACEMENT_3D('',#28234,#23044,#23045);
#19907=AXIS2_PLACEMENT_3D('',#28237,#23048,#23049);
#19908=AXIS2_PLACEMENT_3D('',#28238,#23050,#23051);
#19909=AXIS2_PLACEMENT_3D('',#28240,#23052,#23053);
#19910=AXIS2_PLACEMENT_3D('',#28243,#23055,#23056);
#19911=AXIS2_PLACEMENT_3D('',#28244,#23057,#23058);
#19912=AXIS2_PLACEMENT_3D('',#28246,#23059,#23060);
#19913=AXIS2_PLACEMENT_3D('',#28249,#23062,#23063);
#19914=AXIS2_PLACEMENT_3D('',#28250,#23064,#23065);
#19915=AXIS2_PLACEMENT_3D('',#28259,#23070,#23071);
#19916=AXIS2_PLACEMENT_3D('',#28265,#23075,#23076);
#19917=AXIS2_PLACEMENT_3D('',#28271,#23080,#23081);
#19918=AXIS2_PLACEMENT_3D('',#28274,#23084,#23085);
#19919=AXIS2_PLACEMENT_3D('',#28275,#23086,#23087);
#19920=AXIS2_PLACEMENT_3D('',#28276,#23088,#23089);
#19921=AXIS2_PLACEMENT_3D('',#28277,#23090,#23091);
#19922=AXIS2_PLACEMENT_3D('',#28279,#23092,#23093);
#19923=AXIS2_PLACEMENT_3D('',#28282,#23095,#23096);
#19924=AXIS2_PLACEMENT_3D('',#28283,#23097,#23098);
#19925=AXIS2_PLACEMENT_3D('',#28285,#23099,#23100);
#19926=AXIS2_PLACEMENT_3D('',#28287,#23102,#23103);
#19927=AXIS2_PLACEMENT_3D('',#28288,#23104,#23105);
#19928=AXIS2_PLACEMENT_3D('',#28290,#23106,#23107);
#19929=AXIS2_PLACEMENT_3D('',#28292,#23109,#23110);
#19930=AXIS2_PLACEMENT_3D('',#28293,#23111,#23112);
#19931=AXIS2_PLACEMENT_3D('',#28294,#23113,#23114);
#19932=AXIS2_PLACEMENT_3D('',#28298,#23116,#23117);
#19933=AXIS2_PLACEMENT_3D('',#28299,#23118,#23119);
#19934=AXIS2_PLACEMENT_3D('',#28303,#23121,#23122);
#19935=AXIS2_PLACEMENT_3D('',#28305,#23124,#23125);
#19936=AXIS2_PLACEMENT_3D('',#28310,#23127,#23128);
#19937=AXIS2_PLACEMENT_3D('',#28313,#23130,#23131);
#19938=AXIS2_PLACEMENT_3D('',#28314,#23132,#23133);
#19939=AXIS2_PLACEMENT_3D('',#28316,#23135,#23136);
#19940=AXIS2_PLACEMENT_3D('',#28327,#23142,#23143);
#19941=AXIS2_PLACEMENT_3D('',#28328,#23144,#23145);
#19942=AXIS2_PLACEMENT_3D('',#28335,#23149,#23150);
#19943=AXIS2_PLACEMENT_3D('',#28336,#23151,#23152);
#19944=AXIS2_PLACEMENT_3D('',#28347,#23158,#23159);
#19945=AXIS2_PLACEMENT_3D('',#28348,#23160,#23161);
#19946=AXIS2_PLACEMENT_3D('',#28350,#23162,#23163);
#19947=AXIS2_PLACEMENT_3D('',#28353,#23165,#23166);
#19948=AXIS2_PLACEMENT_3D('',#28354,#23167,#23168);
#19949=AXIS2_PLACEMENT_3D('',#28357,#23170,#23171);
#19950=AXIS2_PLACEMENT_3D('',#28358,#23172,#23173);
#19951=AXIS2_PLACEMENT_3D('',#28360,#23174,#23175);
#19952=AXIS2_PLACEMENT_3D('',#28362,#23177,#23178);
#19953=AXIS2_PLACEMENT_3D('',#28364,#23179,#23180);
#19954=AXIS2_PLACEMENT_3D('',#28366,#23182,#23183);
#19955=AXIS2_PLACEMENT_3D('',#28368,#23184,#23185);
#19956=AXIS2_PLACEMENT_3D('',#28371,#23187,#23188);
#19957=AXIS2_PLACEMENT_3D('',#28372,#23189,#23190);
#19958=AXIS2_PLACEMENT_3D('',#28389,#23200,#23201);
#19959=AXIS2_PLACEMENT_3D('',#28393,#23204,#23205);
#19960=AXIS2_PLACEMENT_3D('',#28397,#23208,#23209);
#19961=AXIS2_PLACEMENT_3D('',#28399,#23211,#23212);
#19962=AXIS2_PLACEMENT_3D('',#28403,#23215,#23216);
#19963=AXIS2_PLACEMENT_3D('',#28407,#23219,#23220);
#19964=AXIS2_PLACEMENT_3D('',#28411,#23223,#23224);
#19965=AXIS2_PLACEMENT_3D('',#28415,#23227,#23228);
#19966=AXIS2_PLACEMENT_3D('',#28419,#23231,#23232);
#19967=AXIS2_PLACEMENT_3D('',#28421,#23234,#23235);
#19968=AXIS2_PLACEMENT_3D('',#28422,#23236,#23237);
#19969=AXIS2_PLACEMENT_3D('',#28423,#23238,#23239);
#19970=AXIS2_PLACEMENT_3D('',#28432,#23244,#23245);
#19971=AXIS2_PLACEMENT_3D('',#28438,#23249,#23250);
#19972=AXIS2_PLACEMENT_3D('',#28444,#23254,#23255);
#19973=AXIS2_PLACEMENT_3D('',#28450,#23259,#23260);
#19974=AXIS2_PLACEMENT_3D('',#28456,#23264,#23265);
#19975=AXIS2_PLACEMENT_3D('',#28459,#23268,#23269);
#19976=AXIS2_PLACEMENT_3D('',#28460,#23270,#23271);
#19977=AXIS2_PLACEMENT_3D('',#28461,#23272,#23273);
#19978=AXIS2_PLACEMENT_3D('',#28463,#23274,#23275);
#19979=AXIS2_PLACEMENT_3D('',#28464,#23276,#23277);
#19980=AXIS2_PLACEMENT_3D('',#28466,#23278,#23279);
#19981=AXIS2_PLACEMENT_3D('',#28467,#23280,#23281);
#19982=AXIS2_PLACEMENT_3D('',#28469,#23282,#23283);
#19983=AXIS2_PLACEMENT_3D('',#28471,#23285,#23286);
#19984=AXIS2_PLACEMENT_3D('',#28473,#23287,#23288);
#19985=AXIS2_PLACEMENT_3D('',#28475,#23290,#23291);
#19986=AXIS2_PLACEMENT_3D('',#28477,#23292,#23293);
#19987=AXIS2_PLACEMENT_3D('',#28479,#23295,#23296);
#19988=AXIS2_PLACEMENT_3D('',#28481,#23297,#23298);
#19989=AXIS2_PLACEMENT_3D('',#28482,#23299,#23300);
#19990=AXIS2_PLACEMENT_3D('',#28484,#23301,#23302);
#19991=AXIS2_PLACEMENT_3D('',#28486,#23304,#23305);
#19992=AXIS2_PLACEMENT_3D('',#28488,#23307,#23308);
#19993=AXIS2_PLACEMENT_3D('',#28489,#23309,#23310);
#19994=AXIS2_PLACEMENT_3D('',#28490,#23311,#23312);
#19995=AXIS2_PLACEMENT_3D('',#28493,#23313,#23314);
#19996=AXIS2_PLACEMENT_3D('',#28494,#23315,#23316);
#19997=AXIS2_PLACEMENT_3D('',#28496,#23317,#23318);
#19998=AXIS2_PLACEMENT_3D('',#28498,#23319,#23320);
#19999=AXIS2_PLACEMENT_3D('',#28499,#23321,#23322);
#20000=AXIS2_PLACEMENT_3D('',#28500,#23323,#23324);
#20001=AXIS2_PLACEMENT_3D('',#28503,#23326,#23327);
#20002=AXIS2_PLACEMENT_3D('',#28504,#23328,#23329);
#20003=AXIS2_PLACEMENT_3D('',#28506,#23330,#23331);
#20004=AXIS2_PLACEMENT_3D('',#28509,#23333,#23334);
#20005=AXIS2_PLACEMENT_3D('',#28510,#23335,#23336);
#20006=AXIS2_PLACEMENT_3D('',#28513,#23338,#23339);
#20007=AXIS2_PLACEMENT_3D('',#28514,#23340,#23341);
#20008=AXIS2_PLACEMENT_3D('',#28515,#23342,#23343);
#20009=AXIS2_PLACEMENT_3D('',#28517,#23344,#23345);
#20010=AXIS2_PLACEMENT_3D('',#28519,#23347,#23348);
#20011=AXIS2_PLACEMENT_3D('',#28521,#23349,#23350);
#20012=AXIS2_PLACEMENT_3D('',#28522,#23351,#23352);
#20013=AXIS2_PLACEMENT_3D('',#28524,#23354,#23355);
#20014=AXIS2_PLACEMENT_3D('',#28525,#23356,#23357);
#20015=AXIS2_PLACEMENT_3D('',#28528,#23358,#23359);
#20016=AXIS2_PLACEMENT_3D('',#28529,#23360,#23361);
#20017=AXIS2_PLACEMENT_3D('',#28531,#23362,#23363);
#20018=AXIS2_PLACEMENT_3D('',#28533,#23364,#23365);
#20019=AXIS2_PLACEMENT_3D('',#28534,#23366,#23367);
#20020=AXIS2_PLACEMENT_3D('',#28535,#23368,#23369);
#20021=AXIS2_PLACEMENT_3D('',#28537,#23370,#23371);
#20022=AXIS2_PLACEMENT_3D('',#28539,#23373,#23374);
#20023=AXIS2_PLACEMENT_3D('',#28541,#23375,#23376);
#20024=AXIS2_PLACEMENT_3D('',#28543,#23377,#23378);
#20025=AXIS2_PLACEMENT_3D('',#28544,#23379,#23380);
#20026=AXIS2_PLACEMENT_3D('',#28546,#23381,#23382);
#20027=AXIS2_PLACEMENT_3D('',#28548,#23384,#23385);
#20028=AXIS2_PLACEMENT_3D('',#28550,#23386,#23387);
#20029=AXIS2_PLACEMENT_3D('',#28552,#23389,#23390);
#20030=AXIS2_PLACEMENT_3D('',#28554,#23391,#23392);
#20031=AXIS2_PLACEMENT_3D('',#28556,#23394,#23395);
#20032=AXIS2_PLACEMENT_3D('',#28557,#23396,#23397);
#20033=AXIS2_PLACEMENT_3D('',#28559,#23399,#23400);
#20034=AXIS2_PLACEMENT_3D('',#28560,#23401,#23402);
#20035=AXIS2_PLACEMENT_3D('',#28563,#23403,#23404);
#20036=AXIS2_PLACEMENT_3D('',#28564,#23405,#23406);
#20037=AXIS2_PLACEMENT_3D('',#28567,#23407,#23408);
#20038=AXIS2_PLACEMENT_3D('',#28568,#23409,#23410);
#20039=AXIS2_PLACEMENT_3D('',#28571,#23411,#23412);
#20040=AXIS2_PLACEMENT_3D('',#28572,#23413,#23414);
#20041=AXIS2_PLACEMENT_3D('',#28575,#23415,#23416);
#20042=AXIS2_PLACEMENT_3D('',#28576,#23417,#23418);
#20043=AXIS2_PLACEMENT_3D('',#28579,#23419,#23420);
#20044=AXIS2_PLACEMENT_3D('',#28580,#23421,#23422);
#20045=AXIS2_PLACEMENT_3D('',#28583,#23423,#23424);
#20046=AXIS2_PLACEMENT_3D('',#28584,#23425,#23426);
#20047=AXIS2_PLACEMENT_3D('',#28587,#23427,#23428);
#20048=AXIS2_PLACEMENT_3D('',#28588,#23429,#23430);
#20049=AXIS2_PLACEMENT_3D('',#28589,#23431,#23432);
#20050=AXIS2_PLACEMENT_3D('',#28615,#23433,#23434);
#20051=AXIS2_PLACEMENT_3D('',#28639,#23435,#23436);
#20052=AXIS2_PLACEMENT_3D('',#28640,#23437,#23438);
#20053=AXIS2_PLACEMENT_3D('',#28642,#23439,#23440);
#20054=AXIS2_PLACEMENT_3D('',#28667,#23441,#23442);
#20055=AXIS2_PLACEMENT_3D('',#28692,#23443,#23444);
#20056=AXIS2_PLACEMENT_3D('',#28695,#23446,#23447);
#20057=AXIS2_PLACEMENT_3D('',#28697,#23448,#23449);
#20058=AXIS2_PLACEMENT_3D('',#28722,#23450,#23451);
#20059=AXIS2_PLACEMENT_3D('',#28747,#23452,#23453);
#20060=AXIS2_PLACEMENT_3D('',#28772,#23454,#23455);
#20061=AXIS2_PLACEMENT_3D('',#28796,#23456,#23457);
#20062=AXIS2_PLACEMENT_3D('',#28797,#23458,#23459);
#20063=AXIS2_PLACEMENT_3D('',#28799,#23460,#23461);
#20064=AXIS2_PLACEMENT_3D('',#28800,#23462,#23463);
#20065=AXIS2_PLACEMENT_3D('',#28801,#23464,#23465);
#20066=AXIS2_PLACEMENT_3D('',#28825,#23466,#23467);
#20067=AXIS2_PLACEMENT_3D('',#28826,#23468,#23469);
#20068=AXIS2_PLACEMENT_3D('',#28828,#23470,#23471);
#20069=AXIS2_PLACEMENT_3D('',#28829,#23472,#23473);
#20070=AXIS2_PLACEMENT_3D('',#28830,#23474,#23475);
#20071=AXIS2_PLACEMENT_3D('',#28854,#23476,#23477);
#20072=AXIS2_PLACEMENT_3D('',#28855,#23478,#23479);
#20073=AXIS2_PLACEMENT_3D('',#28857,#23480,#23481);
#20074=AXIS2_PLACEMENT_3D('',#28859,#23482,#23483);
#20075=AXIS2_PLACEMENT_3D('',#28860,#23484,#23485);
#20076=AXIS2_PLACEMENT_3D('',#28861,#23486,#23487);
#20077=AXIS2_PLACEMENT_3D('',#28885,#23488,#23489);
#20078=AXIS2_PLACEMENT_3D('',#28886,#23490,#23491);
#20079=AXIS2_PLACEMENT_3D('',#28888,#23492,#23493);
#20080=AXIS2_PLACEMENT_3D('',#28889,#23494,#23495);
#20081=AXIS2_PLACEMENT_3D('',#28890,#23496,#23497);
#20082=AXIS2_PLACEMENT_3D('',#28914,#23498,#23499);
#20083=AXIS2_PLACEMENT_3D('',#28915,#23500,#23501);
#20084=AXIS2_PLACEMENT_3D('',#28917,#23502,#23503);
#20085=AXIS2_PLACEMENT_3D('',#28918,#23504,#23505);
#20086=AXIS2_PLACEMENT_3D('',#28919,#23506,#23507);
#20087=AXIS2_PLACEMENT_3D('',#28943,#23508,#23509);
#20088=AXIS2_PLACEMENT_3D('',#28944,#23510,#23511);
#20089=AXIS2_PLACEMENT_3D('',#28946,#23512,#23513);
#20090=AXIS2_PLACEMENT_3D('',#28949,#23515,#23516);
#20091=AXIS2_PLACEMENT_3D('',#28973,#23517,#23518);
#20092=AXIS2_PLACEMENT_3D('',#28974,#23519,#23520);
#20093=AXIS2_PLACEMENT_3D('',#28975,#23521,#23522);
#20094=AXIS2_PLACEMENT_3D('',#28976,#23523,#23524);
#20095=AXIS2_PLACEMENT_3D('',#28977,#23525,#23526);
#20096=AXIS2_PLACEMENT_3D('',#28978,#23527,#23528);
#20097=AXIS2_PLACEMENT_3D('',#28979,#23529,#23530);
#20098=AXIS2_PLACEMENT_3D('',#28980,#23531,#23532);
#20099=AXIS2_PLACEMENT_3D('',#28981,#23533,#23534);
#20100=AXIS2_PLACEMENT_3D('',#28983,#23535,#23536);
#20101=AXIS2_PLACEMENT_3D('',#28985,#23537,#23538);
#20102=AXIS2_PLACEMENT_3D('',#28986,#23539,#23540);
#20103=AXIS2_PLACEMENT_3D('',#28988,#23541,#23542);
#20104=AXIS2_PLACEMENT_3D('',#28990,#23544,#23545);
#20105=AXIS2_PLACEMENT_3D('',#28992,#23546,#23547);
#20106=AXIS2_PLACEMENT_3D('',#28993,#23548,#23549);
#20107=AXIS2_PLACEMENT_3D('',#28995,#23551,#23552);
#20108=AXIS2_PLACEMENT_3D('',#28997,#23553,#23554);
#20109=AXIS2_PLACEMENT_3D('',#28999,#23555,#23556);
#20110=AXIS2_PLACEMENT_3D('',#29000,#23557,#23558);
#20111=AXIS2_PLACEMENT_3D('',#29002,#23559,#23560);
#20112=AXIS2_PLACEMENT_3D('',#29004,#23562,#23563);
#20113=AXIS2_PLACEMENT_3D('',#29006,#23564,#23565);
#20114=AXIS2_PLACEMENT_3D('',#29007,#23566,#23567);
#20115=AXIS2_PLACEMENT_3D('',#29009,#23569,#23570);
#20116=AXIS2_PLACEMENT_3D('',#29010,#23571,#23572);
#20117=AXIS2_PLACEMENT_3D('',#29011,#23573,#23574);
#20118=AXIS2_PLACEMENT_3D('',#29012,#23575,#23576);
#20119=AXIS2_PLACEMENT_3D('',#29013,#23577,#23578);
#20120=AXIS2_PLACEMENT_3D('',#29014,#23579,#23580);
#20121=AXIS2_PLACEMENT_3D('',#29015,#23581,#23582);
#20122=AXIS2_PLACEMENT_3D('',#29016,#23583,#23584);
#20123=AXIS2_PLACEMENT_3D('',#29019,#23585,#23586);
#20124=AXIS2_PLACEMENT_3D('',#29020,#23587,#23588);
#20125=AXIS2_PLACEMENT_3D('',#29022,#23589,#23590);
#20126=AXIS2_PLACEMENT_3D('',#29024,#23591,#23592);
#20127=AXIS2_PLACEMENT_3D('',#29025,#23593,#23594);
#20128=AXIS2_PLACEMENT_3D('',#29026,#23595,#23596);
#20129=AXIS2_PLACEMENT_3D('',#29029,#23598,#23599);
#20130=AXIS2_PLACEMENT_3D('',#29030,#23600,#23601);
#20131=AXIS2_PLACEMENT_3D('',#29032,#23602,#23603);
#20132=AXIS2_PLACEMENT_3D('',#29035,#23605,#23606);
#20133=AXIS2_PLACEMENT_3D('',#29036,#23607,#23608);
#20134=AXIS2_PLACEMENT_3D('',#29039,#23610,#23611);
#20135=AXIS2_PLACEMENT_3D('',#29040,#23612,#23613);
#20136=AXIS2_PLACEMENT_3D('',#29041,#23614,#23615);
#20137=AXIS2_PLACEMENT_3D('',#29043,#23616,#23617);
#20138=AXIS2_PLACEMENT_3D('',#29045,#23619,#23620);
#20139=AXIS2_PLACEMENT_3D('',#29047,#23621,#23622);
#20140=AXIS2_PLACEMENT_3D('',#29048,#23623,#23624);
#20141=AXIS2_PLACEMENT_3D('',#29050,#23626,#23627);
#20142=AXIS2_PLACEMENT_3D('',#29051,#23628,#23629);
#20143=AXIS2_PLACEMENT_3D('',#29054,#23630,#23631);
#20144=AXIS2_PLACEMENT_3D('',#29055,#23632,#23633);
#20145=AXIS2_PLACEMENT_3D('',#29057,#23634,#23635);
#20146=AXIS2_PLACEMENT_3D('',#29059,#23636,#23637);
#20147=AXIS2_PLACEMENT_3D('',#29060,#23638,#23639);
#20148=AXIS2_PLACEMENT_3D('',#29061,#23640,#23641);
#20149=AXIS2_PLACEMENT_3D('',#29063,#23642,#23643);
#20150=AXIS2_PLACEMENT_3D('',#29065,#23645,#23646);
#20151=AXIS2_PLACEMENT_3D('',#29067,#23647,#23648);
#20152=AXIS2_PLACEMENT_3D('',#29069,#23649,#23650);
#20153=AXIS2_PLACEMENT_3D('',#29070,#23651,#23652);
#20154=AXIS2_PLACEMENT_3D('',#29072,#23653,#23654);
#20155=AXIS2_PLACEMENT_3D('',#29074,#23656,#23657);
#20156=AXIS2_PLACEMENT_3D('',#29076,#23658,#23659);
#20157=AXIS2_PLACEMENT_3D('',#29078,#23661,#23662);
#20158=AXIS2_PLACEMENT_3D('',#29080,#23663,#23664);
#20159=AXIS2_PLACEMENT_3D('',#29082,#23666,#23667);
#20160=AXIS2_PLACEMENT_3D('',#29083,#23668,#23669);
#20161=AXIS2_PLACEMENT_3D('',#29085,#23671,#23672);
#20162=AXIS2_PLACEMENT_3D('',#29086,#23673,#23674);
#20163=AXIS2_PLACEMENT_3D('',#29089,#23675,#23676);
#20164=AXIS2_PLACEMENT_3D('',#29090,#23677,#23678);
#20165=AXIS2_PLACEMENT_3D('',#29093,#23679,#23680);
#20166=AXIS2_PLACEMENT_3D('',#29094,#23681,#23682);
#20167=AXIS2_PLACEMENT_3D('',#29097,#23683,#23684);
#20168=AXIS2_PLACEMENT_3D('',#29098,#23685,#23686);
#20169=AXIS2_PLACEMENT_3D('',#29101,#23687,#23688);
#20170=AXIS2_PLACEMENT_3D('',#29102,#23689,#23690);
#20171=AXIS2_PLACEMENT_3D('',#29105,#23691,#23692);
#20172=AXIS2_PLACEMENT_3D('',#29106,#23693,#23694);
#20173=AXIS2_PLACEMENT_3D('',#29109,#23695,#23696);
#20174=AXIS2_PLACEMENT_3D('',#29110,#23697,#23698);
#20175=AXIS2_PLACEMENT_3D('',#29113,#23699,#23700);
#20176=AXIS2_PLACEMENT_3D('',#29114,#23701,#23702);
#20177=AXIS2_PLACEMENT_3D('',#29117,#23703,#23704);
#20178=AXIS2_PLACEMENT_3D('',#29118,#23705,#23706);
#20179=AXIS2_PLACEMENT_3D('',#29119,#23707,#23708);
#20180=AXIS2_PLACEMENT_3D('',#29145,#23709,#23710);
#20181=AXIS2_PLACEMENT_3D('',#29169,#23711,#23712);
#20182=AXIS2_PLACEMENT_3D('',#29170,#23713,#23714);
#20183=AXIS2_PLACEMENT_3D('',#29172,#23715,#23716);
#20184=AXIS2_PLACEMENT_3D('',#29197,#23717,#23718);
#20185=AXIS2_PLACEMENT_3D('',#29222,#23719,#23720);
#20186=AXIS2_PLACEMENT_3D('',#29238,#23722,#23723);
#20187=AXIS2_PLACEMENT_3D('',#29253,#23724,#23725);
#20188=AXIS2_PLACEMENT_3D('',#29278,#23726,#23727);
#20189=AXIS2_PLACEMENT_3D('',#29303,#23728,#23729);
#20190=AXIS2_PLACEMENT_3D('',#29328,#23730,#23731);
#20191=AXIS2_PLACEMENT_3D('',#29352,#23732,#23733);
#20192=AXIS2_PLACEMENT_3D('',#29353,#23734,#23735);
#20193=AXIS2_PLACEMENT_3D('',#29355,#23736,#23737);
#20194=AXIS2_PLACEMENT_3D('',#29356,#23738,#23739);
#20195=AXIS2_PLACEMENT_3D('',#29357,#23740,#23741);
#20196=AXIS2_PLACEMENT_3D('',#29381,#23742,#23743);
#20197=AXIS2_PLACEMENT_3D('',#29382,#23744,#23745);
#20198=AXIS2_PLACEMENT_3D('',#29384,#23746,#23747);
#20199=AXIS2_PLACEMENT_3D('',#29385,#23748,#23749);
#20200=AXIS2_PLACEMENT_3D('',#29386,#23750,#23751);
#20201=AXIS2_PLACEMENT_3D('',#29410,#23752,#23753);
#20202=AXIS2_PLACEMENT_3D('',#29411,#23754,#23755);
#20203=AXIS2_PLACEMENT_3D('',#29413,#23756,#23757);
#20204=AXIS2_PLACEMENT_3D('',#29414,#23758,#23759);
#20205=AXIS2_PLACEMENT_3D('',#29415,#23760,#23761);
#20206=AXIS2_PLACEMENT_3D('',#29430,#23762,#23763);
#20207=AXIS2_PLACEMENT_3D('',#29443,#23764,#23765);
#20208=AXIS2_PLACEMENT_3D('',#29445,#23766,#23767);
#20209=AXIS2_PLACEMENT_3D('',#29446,#23768,#23769);
#20210=AXIS2_PLACEMENT_3D('',#29447,#23770,#23771);
#20211=AXIS2_PLACEMENT_3D('',#29471,#23772,#23773);
#20212=AXIS2_PLACEMENT_3D('',#29472,#23774,#23775);
#20213=AXIS2_PLACEMENT_3D('',#29474,#23776,#23777);
#20214=AXIS2_PLACEMENT_3D('',#29475,#23778,#23779);
#20215=AXIS2_PLACEMENT_3D('',#29476,#23780,#23781);
#20216=AXIS2_PLACEMENT_3D('',#29500,#23782,#23783);
#20217=AXIS2_PLACEMENT_3D('',#29501,#23784,#23785);
#20218=AXIS2_PLACEMENT_3D('',#29503,#23786,#23787);
#20219=AXIS2_PLACEMENT_3D('',#29504,#23788,#23789);
#20220=AXIS2_PLACEMENT_3D('',#29505,#23790,#23791);
#20221=AXIS2_PLACEMENT_3D('',#29529,#23792,#23793);
#20222=AXIS2_PLACEMENT_3D('',#29530,#23794,#23795);
#20223=AXIS2_PLACEMENT_3D('',#29532,#23796,#23797);
#20224=AXIS2_PLACEMENT_3D('',#29535,#23799,#23800);
#20225=AXIS2_PLACEMENT_3D('',#29559,#23801,#23802);
#20226=AXIS2_PLACEMENT_3D('',#29560,#23803,#23804);
#20227=AXIS2_PLACEMENT_3D('',#29561,#23805,#23806);
#20228=AXIS2_PLACEMENT_3D('',#29562,#23807,#23808);
#20229=AXIS2_PLACEMENT_3D('',#29563,#23809,#23810);
#20230=AXIS2_PLACEMENT_3D('',#29564,#23811,#23812);
#20231=AXIS2_PLACEMENT_3D('',#29565,#23813,#23814);
#20232=AXIS2_PLACEMENT_3D('',#29566,#23815,#23816);
#20233=AXIS2_PLACEMENT_3D('',#29567,#23817,#23818);
#20234=AXIS2_PLACEMENT_3D('',#29569,#23819,#23820);
#20235=AXIS2_PLACEMENT_3D('',#29571,#23821,#23822);
#20236=AXIS2_PLACEMENT_3D('',#29572,#23823,#23824);
#20237=AXIS2_PLACEMENT_3D('',#29574,#23825,#23826);
#20238=AXIS2_PLACEMENT_3D('',#29576,#23828,#23829);
#20239=AXIS2_PLACEMENT_3D('',#29578,#23830,#23831);
#20240=AXIS2_PLACEMENT_3D('',#29579,#23832,#23833);
#20241=AXIS2_PLACEMENT_3D('',#29581,#23835,#23836);
#20242=AXIS2_PLACEMENT_3D('',#29583,#23837,#23838);
#20243=AXIS2_PLACEMENT_3D('',#29585,#23839,#23840);
#20244=AXIS2_PLACEMENT_3D('',#29586,#23841,#23842);
#20245=AXIS2_PLACEMENT_3D('',#29588,#23843,#23844);
#20246=AXIS2_PLACEMENT_3D('',#29590,#23846,#23847);
#20247=AXIS2_PLACEMENT_3D('',#29592,#23848,#23849);
#20248=AXIS2_PLACEMENT_3D('',#29593,#23850,#23851);
#20249=AXIS2_PLACEMENT_3D('',#29595,#23853,#23854);
#20250=AXIS2_PLACEMENT_3D('',#29596,#23855,#23856);
#20251=AXIS2_PLACEMENT_3D('',#29597,#23857,#23858);
#20252=AXIS2_PLACEMENT_3D('',#29598,#23859,#23860);
#20253=AXIS2_PLACEMENT_3D('',#29599,#23861,#23862);
#20254=AXIS2_PLACEMENT_3D('',#29600,#23863,#23864);
#20255=AXIS2_PLACEMENT_3D('',#29601,#23865,#23866);
#20256=AXIS2_PLACEMENT_3D('',#29603,#23867,#23868);
#20257=AXIS2_PLACEMENT_3D('',#29604,#23869,#23870);
#20258=AXIS2_PLACEMENT_3D('',#29606,#23871,#23872);
#20259=AXIS2_PLACEMENT_3D('',#29608,#23873,#23874);
#20260=AXIS2_PLACEMENT_3D('',#29609,#23875,#23876);
#20261=AXIS2_PLACEMENT_3D('',#29611,#23878,#23879);
#20262=AXIS2_PLACEMENT_3D('',#29613,#23880,#23881);
#20263=AXIS2_PLACEMENT_3D('',#29614,#23882,#23883);
#20264=AXIS2_PLACEMENT_3D('',#29616,#23884,#23885);
#20265=AXIS2_PLACEMENT_3D('',#29618,#23887,#23888);
#20266=AXIS2_PLACEMENT_3D('',#29620,#23889,#23890);
#20267=AXIS2_PLACEMENT_3D('',#29622,#23892,#23893);
#20268=AXIS2_PLACEMENT_3D('',#29624,#23894,#23895);
#20269=AXIS2_PLACEMENT_3D('',#29626,#23897,#23898);
#20270=AXIS2_PLACEMENT_3D('',#29628,#23899,#23900);
#20271=AXIS2_PLACEMENT_3D('',#29629,#23901,#23902);
#20272=AXIS2_PLACEMENT_3D('',#29631,#23903,#23904);
#20273=AXIS2_PLACEMENT_3D('',#29633,#23906,#23907);
#20274=AXIS2_PLACEMENT_3D('',#29635,#23909,#23910);
#20275=AXIS2_PLACEMENT_3D('',#29644,#23915,#23916);
#20276=AXIS2_PLACEMENT_3D('',#29650,#23920,#23921);
#20277=AXIS2_PLACEMENT_3D('',#29656,#23925,#23926);
#20278=AXIS2_PLACEMENT_3D('',#29662,#23930,#23931);
#20279=AXIS2_PLACEMENT_3D('',#29668,#23935,#23936);
#20280=AXIS2_PLACEMENT_3D('',#29671,#23939,#23940);
#20281=AXIS2_PLACEMENT_3D('',#29672,#23941,#23942);
#20282=AXIS2_PLACEMENT_3D('',#29673,#23943,#23944);
#20283=AXIS2_PLACEMENT_3D('',#29674,#23945,#23946);
#20284=AXIS2_PLACEMENT_3D('',#29683,#23951,#23952);
#20285=AXIS2_PLACEMENT_3D('',#29689,#23956,#23957);
#20286=AXIS2_PLACEMENT_3D('',#29695,#23961,#23962);
#20287=AXIS2_PLACEMENT_3D('',#29701,#23966,#23967);
#20288=AXIS2_PLACEMENT_3D('',#29707,#23971,#23972);
#20289=AXIS2_PLACEMENT_3D('',#29710,#23975,#23976);
#20290=AXIS2_PLACEMENT_3D('',#29711,#23977,#23978);
#20291=AXIS2_PLACEMENT_3D('',#29712,#23979,#23980);
#20292=AXIS2_PLACEMENT_3D('',#29714,#23981,#23982);
#20293=AXIS2_PLACEMENT_3D('',#29715,#23983,#23984);
#20294=AXIS2_PLACEMENT_3D('',#29717,#23985,#23986);
#20295=AXIS2_PLACEMENT_3D('',#29718,#23987,#23988);
#20296=AXIS2_PLACEMENT_3D('',#29720,#23989,#23990);
#20297=AXIS2_PLACEMENT_3D('',#29722,#23992,#23993);
#20298=AXIS2_PLACEMENT_3D('',#29724,#23994,#23995);
#20299=AXIS2_PLACEMENT_3D('',#29726,#23997,#23998);
#20300=AXIS2_PLACEMENT_3D('',#29728,#23999,#24000);
#20301=AXIS2_PLACEMENT_3D('',#29730,#24002,#24003);
#20302=AXIS2_PLACEMENT_3D('',#29732,#24004,#24005);
#20303=AXIS2_PLACEMENT_3D('',#29733,#24006,#24007);
#20304=AXIS2_PLACEMENT_3D('',#29735,#24008,#24009);
#20305=AXIS2_PLACEMENT_3D('',#29737,#24011,#24012);
#20306=AXIS2_PLACEMENT_3D('',#29739,#24014,#24015);
#20307=AXIS2_PLACEMENT_3D('',#29740,#24016,#24017);
#20308=AXIS2_PLACEMENT_3D('',#29749,#24022,#24023);
#20309=AXIS2_PLACEMENT_3D('',#29755,#24027,#24028);
#20310=AXIS2_PLACEMENT_3D('',#29761,#24032,#24033);
#20311=AXIS2_PLACEMENT_3D('',#29767,#24037,#24038);
#20312=AXIS2_PLACEMENT_3D('',#29773,#24042,#24043);
#20313=AXIS2_PLACEMENT_3D('',#29779,#24047,#24048);
#20314=AXIS2_PLACEMENT_3D('',#29785,#24052,#24053);
#20315=AXIS2_PLACEMENT_3D('',#29791,#24057,#24058);
#20316=AXIS2_PLACEMENT_3D('',#29797,#24062,#24063);
#20317=AXIS2_PLACEMENT_3D('',#29806,#24068,#24069);
#20318=AXIS2_PLACEMENT_3D('',#29812,#24073,#24074);
#20319=AXIS2_PLACEMENT_3D('',#29818,#24078,#24079);
#20320=AXIS2_PLACEMENT_3D('',#29824,#24083,#24084);
#20321=AXIS2_PLACEMENT_3D('',#29830,#24088,#24089);
#20322=AXIS2_PLACEMENT_3D('',#29836,#24093,#24094);
#20323=AXIS2_PLACEMENT_3D('',#29842,#24098,#24099);
#20324=AXIS2_PLACEMENT_3D('',#29848,#24103,#24104);
#20325=AXIS2_PLACEMENT_3D('',#29854,#24108,#24109);
#20326=AXIS2_PLACEMENT_3D('',#29863,#24114,#24115);
#20327=AXIS2_PLACEMENT_3D('',#29869,#24119,#24120);
#20328=AXIS2_PLACEMENT_3D('',#29875,#24124,#24125);
#20329=AXIS2_PLACEMENT_3D('',#29881,#24129,#24130);
#20330=AXIS2_PLACEMENT_3D('',#29887,#24134,#24135);
#20331=AXIS2_PLACEMENT_3D('',#29893,#24139,#24140);
#20332=AXIS2_PLACEMENT_3D('',#29899,#24144,#24145);
#20333=AXIS2_PLACEMENT_3D('',#29905,#24149,#24150);
#20334=AXIS2_PLACEMENT_3D('',#29911,#24154,#24155);
#20335=AXIS2_PLACEMENT_3D('',#29920,#24160,#24161);
#20336=AXIS2_PLACEMENT_3D('',#29926,#24165,#24166);
#20337=AXIS2_PLACEMENT_3D('',#29932,#24170,#24171);
#20338=AXIS2_PLACEMENT_3D('',#29938,#24175,#24176);
#20339=AXIS2_PLACEMENT_3D('',#29944,#24180,#24181);
#20340=AXIS2_PLACEMENT_3D('',#29950,#24185,#24186);
#20341=AXIS2_PLACEMENT_3D('',#29956,#24190,#24191);
#20342=AXIS2_PLACEMENT_3D('',#29962,#24195,#24196);
#20343=AXIS2_PLACEMENT_3D('',#29968,#24200,#24201);
#20344=AXIS2_PLACEMENT_3D('',#29970,#24202,#24203);
#20345=AXIS2_PLACEMENT_3D('',#29973,#24205,#24206);
#20346=AXIS2_PLACEMENT_3D('',#29974,#24207,#24208);
#20347=AXIS2_PLACEMENT_3D('',#29980,#24212,#24213);
#20348=AXIS2_PLACEMENT_3D('',#29986,#24217,#24218);
#20349=AXIS2_PLACEMENT_3D('',#29989,#24221,#24222);
#20350=AXIS2_PLACEMENT_3D('',#29995,#24226,#24227);
#20351=AXIS2_PLACEMENT_3D('',#29998,#24230,#24231);
#20352=AXIS2_PLACEMENT_3D('',#30004,#24235,#24236);
#20353=AXIS2_PLACEMENT_3D('',#30007,#24239,#24240);
#20354=AXIS2_PLACEMENT_3D('',#30010,#24243,#24244);
#20355=AXIS2_PLACEMENT_3D('',#30011,#24245,#24246);
#20356=AXIS2_PLACEMENT_3D('',#30012,#24247,#24248);
#20357=AXIS2_PLACEMENT_3D('',#30013,#24249,#24250);
#20358=AXIS2_PLACEMENT_3D('',#30015,#24251,#24252);
#20359=AXIS2_PLACEMENT_3D('',#30016,#24253,#24254);
#20360=AXIS2_PLACEMENT_3D('',#30018,#24255,#24256);
#20361=AXIS2_PLACEMENT_3D('',#30020,#24258,#24259);
#20362=AXIS2_PLACEMENT_3D('',#30022,#24260,#24261);
#20363=AXIS2_PLACEMENT_3D('',#30024,#24263,#24264);
#20364=AXIS2_PLACEMENT_3D('',#30026,#24265,#24266);
#20365=AXIS2_PLACEMENT_3D('',#30028,#24268,#24269);
#20366=AXIS2_PLACEMENT_3D('',#30030,#24270,#24271);
#20367=AXIS2_PLACEMENT_3D('',#30031,#24272,#24273);
#20368=AXIS2_PLACEMENT_3D('',#30033,#24274,#24275);
#20369=AXIS2_PLACEMENT_3D('',#30035,#24277,#24278);
#20370=AXIS2_PLACEMENT_3D('',#30037,#24279,#24280);
#20371=AXIS2_PLACEMENT_3D('',#30039,#24282,#24283);
#20372=AXIS2_PLACEMENT_3D('',#30041,#24284,#24285);
#20373=AXIS2_PLACEMENT_3D('',#30043,#24287,#24288);
#20374=AXIS2_PLACEMENT_3D('',#30044,#24289,#24290);
#20375=AXIS2_PLACEMENT_3D('',#30053,#24295,#24296);
#20376=AXIS2_PLACEMENT_3D('',#30059,#24300,#24301);
#20377=AXIS2_PLACEMENT_3D('',#30065,#24305,#24306);
#20378=AXIS2_PLACEMENT_3D('',#30071,#24310,#24311);
#20379=AXIS2_PLACEMENT_3D('',#30077,#24315,#24316);
#20380=AXIS2_PLACEMENT_3D('',#30080,#24319,#24320);
#20381=AXIS2_PLACEMENT_3D('',#30081,#24321,#24322);
#20382=AXIS2_PLACEMENT_3D('',#30082,#24323,#24324);
#20383=AXIS2_PLACEMENT_3D('',#30083,#24325,#24326);
#20384=AXIS2_PLACEMENT_3D('',#30092,#24331,#24332);
#20385=AXIS2_PLACEMENT_3D('',#30098,#24336,#24337);
#20386=AXIS2_PLACEMENT_3D('',#30105,#24341,#24342);
#20387=AXIS2_PLACEMENT_3D('',#30106,#24343,#24344);
#20388=AXIS2_PLACEMENT_3D('',#30120,#24352,#24353);
#20389=AXIS2_PLACEMENT_3D('',#30124,#24356,#24357);
#20390=AXIS2_PLACEMENT_3D('',#30128,#24360,#24361);
#20391=AXIS2_PLACEMENT_3D('',#30138,#24367,#24368);
#20392=AXIS2_PLACEMENT_3D('',#30140,#24370,#24371);
#20393=AXIS2_PLACEMENT_3D('',#30144,#24373,#24374);
#20394=AXIS2_PLACEMENT_3D('',#30146,#24376,#24377);
#20395=AXIS2_PLACEMENT_3D('',#30148,#24378,#24379);
#20396=AXIS2_PLACEMENT_3D('',#30151,#24381,#24382);
#20397=AXIS2_PLACEMENT_3D('',#30153,#24383,#24384);
#20398=AXIS2_PLACEMENT_3D('',#30154,#24385,#24386);
#20399=AXIS2_PLACEMENT_3D('',#30155,#24387,#24388);
#20400=AXIS2_PLACEMENT_3D('',#30157,#24390,#24391);
#20401=AXIS2_PLACEMENT_3D('',#30159,#24393,#24394);
#20402=AXIS2_PLACEMENT_3D('',#30161,#24396,#24397);
#20403=AXIS2_PLACEMENT_3D('',#30162,#24398,#24399);
#20404=AXIS2_PLACEMENT_3D('',#30163,#24400,#24401);
#20405=AXIS2_PLACEMENT_3D('',#30165,#24402,#24403);
#20406=AXIS2_PLACEMENT_3D('',#30178,#24410,#24411);
#20407=AXIS2_PLACEMENT_3D('',#30180,#24412,#24413);
#20408=AXIS2_PLACEMENT_3D('',#30181,#24414,#24415);
#20409=AXIS2_PLACEMENT_3D('',#30183,#24416,#24417);
#20410=AXIS2_PLACEMENT_3D('',#30185,#24419,#24420);
#20411=AXIS2_PLACEMENT_3D('',#30187,#24421,#24422);
#20412=AXIS2_PLACEMENT_3D('',#30189,#24424,#24425);
#20413=AXIS2_PLACEMENT_3D('',#30191,#24426,#24427);
#20414=AXIS2_PLACEMENT_3D('',#30193,#24429,#24430);
#20415=AXIS2_PLACEMENT_3D('',#30195,#24431,#24432);
#20416=AXIS2_PLACEMENT_3D('',#30196,#24433,#24434);
#20417=AXIS2_PLACEMENT_3D('',#30198,#24435,#24436);
#20418=AXIS2_PLACEMENT_3D('',#30200,#24438,#24439);
#20419=AXIS2_PLACEMENT_3D('',#30202,#24441,#24442);
#20420=AXIS2_PLACEMENT_3D('',#30208,#24446,#24447);
#20421=AXIS2_PLACEMENT_3D('',#30212,#24450,#24451);
#20422=AXIS2_PLACEMENT_3D('',#30216,#24454,#24455);
#20423=AXIS2_PLACEMENT_3D('',#30220,#24458,#24459);
#20424=AXIS2_PLACEMENT_3D('',#30224,#24462,#24463);
#20425=AXIS2_PLACEMENT_3D('',#30226,#24465,#24466);
#20426=AXIS2_PLACEMENT_3D('',#30227,#24467,#24468);
#20427=AXIS2_PLACEMENT_3D('',#30228,#24469,#24470);
#20428=AXIS2_PLACEMENT_3D('',#30229,#24471,#24472);
#20429=AXIS2_PLACEMENT_3D('',#30231,#24473,#24474);
#20430=AXIS2_PLACEMENT_3D('',#30234,#24476,#24477);
#20431=AXIS2_PLACEMENT_3D('',#30235,#24478,#24479);
#20432=AXIS2_PLACEMENT_3D('',#30237,#24480,#24481);
#20433=AXIS2_PLACEMENT_3D('',#30240,#24483,#24484);
#20434=AXIS2_PLACEMENT_3D('',#30241,#24485,#24486);
#20435=AXIS2_PLACEMENT_3D('',#30243,#24487,#24488);
#20436=AXIS2_PLACEMENT_3D('',#30246,#24490,#24491);
#20437=AXIS2_PLACEMENT_3D('',#30247,#24492,#24493);
#20438=AXIS2_PLACEMENT_3D('',#30249,#24494,#24495);
#20439=AXIS2_PLACEMENT_3D('',#30252,#24497,#24498);
#20440=AXIS2_PLACEMENT_3D('',#30253,#24499,#24500);
#20441=AXIS2_PLACEMENT_3D('',#30255,#24501,#24502);
#20442=AXIS2_PLACEMENT_3D('',#30258,#24504,#24505);
#20443=AXIS2_PLACEMENT_3D('',#30259,#24506,#24507);
#20444=AXIS2_PLACEMENT_3D('',#30261,#24508,#24509);
#20445=AXIS2_PLACEMENT_3D('',#30264,#24511,#24512);
#20446=AXIS2_PLACEMENT_3D('',#30265,#24513,#24514);
#20447=AXIS2_PLACEMENT_3D('',#30267,#24515,#24516);
#20448=AXIS2_PLACEMENT_3D('',#30270,#24518,#24519);
#20449=AXIS2_PLACEMENT_3D('',#30271,#24520,#24521);
#20450=AXIS2_PLACEMENT_3D('',#30273,#24522,#24523);
#20451=AXIS2_PLACEMENT_3D('',#30276,#24525,#24526);
#20452=AXIS2_PLACEMENT_3D('',#30277,#24527,#24528);
#20453=AXIS2_PLACEMENT_3D('',#30279,#24529,#24530);
#20454=AXIS2_PLACEMENT_3D('',#30282,#24532,#24533);
#20455=AXIS2_PLACEMENT_3D('',#30283,#24534,#24535);
#20456=AXIS2_PLACEMENT_3D('',#30285,#24536,#24537);
#20457=AXIS2_PLACEMENT_3D('',#30288,#24539,#24540);
#20458=AXIS2_PLACEMENT_3D('',#30289,#24541,#24542);
#20459=AXIS2_PLACEMENT_3D('',#30291,#24543,#24544);
#20460=AXIS2_PLACEMENT_3D('',#30294,#24546,#24547);
#20461=AXIS2_PLACEMENT_3D('',#30295,#24548,#24549);
#20462=AXIS2_PLACEMENT_3D('',#30297,#24550,#24551);
#20463=AXIS2_PLACEMENT_3D('',#30300,#24553,#24554);
#20464=AXIS2_PLACEMENT_3D('',#30301,#24555,#24556);
#20465=AXIS2_PLACEMENT_3D('',#30303,#24557,#24558);
#20466=AXIS2_PLACEMENT_3D('',#30306,#24560,#24561);
#20467=AXIS2_PLACEMENT_3D('',#30307,#24562,#24563);
#20468=AXIS2_PLACEMENT_3D('',#30309,#24564,#24565);
#20469=AXIS2_PLACEMENT_3D('',#30312,#24567,#24568);
#20470=AXIS2_PLACEMENT_3D('',#30313,#24569,#24570);
#20471=AXIS2_PLACEMENT_3D('',#30315,#24571,#24572);
#20472=AXIS2_PLACEMENT_3D('',#30318,#24574,#24575);
#20473=AXIS2_PLACEMENT_3D('',#30319,#24576,#24577);
#20474=AXIS2_PLACEMENT_3D('',#30321,#24578,#24579);
#20475=AXIS2_PLACEMENT_3D('',#30324,#24581,#24582);
#20476=AXIS2_PLACEMENT_3D('',#30325,#24583,#24584);
#20477=AXIS2_PLACEMENT_3D('',#30327,#24585,#24586);
#20478=AXIS2_PLACEMENT_3D('',#30330,#24588,#24589);
#20479=AXIS2_PLACEMENT_3D('',#30331,#24590,#24591);
#20480=AXIS2_PLACEMENT_3D('',#30333,#24592,#24593);
#20481=AXIS2_PLACEMENT_3D('',#30336,#24595,#24596);
#20482=AXIS2_PLACEMENT_3D('',#30337,#24597,#24598);
#20483=AXIS2_PLACEMENT_3D('',#30346,#24603,#24604);
#20484=AXIS2_PLACEMENT_3D('',#30352,#24608,#24609);
#20485=AXIS2_PLACEMENT_3D('',#30358,#24613,#24614);
#20486=AXIS2_PLACEMENT_3D('',#30361,#24617,#24618);
#20487=AXIS2_PLACEMENT_3D('',#30362,#24619,#24620);
#20488=AXIS2_PLACEMENT_3D('',#30363,#24621,#24622);
#20489=AXIS2_PLACEMENT_3D('',#30364,#24623,#24624);
#20490=AXIS2_PLACEMENT_3D('',#30367,#24625,#24626);
#20491=AXIS2_PLACEMENT_3D('',#30368,#24627,#24628);
#20492=AXIS2_PLACEMENT_3D('',#30369,#24629,#24630);
#20493=AXIS2_PLACEMENT_3D('',#30373,#24632,#24633);
#20494=AXIS2_PLACEMENT_3D('',#30376,#24635,#24636);
#20495=AXIS2_PLACEMENT_3D('',#30378,#24637,#24638);
#20496=AXIS2_PLACEMENT_3D('',#30380,#24640,#24641);
#20497=AXIS2_PLACEMENT_3D('',#30383,#24642,#24643);
#20498=AXIS2_PLACEMENT_3D('',#30384,#24644,#24645);
#20499=AXIS2_PLACEMENT_3D('',#30385,#24646,#24647);
#20500=AXIS2_PLACEMENT_3D('',#30389,#24649,#24650);
#20501=AXIS2_PLACEMENT_3D('',#30392,#24652,#24653);
#20502=AXIS2_PLACEMENT_3D('',#30394,#24654,#24655);
#20503=AXIS2_PLACEMENT_3D('',#30396,#24657,#24658);
#20504=AXIS2_PLACEMENT_3D('',#30399,#24659,#24660);
#20505=AXIS2_PLACEMENT_3D('',#30401,#24661,#24662);
#20506=AXIS2_PLACEMENT_3D('',#30402,#24663,#24664);
#20507=AXIS2_PLACEMENT_3D('',#30403,#24665,#24666);
#20508=AXIS2_PLACEMENT_3D('',#30407,#24668,#24669);
#20509=AXIS2_PLACEMENT_3D('',#30411,#24672,#24673);
#20510=AXIS2_PLACEMENT_3D('',#30412,#24674,#24675);
#20511=AXIS2_PLACEMENT_3D('',#30415,#24676,#24677);
#20512=AXIS2_PLACEMENT_3D('',#30417,#24678,#24679);
#20513=AXIS2_PLACEMENT_3D('',#30418,#24680,#24681);
#20514=AXIS2_PLACEMENT_3D('',#30419,#24682,#24683);
#20515=AXIS2_PLACEMENT_3D('',#30423,#24685,#24686);
#20516=AXIS2_PLACEMENT_3D('',#30427,#24689,#24690);
#20517=AXIS2_PLACEMENT_3D('',#30428,#24691,#24692);
#20518=AXIS2_PLACEMENT_3D('',#30430,#24693,#24694);
#20519=AXIS2_PLACEMENT_3D('',#30433,#24696,#24697);
#20520=AXIS2_PLACEMENT_3D('',#30434,#24698,#24699);
#20521=AXIS2_PLACEMENT_3D('',#30435,#24700,#24701);
#20522=AXIS2_PLACEMENT_3D('',#30436,#24702,#24703);
#20523=AXIS2_PLACEMENT_3D('',#30437,#24704,#24705);
#20524=AXIS2_PLACEMENT_3D('',#30438,#24706,#24707);
#20525=AXIS2_PLACEMENT_3D('',#30440,#24708,#24709);
#20526=AXIS2_PLACEMENT_3D('',#30443,#24711,#24712);
#20527=AXIS2_PLACEMENT_3D('',#30444,#24713,#24714);
#20528=AXIS2_PLACEMENT_3D('',#30446,#24715,#24716);
#20529=AXIS2_PLACEMENT_3D('',#30447,#24717,#24718);
#20530=AXIS2_PLACEMENT_3D('',#30449,#24719,#24720);
#20531=AXIS2_PLACEMENT_3D('',#30450,#24721,#24722);
#20532=AXIS2_PLACEMENT_3D('',#30452,#24723,#24724);
#20533=AXIS2_PLACEMENT_3D('',#30454,#24726,#24727);
#20534=AXIS2_PLACEMENT_3D('',#30457,#24729,#24730);
#20535=AXIS2_PLACEMENT_3D('',#30458,#24731,#24732);
#20536=AXIS2_PLACEMENT_3D('',#30459,#24733,#24734);
#20537=AXIS2_PLACEMENT_3D('',#30460,#24735,#24736);
#20538=AXIS2_PLACEMENT_3D('',#30461,#24737,#24738);
#20539=AXIS2_PLACEMENT_3D('',#30464,#24739,#24740);
#20540=AXIS2_PLACEMENT_3D('',#30465,#24741,#24742);
#20541=AXIS2_PLACEMENT_3D('',#30466,#24743,#24744);
#20542=AXIS2_PLACEMENT_3D('',#30470,#24746,#24747);
#20543=AXIS2_PLACEMENT_3D('',#30473,#24749,#24750);
#20544=AXIS2_PLACEMENT_3D('',#30475,#24751,#24752);
#20545=AXIS2_PLACEMENT_3D('',#30477,#24754,#24755);
#20546=AXIS2_PLACEMENT_3D('',#30480,#24756,#24757);
#20547=AXIS2_PLACEMENT_3D('',#30481,#24758,#24759);
#20548=AXIS2_PLACEMENT_3D('',#30482,#24760,#24761);
#20549=AXIS2_PLACEMENT_3D('',#30486,#24763,#24764);
#20550=AXIS2_PLACEMENT_3D('',#30489,#24766,#24767);
#20551=AXIS2_PLACEMENT_3D('',#30491,#24768,#24769);
#20552=AXIS2_PLACEMENT_3D('',#30493,#24771,#24772);
#20553=AXIS2_PLACEMENT_3D('',#30496,#24773,#24774);
#20554=AXIS2_PLACEMENT_3D('',#30498,#24775,#24776);
#20555=AXIS2_PLACEMENT_3D('',#30499,#24777,#24778);
#20556=AXIS2_PLACEMENT_3D('',#30500,#24779,#24780);
#20557=AXIS2_PLACEMENT_3D('',#30504,#24782,#24783);
#20558=AXIS2_PLACEMENT_3D('',#30508,#24786,#24787);
#20559=AXIS2_PLACEMENT_3D('',#30509,#24788,#24789);
#20560=AXIS2_PLACEMENT_3D('',#30512,#24790,#24791);
#20561=AXIS2_PLACEMENT_3D('',#30514,#24792,#24793);
#20562=AXIS2_PLACEMENT_3D('',#30515,#24794,#24795);
#20563=AXIS2_PLACEMENT_3D('',#30516,#24796,#24797);
#20564=AXIS2_PLACEMENT_3D('',#30520,#24799,#24800);
#20565=AXIS2_PLACEMENT_3D('',#30524,#24803,#24804);
#20566=AXIS2_PLACEMENT_3D('',#30525,#24805,#24806);
#20567=AXIS2_PLACEMENT_3D('',#30527,#24807,#24808);
#20568=AXIS2_PLACEMENT_3D('',#30530,#24810,#24811);
#20569=AXIS2_PLACEMENT_3D('',#30531,#24812,#24813);
#20570=AXIS2_PLACEMENT_3D('',#30532,#24814,#24815);
#20571=AXIS2_PLACEMENT_3D('',#30533,#24816,#24817);
#20572=AXIS2_PLACEMENT_3D('',#30534,#24818,#24819);
#20573=AXIS2_PLACEMENT_3D('',#30535,#24820,#24821);
#20574=AXIS2_PLACEMENT_3D('',#30537,#24822,#24823);
#20575=AXIS2_PLACEMENT_3D('',#30540,#24825,#24826);
#20576=AXIS2_PLACEMENT_3D('',#30541,#24827,#24828);
#20577=AXIS2_PLACEMENT_3D('',#30543,#24829,#24830);
#20578=AXIS2_PLACEMENT_3D('',#30544,#24831,#24832);
#20579=AXIS2_PLACEMENT_3D('',#30546,#24833,#24834);
#20580=AXIS2_PLACEMENT_3D('',#30547,#24835,#24836);
#20581=AXIS2_PLACEMENT_3D('',#30549,#24837,#24838);
#20582=AXIS2_PLACEMENT_3D('',#30551,#24840,#24841);
#20583=AXIS2_PLACEMENT_3D('',#30554,#24843,#24844);
#20584=AXIS2_PLACEMENT_3D('',#30555,#24845,#24846);
#20585=AXIS2_PLACEMENT_3D('',#30556,#24847,#24848);
#20586=AXIS2_PLACEMENT_3D('',#30557,#24849,#24850);
#20587=AXIS2_PLACEMENT_3D('',#30558,#24851,#24852);
#20588=AXIS2_PLACEMENT_3D('',#30560,#24853,#24854);
#20589=AXIS2_PLACEMENT_3D('',#30563,#24856,#24857);
#20590=AXIS2_PLACEMENT_3D('',#30564,#24858,#24859);
#20591=AXIS2_PLACEMENT_3D('',#30565,#24860,#24861);
#20592=AXIS2_PLACEMENT_3D('',#30567,#24862,#24863);
#20593=AXIS2_PLACEMENT_3D('',#30570,#24865,#24866);
#20594=AXIS2_PLACEMENT_3D('',#30571,#24867,#24868);
#20595=AXIS2_PLACEMENT_3D('',#30572,#24869,#24870);
#20596=AXIS2_PLACEMENT_3D('',#30574,#24871,#24872);
#20597=AXIS2_PLACEMENT_3D('',#30577,#24874,#24875);
#20598=AXIS2_PLACEMENT_3D('',#30578,#24876,#24877);
#20599=AXIS2_PLACEMENT_3D('',#30579,#24878,#24879);
#20600=AXIS2_PLACEMENT_3D('',#30581,#24880,#24881);
#20601=AXIS2_PLACEMENT_3D('',#30584,#24883,#24884);
#20602=AXIS2_PLACEMENT_3D('',#30585,#24885,#24886);
#20603=AXIS2_PLACEMENT_3D('',#30587,#24887,#24888);
#20604=AXIS2_PLACEMENT_3D('',#30590,#24890,#24891);
#20605=AXIS2_PLACEMENT_3D('',#30591,#24892,#24893);
#20606=AXIS2_PLACEMENT_3D('',#30592,#24894,#24895);
#20607=AXIS2_PLACEMENT_3D('',#30593,#24896,#24897);
#20608=AXIS2_PLACEMENT_3D('',#30594,#24898,#24899);
#20609=AXIS2_PLACEMENT_3D('',#30596,#24900,#24901);
#20610=AXIS2_PLACEMENT_3D('',#30599,#24903,#24904);
#20611=AXIS2_PLACEMENT_3D('',#30600,#24905,#24906);
#20612=AXIS2_PLACEMENT_3D('',#30602,#24907,#24908);
#20613=AXIS2_PLACEMENT_3D('',#30605,#24910,#24911);
#20614=AXIS2_PLACEMENT_3D('',#30606,#24912,#24913);
#20615=AXIS2_PLACEMENT_3D('',#30608,#24914,#24915);
#20616=AXIS2_PLACEMENT_3D('',#30611,#24917,#24918);
#20617=AXIS2_PLACEMENT_3D('',#30612,#24919,#24920);
#20618=AXIS2_PLACEMENT_3D('',#30613,#24921,#24922);
#20619=AXIS2_PLACEMENT_3D('',#30614,#24923,#24924);
#20620=AXIS2_PLACEMENT_3D('',#30615,#24925,#24926);
#20621=AXIS2_PLACEMENT_3D('',#30617,#24927,#24928);
#20622=AXIS2_PLACEMENT_3D('',#30620,#24930,#24931);
#20623=AXIS2_PLACEMENT_3D('',#30621,#24932,#24933);
#20624=AXIS2_PLACEMENT_3D('',#30623,#24934,#24935);
#20625=AXIS2_PLACEMENT_3D('',#30626,#24937,#24938);
#20626=AXIS2_PLACEMENT_3D('',#30627,#24939,#24940);
#20627=AXIS2_PLACEMENT_3D('',#30636,#24945,#24946);
#20628=AXIS2_PLACEMENT_3D('',#30642,#24950,#24951);
#20629=AXIS2_PLACEMENT_3D('',#30644,#24953,#24954);
#20630=AXIS2_PLACEMENT_3D('',#30653,#24959,#24960);
#20631=AXIS2_PLACEMENT_3D('',#30659,#24964,#24965);
#20632=AXIS2_PLACEMENT_3D('',#30665,#24969,#24970);
#20633=AXIS2_PLACEMENT_3D('',#30667,#24972,#24973);
#20634=AXIS2_PLACEMENT_3D('',#30677,#24979,#24980);
#20635=AXIS2_PLACEMENT_3D('',#30683,#24984,#24985);
#20636=AXIS2_PLACEMENT_3D('',#30689,#24989,#24990);
#20637=AXIS2_PLACEMENT_3D('',#30693,#24994,#24995);
#20638=AXIS2_PLACEMENT_3D('',#30694,#24996,#24997);
#20639=AXIS2_PLACEMENT_3D('',#30695,#24998,#24999);
#20640=AXIS2_PLACEMENT_3D('',#30696,#25000,#25001);
#20641=AXIS2_PLACEMENT_3D('',#30697,#25002,#25003);
#20642=AXIS2_PLACEMENT_3D('',#30700,#25004,#25005);
#20643=AXIS2_PLACEMENT_3D('',#30706,#25009,#25010);
#20644=AXIS2_PLACEMENT_3D('',#30712,#25014,#25015);
#20645=AXIS2_PLACEMENT_3D('',#30714,#25016,#25017);
#20646=AXIS2_PLACEMENT_3D('',#30718,#25020,#25021);
#20647=AXIS2_PLACEMENT_3D('',#30721,#25024,#25025);
#20648=AXIS2_PLACEMENT_3D('',#30722,#25026,#25027);
#20649=AXIS2_PLACEMENT_3D('',#30724,#25028,#25029);
#20650=AXIS2_PLACEMENT_3D('',#30726,#25030,#25031);
#20651=AXIS2_PLACEMENT_3D('',#30727,#25032,#25033);
#20652=AXIS2_PLACEMENT_3D('',#30729,#25034,#25035);
#20653=AXIS2_PLACEMENT_3D('',#30731,#25037,#25038);
#20654=AXIS2_PLACEMENT_3D('',#30733,#25039,#25040);
#20655=AXIS2_PLACEMENT_3D('',#30734,#25041,#25042);
#20656=AXIS2_PLACEMENT_3D('',#30736,#25043,#25044);
#20657=AXIS2_PLACEMENT_3D('',#30738,#25046,#25047);
#20658=AXIS2_PLACEMENT_3D('',#30740,#25048,#25049);
#20659=AXIS2_PLACEMENT_3D('',#30741,#25050,#25051);
#20660=AXIS2_PLACEMENT_3D('',#30743,#25052,#25053);
#20661=AXIS2_PLACEMENT_3D('',#30745,#25055,#25056);
#20662=AXIS2_PLACEMENT_3D('',#30747,#25057,#25058);
#20663=AXIS2_PLACEMENT_3D('',#30748,#25059,#25060);
#20664=AXIS2_PLACEMENT_3D('',#30750,#25061,#25062);
#20665=AXIS2_PLACEMENT_3D('',#30752,#25064,#25065);
#20666=AXIS2_PLACEMENT_3D('',#30754,#25066,#25067);
#20667=AXIS2_PLACEMENT_3D('',#30755,#25068,#25069);
#20668=AXIS2_PLACEMENT_3D('',#30757,#25070,#25071);
#20669=AXIS2_PLACEMENT_3D('',#30759,#25073,#25074);
#20670=AXIS2_PLACEMENT_3D('',#30761,#25075,#25076);
#20671=AXIS2_PLACEMENT_3D('',#30762,#25077,#25078);
#20672=AXIS2_PLACEMENT_3D('',#30764,#25080,#25081);
#20673=AXIS2_PLACEMENT_3D('',#30765,#25082,#25083);
#20674=AXIS2_PLACEMENT_3D('',#30768,#25084,#25085);
#20675=AXIS2_PLACEMENT_3D('',#30772,#25087,#25088);
#20676=AXIS2_PLACEMENT_3D('',#30774,#25090,#25091);
#20677=AXIS2_PLACEMENT_3D('',#30780,#25095,#25096);
#20678=AXIS2_PLACEMENT_3D('',#30782,#25097,#25098);
#20679=AXIS2_PLACEMENT_3D('',#30784,#25099,#25100);
#20680=AXIS2_PLACEMENT_3D('',#30786,#25102,#25103);
#20681=AXIS2_PLACEMENT_3D('',#30789,#25106,#25107);
#20682=AXIS2_PLACEMENT_3D('',#30791,#25108,#25109);
#20683=AXIS2_PLACEMENT_3D('',#30793,#25110,#25111);
#20684=AXIS2_PLACEMENT_3D('',#30794,#25112,#25113);
#20685=AXIS2_PLACEMENT_3D('',#30796,#25114,#25115);
#20686=AXIS2_PLACEMENT_3D('',#30798,#25117,#25118);
#20687=AXIS2_PLACEMENT_3D('',#30800,#25119,#25120);
#20688=AXIS2_PLACEMENT_3D('',#30801,#25121,#25122);
#20689=AXIS2_PLACEMENT_3D('',#30803,#25124,#25125);
#20690=AXIS2_PLACEMENT_3D('',#30804,#25126,#25127);
#20691=AXIS2_PLACEMENT_3D('',#30805,#25128,#25129);
#20692=AXIS2_PLACEMENT_3D('',#30806,#25130,#25131);
#20693=AXIS2_PLACEMENT_3D('',#30837,#25133,#25134);
#20694=AXIS2_PLACEMENT_3D('',#30878,#25135,#25136);
#20695=AXIS2_PLACEMENT_3D('',#30965,#25138,#25139);
#20696=AXIS2_PLACEMENT_3D('',#31055,#25141,#25142);
#20697=AXIS2_PLACEMENT_3D('',#31142,#25144,#25145);
#20698=AXIS2_PLACEMENT_3D('',#31232,#25147,#25148);
#20699=AXIS2_PLACEMENT_3D('',#31319,#25150,#25151);
#20700=AXIS2_PLACEMENT_3D('',#31406,#25153,#25154);
#20701=AXIS2_PLACEMENT_3D('',#31496,#25156,#25157);
#20702=AXIS2_PLACEMENT_3D('',#31501,#25159,#25160);
#20703=AXIS2_PLACEMENT_3D('',#31512,#25161,#25162);
#20704=AXIS2_PLACEMENT_3D('',#31525,#25164,#25165);
#20705=AXIS2_PLACEMENT_3D('',#31538,#25166,#25167);
#20706=AXIS2_PLACEMENT_3D('',#31575,#25169,#25170);
#20707=AXIS2_PLACEMENT_3D('',#31612,#25172,#25173);
#20708=AXIS2_PLACEMENT_3D('',#31650,#25175,#25176);
#20709=AXIS2_PLACEMENT_3D('',#31687,#25178,#25179);
#20710=AXIS2_PLACEMENT_3D('',#31724,#25181,#25182);
#20711=AXIS2_PLACEMENT_3D('',#31762,#25184,#25185);
#20712=AXIS2_PLACEMENT_3D('',#31800,#25187,#25188);
#20713=AXIS2_PLACEMENT_3D('',#31811,#25190,#25191);
#20714=AXIS2_PLACEMENT_3D('',#31822,#25192,#25193);
#20715=AXIS2_PLACEMENT_3D('',#32965,#25194,#25195);
#20716=AXIS2_PLACEMENT_3D('',#32969,#25197,#25198);
#20717=AXIS2_PLACEMENT_3D('',#32970,#25199,#25200);
#20718=AXIS2_PLACEMENT_3D('',#32972,#25201,#25202);
#20719=AXIS2_PLACEMENT_3D('',#32974,#25203,#25204);
#20720=AXIS2_PLACEMENT_3D('',#32976,#25205,#25206);
#20721=AXIS2_PLACEMENT_3D('',#32977,#25207,#25208);
#20722=AXIS2_PLACEMENT_3D('',#32979,#25209,#25210);
#20723=AXIS2_PLACEMENT_3D('',#32981,#25212,#25213);
#20724=AXIS2_PLACEMENT_3D('',#32983,#25214,#25215);
#20725=AXIS2_PLACEMENT_3D('',#32985,#25217,#25218);
#20726=AXIS2_PLACEMENT_3D('',#32987,#25219,#25220);
#20727=AXIS2_PLACEMENT_3D('',#32989,#25222,#25223);
#20728=AXIS2_PLACEMENT_3D('',#32995,#25227,#25228);
#20729=AXIS2_PLACEMENT_3D('',#32996,#25229,#25230);
#20730=AXIS2_PLACEMENT_3D('',#32998,#25231,#25232);
#20731=AXIS2_PLACEMENT_3D('',#32999,#25233,#25234);
#20732=AXIS2_PLACEMENT_3D('',#33000,#25235,#25236);
#20733=AXIS2_PLACEMENT_3D('',#33001,#25237,#25238);
#20734=AXIS2_PLACEMENT_3D('',#33004,#25240,#25241);
#20735=AXIS2_PLACEMENT_3D('',#33005,#25242,#25243);
#20736=AXIS2_PLACEMENT_3D('',#33006,#25244,#25245);
#20737=AXIS2_PLACEMENT_3D('',#33007,#25246,#25247);
#20738=AXIS2_PLACEMENT_3D('',#33016,#25252,#25253);
#20739=AXIS2_PLACEMENT_3D('',#33022,#25257,#25258);
#20740=AXIS2_PLACEMENT_3D('',#33028,#25262,#25263);
#20741=AXIS2_PLACEMENT_3D('',#33034,#25267,#25268);
#20742=AXIS2_PLACEMENT_3D('',#33040,#25272,#25273);
#20743=AXIS2_PLACEMENT_3D('',#33043,#25276,#25277);
#20744=AXIS2_PLACEMENT_3D('',#33044,#25278,#25279);
#20745=AXIS2_PLACEMENT_3D('',#33045,#25280,#25281);
#20746=AXIS2_PLACEMENT_3D('',#33047,#25282,#25283);
#20747=AXIS2_PLACEMENT_3D('',#33049,#25284,#25285);
#20748=AXIS2_PLACEMENT_3D('',#33050,#25286,#25287);
#20749=AXIS2_PLACEMENT_3D('',#33053,#25289,#25290);
#20750=AXIS2_PLACEMENT_3D('',#33054,#25291,#25292);
#20751=AXIS2_PLACEMENT_3D('',#33055,#25293,#25294);
#20752=AXIS2_PLACEMENT_3D('',#33057,#25295,#25296);
#20753=AXIS2_PLACEMENT_3D('',#33058,#25297,#25298);
#20754=AXIS2_PLACEMENT_3D('',#33060,#25299,#25300);
#20755=AXIS2_PLACEMENT_3D('',#33062,#25302,#25303);
#20756=AXIS2_PLACEMENT_3D('',#33064,#25304,#25305);
#20757=AXIS2_PLACEMENT_3D('',#33066,#25307,#25308);
#20758=AXIS2_PLACEMENT_3D('',#33068,#25309,#25310);
#20759=AXIS2_PLACEMENT_3D('',#33070,#25312,#25313);
#20760=AXIS2_PLACEMENT_3D('',#33072,#25314,#25315);
#20761=AXIS2_PLACEMENT_3D('',#33073,#25316,#25317);
#20762=AXIS2_PLACEMENT_3D('',#33075,#25318,#25319);
#20763=AXIS2_PLACEMENT_3D('',#33077,#25321,#25322);
#20764=AXIS2_PLACEMENT_3D('',#33079,#25324,#25325);
#20765=AXIS2_PLACEMENT_3D('',#33080,#25326,#25327);
#20766=AXIS2_PLACEMENT_3D('',#33082,#25328,#25329);
#20767=AXIS2_PLACEMENT_3D('',#33083,#25330,#25331);
#20768=AXIS2_PLACEMENT_3D('',#33085,#25332,#25333);
#20769=AXIS2_PLACEMENT_3D('',#33087,#25335,#25336);
#20770=AXIS2_PLACEMENT_3D('',#33089,#25337,#25338);
#20771=AXIS2_PLACEMENT_3D('',#33091,#25340,#25341);
#20772=AXIS2_PLACEMENT_3D('',#33093,#25342,#25343);
#20773=AXIS2_PLACEMENT_3D('',#33095,#25345,#25346);
#20774=AXIS2_PLACEMENT_3D('',#33097,#25347,#25348);
#20775=AXIS2_PLACEMENT_3D('',#33098,#25349,#25350);
#20776=AXIS2_PLACEMENT_3D('',#33100,#25351,#25352);
#20777=AXIS2_PLACEMENT_3D('',#33102,#25354,#25355);
#20778=AXIS2_PLACEMENT_3D('',#33104,#25356,#25357);
#20779=AXIS2_PLACEMENT_3D('',#33106,#25359,#25360);
#20780=AXIS2_PLACEMENT_3D('',#33108,#25361,#25362);
#20781=AXIS2_PLACEMENT_3D('',#33110,#25364,#25365);
#20782=AXIS2_PLACEMENT_3D('',#33111,#25366,#25367);
#20783=AXIS2_PLACEMENT_3D('',#33120,#25372,#25373);
#20784=AXIS2_PLACEMENT_3D('',#33126,#25377,#25378);
#20785=AXIS2_PLACEMENT_3D('',#33132,#25382,#25383);
#20786=AXIS2_PLACEMENT_3D('',#33138,#25387,#25388);
#20787=AXIS2_PLACEMENT_3D('',#33144,#25392,#25393);
#20788=AXIS2_PLACEMENT_3D('',#33147,#25396,#25397);
#20789=AXIS2_PLACEMENT_3D('',#33148,#25398,#25399);
#20790=AXIS2_PLACEMENT_3D('',#33149,#25400,#25401);
#20791=AXIS2_PLACEMENT_3D('',#33150,#25402,#25403);
#20792=AXIS2_PLACEMENT_3D('',#33151,#25404,#25405);
#20793=AXIS2_PLACEMENT_3D('',#33152,#25406,#25407);
#20794=AXIS2_PLACEMENT_3D('',#33153,#25408,#25409);
#20795=AXIS2_PLACEMENT_3D('',#33154,#25410,#25411);
#20796=AXIS2_PLACEMENT_3D('',#33155,#25412,#25413);
#20797=AXIS2_PLACEMENT_3D('',#33156,#25414,#25415);
#20798=AXIS2_PLACEMENT_3D('',#33157,#25416,#25417);
#20799=AXIS2_PLACEMENT_3D('',#33158,#25418,#25419);
#20800=AXIS2_PLACEMENT_3D('',#33159,#25420,#25421);
#20801=AXIS2_PLACEMENT_3D('',#33160,#25422,#25423);
#20802=AXIS2_PLACEMENT_3D('',#33161,#25424,#25425);
#20803=AXIS2_PLACEMENT_3D('',#33162,#25426,#25427);
#20804=AXIS2_PLACEMENT_3D('',#33163,#25428,#25429);
#20805=AXIS2_PLACEMENT_3D('',#33164,#25430,#25431);
#20806=AXIS2_PLACEMENT_3D('',#33165,#25432,#25433);
#20807=AXIS2_PLACEMENT_3D('',#33166,#25434,#25435);
#20808=AXIS2_PLACEMENT_3D('',#33167,#25436,#25437);
#20809=AXIS2_PLACEMENT_3D('',#33168,#25438,#25439);
#20810=AXIS2_PLACEMENT_3D('',#33169,#25440,#25441);
#20811=AXIS2_PLACEMENT_3D('',#33170,#25442,#25443);
#20812=AXIS2_PLACEMENT_3D('',#33171,#25444,#25445);
#20813=AXIS2_PLACEMENT_3D('',#33172,#25446,#25447);
#20814=AXIS2_PLACEMENT_3D('',#33173,#25448,#25449);
#20815=AXIS2_PLACEMENT_3D('',#33174,#25450,#25451);
#20816=AXIS2_PLACEMENT_3D('',#33175,#25452,#25453);
#20817=AXIS2_PLACEMENT_3D('',#33176,#25454,#25455);
#20818=AXIS2_PLACEMENT_3D('',#33177,#25456,#25457);
#20819=AXIS2_PLACEMENT_3D('',#33178,#25458,#25459);
#20820=AXIS2_PLACEMENT_3D('',#33179,#25460,#25461);
#20821=AXIS2_PLACEMENT_3D('',#33180,#25462,#25463);
#20822=AXIS2_PLACEMENT_3D('',#33181,#25464,#25465);
#20823=AXIS2_PLACEMENT_3D('',#33182,#25466,#25467);
#20824=AXIS2_PLACEMENT_3D('',#33183,#25468,#25469);
#20825=AXIS2_PLACEMENT_3D('',#33184,#25470,#25471);
#20826=AXIS2_PLACEMENT_3D('',#33185,#25472,#25473);
#20827=AXIS2_PLACEMENT_3D('',#33186,#25474,#25475);
#20828=AXIS2_PLACEMENT_3D('',#33187,#25476,#25477);
#20829=AXIS2_PLACEMENT_3D('',#33188,#25478,#25479);
#20830=AXIS2_PLACEMENT_3D('',#33189,#25480,#25481);
#20831=AXIS2_PLACEMENT_3D('',#33190,#25482,#25483);
#20832=AXIS2_PLACEMENT_3D('',#33191,#25484,#25485);
#20833=AXIS2_PLACEMENT_3D('',#33192,#25486,#25487);
#20834=AXIS2_PLACEMENT_3D('',#33193,#25488,#25489);
#20835=AXIS2_PLACEMENT_3D('',#33194,#25490,#25491);
#20836=AXIS2_PLACEMENT_3D('',#33195,#25492,#25493);
#20837=AXIS2_PLACEMENT_3D('',#33196,#25494,#25495);
#20838=AXIS2_PLACEMENT_3D('',#33197,#25496,#25497);
#20839=AXIS2_PLACEMENT_3D('',#33198,#25498,#25499);
#20840=AXIS2_PLACEMENT_3D('',#33199,#25500,#25501);
#20841=AXIS2_PLACEMENT_3D('',#33200,#25502,#25503);
#20842=AXIS2_PLACEMENT_3D('',#33201,#25504,#25505);
#20843=AXIS2_PLACEMENT_3D('',#33202,#25506,#25507);
#20844=AXIS2_PLACEMENT_3D('',#33203,#25508,#25509);
#20845=AXIS2_PLACEMENT_3D('',#33204,#25510,#25511);
#20846=AXIS2_PLACEMENT_3D('',#33205,#25512,#25513);
#20847=AXIS2_PLACEMENT_3D('',#33206,#25514,#25515);
#20848=AXIS2_PLACEMENT_3D('',#33207,#25516,#25517);
#20849=AXIS2_PLACEMENT_3D('',#33208,#25518,#25519);
#20850=AXIS2_PLACEMENT_3D('',#33209,#25520,#25521);
#20851=AXIS2_PLACEMENT_3D('',#33210,#25522,#25523);
#20852=AXIS2_PLACEMENT_3D('',#33211,#25524,#25525);
#20853=AXIS2_PLACEMENT_3D('',#33212,#25526,#25527);
#20854=AXIS2_PLACEMENT_3D('',#33213,#25528,#25529);
#20855=AXIS2_PLACEMENT_3D('',#33214,#25530,#25531);
#20856=AXIS2_PLACEMENT_3D('',#33215,#25532,#25533);
#20857=AXIS2_PLACEMENT_3D('',#33216,#25534,#25535);
#20858=AXIS2_PLACEMENT_3D('',#33217,#25536,#25537);
#20859=AXIS2_PLACEMENT_3D('',#33218,#25538,#25539);
#20860=AXIS2_PLACEMENT_3D('',#33219,#25540,#25541);
#20861=AXIS2_PLACEMENT_3D('',#33220,#25542,#25543);
#20862=AXIS2_PLACEMENT_3D('',#33221,#25544,#25545);
#20863=AXIS2_PLACEMENT_3D('',#33222,#25546,#25547);
#20864=AXIS2_PLACEMENT_3D('',#33223,#25548,#25549);
#20865=AXIS2_PLACEMENT_3D('',#33224,#25550,#25551);
#20866=AXIS2_PLACEMENT_3D('',#33225,#25552,#25553);
#20867=AXIS2_PLACEMENT_3D('',#33226,#25554,#25555);
#20868=AXIS2_PLACEMENT_3D('',#33227,#25556,#25557);
#20869=AXIS2_PLACEMENT_3D('',#33228,#25558,#25559);
#20870=AXIS2_PLACEMENT_3D('',#33229,#25560,#25561);
#20871=AXIS2_PLACEMENT_3D('',#33230,#25562,#25563);
#20872=AXIS2_PLACEMENT_3D('',#33231,#25564,#25565);
#20873=AXIS2_PLACEMENT_3D('',#33232,#25566,#25567);
#20874=AXIS2_PLACEMENT_3D('',#33233,#25568,#25569);
#20875=AXIS2_PLACEMENT_3D('',#33234,#25570,#25571);
#20876=AXIS2_PLACEMENT_3D('',#33235,#25572,#25573);
#20877=AXIS2_PLACEMENT_3D('',#33236,#25574,#25575);
#20878=AXIS2_PLACEMENT_3D('',#33237,#25576,#25577);
#20879=AXIS2_PLACEMENT_3D('',#33238,#25578,#25579);
#20880=AXIS2_PLACEMENT_3D('',#33239,#25580,#25581);
#20881=AXIS2_PLACEMENT_3D('',#33240,#25582,#25583);
#20882=AXIS2_PLACEMENT_3D('',#33241,#25584,#25585);
#20883=AXIS2_PLACEMENT_3D('',#33242,#25586,#25587);
#20884=AXIS2_PLACEMENT_3D('',#33243,#25588,#25589);
#20885=AXIS2_PLACEMENT_3D('',#33244,#25590,#25591);
#20886=AXIS2_PLACEMENT_3D('',#33245,#25592,#25593);
#20887=AXIS2_PLACEMENT_3D('',#33246,#25594,#25595);
#20888=AXIS2_PLACEMENT_3D('',#33247,#25596,#25597);
#20889=AXIS2_PLACEMENT_3D('',#33248,#25598,#25599);
#20890=AXIS2_PLACEMENT_3D('',#33249,#25600,#25601);
#20891=AXIS2_PLACEMENT_3D('',#33250,#25602,#25603);
#20892=AXIS2_PLACEMENT_3D('',#33251,#25604,#25605);
#20893=AXIS2_PLACEMENT_3D('',#33252,#25606,#25607);
#20894=AXIS2_PLACEMENT_3D('',#33253,#25608,#25609);
#20895=AXIS2_PLACEMENT_3D('',#33254,#25610,#25611);
#20896=AXIS2_PLACEMENT_3D('',#33255,#25612,#25613);
#20897=AXIS2_PLACEMENT_3D('',#33256,#25614,#25615);
#20898=AXIS2_PLACEMENT_3D('',#33257,#25616,#25617);
#20899=AXIS2_PLACEMENT_3D('',#33258,#25618,#25619);
#20900=AXIS2_PLACEMENT_3D('',#33259,#25620,#25621);
#20901=AXIS2_PLACEMENT_3D('',#33284,#25623,#25624);
#20902=AXIS2_PLACEMENT_3D('',#33289,#25625,#25626);
#20903=AXIS2_PLACEMENT_3D('',#33376,#25628,#25629);
#20904=AXIS2_PLACEMENT_3D('',#33466,#25631,#25632);
#20905=AXIS2_PLACEMENT_3D('',#33553,#25634,#25635);
#20906=AXIS2_PLACEMENT_3D('',#33640,#25637,#25638);
#20907=AXIS2_PLACEMENT_3D('',#33727,#25640,#25641);
#20908=AXIS2_PLACEMENT_3D('',#33814,#25643,#25644);
#20909=AXIS2_PLACEMENT_3D('',#33901,#25646,#25647);
#20910=AXIS2_PLACEMENT_3D('',#33973,#25649,#25650);
#20911=AXIS2_PLACEMENT_3D('',#34024,#25652,#25653);
#20912=AXIS2_PLACEMENT_3D('',#34072,#25655,#25656);
#20913=AXIS2_PLACEMENT_3D('',#34120,#25658,#25659);
#20914=AXIS2_PLACEMENT_3D('',#34171,#25661,#25662);
#20915=AXIS2_PLACEMENT_3D('',#34222,#25664,#25665);
#20916=AXIS2_PLACEMENT_3D('',#34270,#25667,#25668);
#20917=AXIS2_PLACEMENT_3D('',#34321,#25670,#25671);
#20918=AXIS2_PLACEMENT_3D('',#34372,#25673,#25674);
#20919=AXIS2_PLACEMENT_3D('',#34420,#25676,#25677);
#20920=AXIS2_PLACEMENT_3D('',#34468,#25679,#25680);
#20921=AXIS2_PLACEMENT_3D('',#34519,#25682,#25683);
#20922=AXIS2_PLACEMENT_3D('',#34570,#25685,#25686);
#20923=AXIS2_PLACEMENT_3D('',#34618,#25688,#25689);
#20924=AXIS2_PLACEMENT_3D('',#34669,#25691,#25692);
#20925=AXIS2_PLACEMENT_3D('',#34720,#25694,#25695);
#20926=AXIS2_PLACEMENT_3D('',#34768,#25697,#25698);
#20927=AXIS2_PLACEMENT_3D('',#34816,#25700,#25701);
#20928=AXIS2_PLACEMENT_3D('',#34867,#25703,#25704);
#20929=AXIS2_PLACEMENT_3D('',#34918,#25706,#25707);
#20930=AXIS2_PLACEMENT_3D('',#34966,#25709,#25710);
#20931=AXIS2_PLACEMENT_3D('',#35017,#25712,#25713);
#20932=AXIS2_PLACEMENT_3D('',#35068,#25715,#25716);
#20933=AXIS2_PLACEMENT_3D('',#35116,#25718,#25719);
#20934=AXIS2_PLACEMENT_3D('',#35164,#25721,#25722);
#20935=AXIS2_PLACEMENT_3D('',#35215,#25724,#25725);
#20936=AXIS2_PLACEMENT_3D('',#35266,#25727,#25728);
#20937=AXIS2_PLACEMENT_3D('',#35314,#25730,#25731);
#20938=AXIS2_PLACEMENT_3D('',#35365,#25733,#25734);
#20939=AXIS2_PLACEMENT_3D('',#35416,#25736,#25737);
#20940=AXIS2_PLACEMENT_3D('',#35464,#25739,#25740);
#20941=AXIS2_PLACEMENT_3D('',#35512,#25742,#25743);
#20942=AXIS2_PLACEMENT_3D('',#35563,#25745,#25746);
#20943=AXIS2_PLACEMENT_3D('',#35614,#25748,#25749);
#20944=AXIS2_PLACEMENT_3D('',#35662,#25751,#25752);
#20945=AXIS2_PLACEMENT_3D('',#35713,#25754,#25755);
#20946=AXIS2_PLACEMENT_3D('',#35764,#25757,#25758);
#20947=AXIS2_PLACEMENT_3D('',#35812,#25760,#25761);
#20948=AXIS2_PLACEMENT_3D('',#35860,#25763,#25764);
#20949=AXIS2_PLACEMENT_3D('',#35911,#25766,#25767);
#20950=AXIS2_PLACEMENT_3D('',#35962,#25769,#25770);
#20951=AXIS2_PLACEMENT_3D('',#36010,#25772,#25773);
#20952=AXIS2_PLACEMENT_3D('',#36061,#25775,#25776);
#20953=AXIS2_PLACEMENT_3D('',#36112,#25778,#25779);
#20954=AXIS2_PLACEMENT_3D('',#36160,#25781,#25782);
#20955=AXIS2_PLACEMENT_3D('',#36208,#25784,#25785);
#20956=AXIS2_PLACEMENT_3D('',#36259,#25787,#25788);
#20957=AXIS2_PLACEMENT_3D('',#36325,#25790,#25791);
#20958=AXIS2_PLACEMENT_3D('',#36415,#25793,#25794);
#20959=AXIS2_PLACEMENT_3D('',#36502,#25796,#25797);
#20960=AXIS2_PLACEMENT_3D('',#36589,#25799,#25800);
#20961=AXIS2_PLACEMENT_3D('',#36676,#25802,#25803);
#20962=AXIS2_PLACEMENT_3D('',#36763,#25805,#25806);
#20963=AXIS2_PLACEMENT_3D('',#36850,#25808,#25809);
#20964=AXIS2_PLACEMENT_3D('',#36940,#25811,#25812);
#20965=AXIS2_PLACEMENT_3D('',#36949,#25814,#25815);
#20966=AXIS2_PLACEMENT_3D('',#36950,#25816,#25817);
#20967=AXIS2_PLACEMENT_3D('',#36972,#25819,#25820);
#20968=AXIS2_PLACEMENT_3D('',#36986,#25821,#25822);
#20969=AXIS2_PLACEMENT_3D('',#37024,#25824,#25825);
#20970=AXIS2_PLACEMENT_3D('',#37060,#25827,#25828);
#20971=AXIS2_PLACEMENT_3D('',#37098,#25830,#25831);
#20972=AXIS2_PLACEMENT_3D('',#37134,#25833,#25834);
#20973=AXIS2_PLACEMENT_3D('',#37172,#25836,#25837);
#20974=AXIS2_PLACEMENT_3D('',#37209,#25839,#25840);
#20975=AXIS2_PLACEMENT_3D('',#37244,#25842,#25843);
#20976=AXIS2_PLACEMENT_3D('',#37271,#25845,#25846);
#20977=AXIS2_PLACEMENT_3D('',#37295,#25848,#25849);
#20978=AXIS2_PLACEMENT_3D('',#37319,#25851,#25852);
#20979=AXIS2_PLACEMENT_3D('',#37343,#25854,#25855);
#20980=AXIS2_PLACEMENT_3D('',#37369,#25857,#25858);
#20981=AXIS2_PLACEMENT_3D('',#37393,#25860,#25861);
#20982=AXIS2_PLACEMENT_3D('',#37417,#25863,#25864);
#20983=AXIS2_PLACEMENT_3D('',#37443,#25866,#25867);
#20984=AXIS2_PLACEMENT_3D('',#37467,#25869,#25870);
#20985=AXIS2_PLACEMENT_3D('',#37491,#25872,#25873);
#20986=AXIS2_PLACEMENT_3D('',#37515,#25875,#25876);
#20987=AXIS2_PLACEMENT_3D('',#37541,#25878,#25879);
#20988=AXIS2_PLACEMENT_3D('',#37565,#25881,#25882);
#20989=AXIS2_PLACEMENT_3D('',#37589,#25884,#25885);
#20990=AXIS2_PLACEMENT_3D('',#37615,#25887,#25888);
#20991=AXIS2_PLACEMENT_3D('',#37639,#25890,#25891);
#20992=AXIS2_PLACEMENT_3D('',#37663,#25893,#25894);
#20993=AXIS2_PLACEMENT_3D('',#37687,#25896,#25897);
#20994=AXIS2_PLACEMENT_3D('',#37713,#25899,#25900);
#20995=AXIS2_PLACEMENT_3D('',#37737,#25902,#25903);
#20996=AXIS2_PLACEMENT_3D('',#37761,#25905,#25906);
#20997=AXIS2_PLACEMENT_3D('',#37787,#25908,#25909);
#20998=AXIS2_PLACEMENT_3D('',#37811,#25911,#25912);
#20999=AXIS2_PLACEMENT_3D('',#37835,#25914,#25915);
#21000=AXIS2_PLACEMENT_3D('',#37859,#25917,#25918);
#21001=AXIS2_PLACEMENT_3D('',#37885,#25920,#25921);
#21002=AXIS2_PLACEMENT_3D('',#37909,#25923,#25924);
#21003=AXIS2_PLACEMENT_3D('',#37933,#25926,#25927);
#21004=AXIS2_PLACEMENT_3D('',#37959,#25929,#25930);
#21005=AXIS2_PLACEMENT_3D('',#37983,#25932,#25933);
#21006=AXIS2_PLACEMENT_3D('',#38007,#25935,#25936);
#21007=AXIS2_PLACEMENT_3D('',#38031,#25938,#25939);
#21008=AXIS2_PLACEMENT_3D('',#38057,#25941,#25942);
#21009=AXIS2_PLACEMENT_3D('',#38081,#25944,#25945);
#21010=AXIS2_PLACEMENT_3D('',#38105,#25947,#25948);
#21011=AXIS2_PLACEMENT_3D('',#38131,#25950,#25951);
#21012=AXIS2_PLACEMENT_3D('',#38155,#25953,#25954);
#21013=AXIS2_PLACEMENT_3D('',#38179,#25956,#25957);
#21014=AXIS2_PLACEMENT_3D('',#38203,#25959,#25960);
#21015=AXIS2_PLACEMENT_3D('',#38229,#25962,#25963);
#21016=AXIS2_PLACEMENT_3D('',#38253,#25965,#25966);
#21017=AXIS2_PLACEMENT_3D('',#38277,#25968,#25969);
#21018=AXIS2_PLACEMENT_3D('',#38303,#25971,#25972);
#21019=AXIS2_PLACEMENT_3D('',#38327,#25974,#25975);
#21020=AXIS2_PLACEMENT_3D('',#38351,#25977,#25978);
#21021=AXIS2_PLACEMENT_3D('',#38376,#25980,#25981);
#21022=AXIS2_PLACEMENT_3D('',#38403,#25983,#25984);
#21023=AXIS2_PLACEMENT_3D('',#38440,#25986,#25987);
#21024=AXIS2_PLACEMENT_3D('',#38476,#25989,#25990);
#21025=AXIS2_PLACEMENT_3D('',#38514,#25992,#25993);
#21026=AXIS2_PLACEMENT_3D('',#38550,#25995,#25996);
#21027=AXIS2_PLACEMENT_3D('',#38588,#25998,#25999);
#21028=AXIS2_PLACEMENT_3D('',#38625,#26001,#26002);
#21029=AXIS2_PLACEMENT_3D('',#38662,#26004,#26005);
#21030=AXIS2_PLACEMENT_3D('',#38664,#26006,#26007);
#21031=AXIS2_PLACEMENT_3D('',#38741,#26008,#26009);
#21032=AXIS2_PLACEMENT_3D('',#38742,#26010,#26011);
#21033=AXIS2_PLACEMENT_3D('',#38745,#26013,#26014);
#21034=AXIS2_PLACEMENT_3D('',#38746,#26015,#26016);
#21035=AXIS2_PLACEMENT_3D('',#40820,#26017,#26018);
#21036=AXIS2_PLACEMENT_3D('',#42875,#26019,#26020);
#21037=AXIS2_PLACEMENT_3D('',#42884,#26025,#26026);
#21038=AXIS2_PLACEMENT_3D('',#42886,#26027,#26028);
#21039=AXIS2_PLACEMENT_3D('',#42890,#26031,#26032);
#21040=AXIS2_PLACEMENT_3D('',#42894,#26035,#26036);
#21041=AXIS2_PLACEMENT_3D('',#42898,#26039,#26040);
#21042=AXIS2_PLACEMENT_3D('',#42899,#26041,#26042);
#21043=AXIS2_PLACEMENT_3D('',#42900,#26043,#26044);
#21044=AXIS2_PLACEMENT_3D('',#42902,#26045,#26046);
#21045=AXIS2_PLACEMENT_3D('',#42905,#26048,#26049);
#21046=AXIS2_PLACEMENT_3D('',#42906,#26050,#26051);
#21047=AXIS2_PLACEMENT_3D('',#42907,#26052,#26053);
#21048=AXIS2_PLACEMENT_3D('',#42909,#26054,#26055);
#21049=AXIS2_PLACEMENT_3D('',#42910,#26056,#26057);
#21050=AXIS2_PLACEMENT_3D('',#42911,#26058,#26059);
#21051=AXIS2_PLACEMENT_3D('',#42913,#26060,#26061);
#21052=AXIS2_PLACEMENT_3D('',#42915,#26063,#26064);
#21053=AXIS2_PLACEMENT_3D('',#42916,#26065,#26066);
#21054=AXIS2_PLACEMENT_3D('',#42917,#26067,#26068);
#21055=AXIS2_PLACEMENT_3D('',#42918,#26069,#26070);
#21056=AXIS2_PLACEMENT_3D('',#42920,#26071,#26072);
#21057=AXIS2_PLACEMENT_3D('',#42923,#26074,#26075);
#21058=AXIS2_PLACEMENT_3D('',#42924,#26076,#26077);
#21059=AXIS2_PLACEMENT_3D('',#42926,#26078,#26079);
#21060=AXIS2_PLACEMENT_3D('',#42929,#26081,#26082);
#21061=AXIS2_PLACEMENT_3D('',#42930,#26083,#26084);
#21062=AXIS2_PLACEMENT_3D('',#42931,#26085,#26086);
#21063=AXIS2_PLACEMENT_3D('',#42932,#26087,#26088);
#21064=AXIS2_PLACEMENT_3D('',#42933,#26089,#26090);
#21065=AXIS2_PLACEMENT_3D('',#42937,#26092,#26093);
#21066=AXIS2_PLACEMENT_3D('',#42938,#26094,#26095);
#21067=AXIS2_PLACEMENT_3D('',#42950,#26096,#26097);
#21068=AXIS2_PLACEMENT_3D('',#43012,#26099,#26100);
#21069=AXIS2_PLACEMENT_3D('',#43014,#26102,#26103);
#21070=AXIS2_PLACEMENT_3D('',#43016,#26104,#26105);
#21071=AXIS2_PLACEMENT_3D('',#43019,#26107,#26108);
#21072=AXIS2_PLACEMENT_3D('',#43020,#26109,#26110);
#21073=AXIS2_PLACEMENT_3D('',#43022,#26111,#26112);
#21074=AXIS2_PLACEMENT_3D('',#43025,#26114,#26115);
#21075=AXIS2_PLACEMENT_3D('',#43026,#26116,#26117);
#21076=AXIS2_PLACEMENT_3D('',#43027,#26118,#26119);
#21077=AXIS2_PLACEMENT_3D('',#43028,#26120,#26121);
#21078=AXIS2_PLACEMENT_3D('',#43029,#26122,#26123);
#21079=AXIS2_PLACEMENT_3D('',#43031,#26124,#26125);
#21080=AXIS2_PLACEMENT_3D('',#43034,#26127,#26128);
#21081=AXIS2_PLACEMENT_3D('',#43035,#26129,#26130);
#21082=AXIS2_PLACEMENT_3D('',#43039,#26132,#26133);
#21083=AXIS2_PLACEMENT_3D('',#43040,#26134,#26135);
#21084=AXIS2_PLACEMENT_3D('',#43050,#26136,#26137);
#21085=AXIS2_PLACEMENT_3D('',#43106,#26139,#26140);
#21086=AXIS2_PLACEMENT_3D('',#43108,#26142,#26143);
#21087=AXIS2_PLACEMENT_3D('',#43121,#26150,#26151);
#21088=AXIS2_PLACEMENT_3D('',#43127,#26155,#26156);
#21089=AXIS2_PLACEMENT_3D('',#43137,#26162,#26163);
#21090=AXIS2_PLACEMENT_3D('',#43139,#26164,#26165);
#21091=AXIS2_PLACEMENT_3D('',#43140,#26166,#26167);
#21092=AXIS2_PLACEMENT_3D('',#43141,#26168,#26169);
#21093=AXIS2_PLACEMENT_3D('',#43143,#26170,#26171);
#21094=AXIS2_PLACEMENT_3D('',#43144,#26172,#26173);
#21095=AXIS2_PLACEMENT_3D('',#43145,#26174,#26175);
#21096=AXIS2_PLACEMENT_3D('',#43147,#26177,#26178);
#21097=AXIS2_PLACEMENT_3D('',#43148,#26179,#26180);
#21098=AXIS2_PLACEMENT_3D('',#43149,#26181,#26182);
#21099=AXIS2_PLACEMENT_3D('',#43150,#26183,#26184);
#21100=AXIS2_PLACEMENT_3D('',#43151,#26185,#26186);
#21101=AXIS2_PLACEMENT_3D('',#43152,#26187,#26188);
#21102=AXIS2_PLACEMENT_3D('',#43153,#26189,#26190);
#21103=AXIS2_PLACEMENT_3D('',#43155,#26191,#26192);
#21104=AXIS2_PLACEMENT_3D('',#43158,#26194,#26195);
#21105=AXIS2_PLACEMENT_3D('',#43159,#26196,#26197);
#21106=AXIS2_PLACEMENT_3D('',#43161,#26198,#26199);
#21107=AXIS2_PLACEMENT_3D('',#43164,#26201,#26202);
#21108=AXIS2_PLACEMENT_3D('',#43165,#26203,#26204);
#21109=AXIS2_PLACEMENT_3D('',#43166,#26205,#26206);
#21110=AXIS2_PLACEMENT_3D('',#43167,#26207,#26208);
#21111=AXIS2_PLACEMENT_3D('',#43168,#26209,#26210);
#21112=AXIS2_PLACEMENT_3D('',#43170,#26211,#26212);
#21113=AXIS2_PLACEMENT_3D('',#43173,#26214,#26215);
#21114=AXIS2_PLACEMENT_3D('',#43174,#26216,#26217);
#21115=AXIS2_PLACEMENT_3D('',#43176,#26218,#26219);
#21116=AXIS2_PLACEMENT_3D('',#43179,#26221,#26222);
#21117=AXIS2_PLACEMENT_3D('',#43180,#26223,#26224);
#21118=AXIS2_PLACEMENT_3D('',#43181,#26225,#26226);
#21119=AXIS2_PLACEMENT_3D('',#43182,#26227,#26228);
#21120=AXIS2_PLACEMENT_3D('',#43183,#26229,#26230);
#21121=AXIS2_PLACEMENT_3D('',#43200,#26239,#26240);
#21122=AXIS2_PLACEMENT_3D('',#43206,#26244,#26245);
#21123=AXIS2_PLACEMENT_3D('',#43210,#26248,#26249);
#21124=AXIS2_PLACEMENT_3D('',#43214,#26252,#26253);
#21125=AXIS2_PLACEMENT_3D('',#43218,#26256,#26257);
#21126=AXIS2_PLACEMENT_3D('',#43226,#26262,#26263);
#21127=AXIS2_PLACEMENT_3D('',#43228,#26265,#26266);
#21128=AXIS2_PLACEMENT_3D('',#43230,#26268,#26269);
#21129=AXIS2_PLACEMENT_3D('',#43232,#26271,#26272);
#21130=AXIS2_PLACEMENT_3D('',#43233,#26273,#26274);
#21131=AXIS2_PLACEMENT_3D('',#43234,#26275,#26276);
#21132=AXIS2_PLACEMENT_3D('',#43243,#26281,#26282);
#21133=AXIS2_PLACEMENT_3D('',#43249,#26286,#26287);
#21134=AXIS2_PLACEMENT_3D('',#43255,#26291,#26292);
#21135=AXIS2_PLACEMENT_3D('',#43261,#26296,#26297);
#21136=AXIS2_PLACEMENT_3D('',#43267,#26301,#26302);
#21137=AXIS2_PLACEMENT_3D('',#43270,#26305,#26306);
#21138=AXIS2_PLACEMENT_3D('',#43271,#26307,#26308);
#21139=AXIS2_PLACEMENT_3D('',#43273,#26309,#26310);
#21140=AXIS2_PLACEMENT_3D('',#43274,#26311,#26312);
#21141=AXIS2_PLACEMENT_3D('',#43276,#26313,#26314);
#21142=AXIS2_PLACEMENT_3D('',#43278,#26316,#26317);
#21143=AXIS2_PLACEMENT_3D('',#43280,#26318,#26319);
#21144=AXIS2_PLACEMENT_3D('',#43282,#26321,#26322);
#21145=AXIS2_PLACEMENT_3D('',#43284,#26323,#26324);
#21146=AXIS2_PLACEMENT_3D('',#43286,#26326,#26327);
#21147=AXIS2_PLACEMENT_3D('',#43287,#26328,#26329);
#21148=AXIS2_PLACEMENT_3D('',#43288,#26330,#26331);
#21149=AXIS2_PLACEMENT_3D('',#43290,#26332,#26333);
#21150=AXIS2_PLACEMENT_3D('',#43293,#26335,#26336);
#21151=AXIS2_PLACEMENT_3D('',#43294,#26337,#26338);
#21152=AXIS2_PLACEMENT_3D('',#43296,#26339,#26340);
#21153=AXIS2_PLACEMENT_3D('',#43299,#26342,#26343);
#21154=AXIS2_PLACEMENT_3D('',#43300,#26344,#26345);
#21155=AXIS2_PLACEMENT_3D('',#43301,#26346,#26347);
#21156=AXIS2_PLACEMENT_3D('',#43302,#26348,#26349);
#21157=AXIS2_PLACEMENT_3D('',#43303,#26350,#26351);
#21158=AXIS2_PLACEMENT_3D('',#43305,#26352,#26353);
#21159=AXIS2_PLACEMENT_3D('',#43306,#26354,#26355);
#21160=AXIS2_PLACEMENT_3D('',#43308,#26356,#26357);
#21161=AXIS2_PLACEMENT_3D('',#43310,#26359,#26360);
#21162=AXIS2_PLACEMENT_3D('',#43312,#26361,#26362);
#21163=AXIS2_PLACEMENT_3D('',#43314,#26364,#26365);
#21164=AXIS2_PLACEMENT_3D('',#43316,#26366,#26367);
#21165=AXIS2_PLACEMENT_3D('',#43318,#26369,#26370);
#21166=AXIS2_PLACEMENT_3D('',#43320,#26371,#26372);
#21167=AXIS2_PLACEMENT_3D('',#43321,#26373,#26374);
#21168=AXIS2_PLACEMENT_3D('',#43323,#26375,#26376);
#21169=AXIS2_PLACEMENT_3D('',#43325,#26378,#26379);
#21170=AXIS2_PLACEMENT_3D('',#43327,#26380,#26381);
#21171=AXIS2_PLACEMENT_3D('',#43329,#26383,#26384);
#21172=AXIS2_PLACEMENT_3D('',#43331,#26385,#26386);
#21173=AXIS2_PLACEMENT_3D('',#43333,#26388,#26389);
#21174=AXIS2_PLACEMENT_3D('',#43334,#26390,#26391);
#21175=AXIS2_PLACEMENT_3D('',#43343,#26396,#26397);
#21176=AXIS2_PLACEMENT_3D('',#43349,#26401,#26402);
#21177=AXIS2_PLACEMENT_3D('',#43355,#26406,#26407);
#21178=AXIS2_PLACEMENT_3D('',#43361,#26411,#26412);
#21179=AXIS2_PLACEMENT_3D('',#43367,#26416,#26417);
#21180=AXIS2_PLACEMENT_3D('',#43370,#26420,#26421);
#21181=AXIS2_PLACEMENT_3D('',#43371,#26422,#26423);
#21182=AXIS2_PLACEMENT_3D('',#43372,#26424,#26425);
#21183=AXIS2_PLACEMENT_3D('',#43373,#26426,#26427);
#21184=AXIS2_PLACEMENT_3D('',#43374,#26428,#26429);
#21185=AXIS2_PLACEMENT_3D('',#43375,#26430,#26431);
#21186=AXIS2_PLACEMENT_3D('',#43376,#26432,#26433);
#21187=AXIS2_PLACEMENT_3D('',#43377,#26434,#26435);
#21188=AXIS2_PLACEMENT_3D('',#43378,#26436,#26437);
#21189=AXIS2_PLACEMENT_3D('',#43379,#26438,#26439);
#21190=AXIS2_PLACEMENT_3D('',#43380,#26440,#26441);
#21191=AXIS2_PLACEMENT_3D('',#43381,#26442,#26443);
#21192=AXIS2_PLACEMENT_3D('',#43382,#26444,#26445);
#21193=AXIS2_PLACEMENT_3D('',#43383,#26446,#26447);
#21194=AXIS2_PLACEMENT_3D('',#43384,#26448,#26449);
#21195=AXIS2_PLACEMENT_3D('',#43385,#26450,#26451);
#21196=DIRECTION('axis',(0.,0.,1.));
#21197=DIRECTION('refdir',(1.,0.,0.));
#21198=DIRECTION('axis',(0.,0.,1.));
#21199=DIRECTION('refdir',(1.,0.,0.));
#21200=DIRECTION('axis',(0.,0.,1.));
#21201=DIRECTION('refdir',(1.,0.,0.));
#21202=DIRECTION('center_axis',(0.,0.,1.));
#21203=DIRECTION('ref_axis',(1.,0.,0.));
#21204=DIRECTION('center_axis',(0.,0.,1.));
#21205=DIRECTION('ref_axis',(1.,0.,0.));
#21206=DIRECTION('',(0.,0.,1.));
#21207=DIRECTION('center_axis',(0.,0.,-1.));
#21208=DIRECTION('ref_axis',(1.,0.,0.));
#21209=DIRECTION('center_axis',(0.,1.,0.));
#21210=DIRECTION('ref_axis',(0.,0.,1.));
#21211=DIRECTION('',(0.,0.,-1.));
#21212=DIRECTION('',(1.,0.,0.));
#21213=DIRECTION('',(0.,0.,-1.));
#21214=DIRECTION('',(-1.,0.,0.));
#21215=DIRECTION('center_axis',(1.,0.,0.));
#21216=DIRECTION('ref_axis',(0.,0.,-1.));
#21217=DIRECTION('',(0.,0.,1.));
#21218=DIRECTION('',(0.,1.,0.));
#21219=DIRECTION('',(0.,1.,0.));
#21220=DIRECTION('center_axis',(0.,1.,0.));
#21221=DIRECTION('ref_axis',(1.,0.,0.));
#21222=DIRECTION('',(0.,0.,1.));
#21223=DIRECTION('',(1.,0.,0.));
#21224=DIRECTION('',(-1.,0.,0.));
#21225=DIRECTION('center_axis',(1.,0.,0.));
#21226=DIRECTION('ref_axis',(0.,1.,0.));
#21227=DIRECTION('',(0.,1.,0.));
#21228=DIRECTION('',(0.,0.,1.));
#21229=DIRECTION('',(0.,1.,0.));
#21230=DIRECTION('center_axis',(1.,0.,0.));
#21231=DIRECTION('ref_axis',(0.,1.,0.));
#21232=DIRECTION('',(0.,1.,0.));
#21233=DIRECTION('',(0.,0.,1.));
#21234=DIRECTION('',(0.,1.,0.));
#21235=DIRECTION('center_axis',(0.,0.,1.));
#21236=DIRECTION('ref_axis',(1.,0.,0.));
#21237=DIRECTION('center_axis',(0.,0.,1.));
#21238=DIRECTION('ref_axis',(1.,0.,0.));
#21239=DIRECTION('',(0.,0.,1.));
#21240=DIRECTION('center_axis',(0.,0.,-1.));
#21241=DIRECTION('ref_axis',(1.,0.,0.));
#21242=DIRECTION('center_axis',(0.,0.,1.));
#21243=DIRECTION('ref_axis',(1.,0.,0.));
#21244=DIRECTION('center_axis',(0.,0.,1.));
#21245=DIRECTION('ref_axis',(1.,0.,0.));
#21246=DIRECTION('center_axis',(0.,0.,1.));
#21247=DIRECTION('ref_axis',(1.,0.,0.));
#21248=DIRECTION('',(0.,0.,1.));
#21249=DIRECTION('center_axis',(0.,0.,-1.));
#21250=DIRECTION('ref_axis',(1.,0.,0.));
#21251=DIRECTION('center_axis',(0.,0.,1.));
#21252=DIRECTION('ref_axis',(1.,0.,0.));
#21253=DIRECTION('center_axis',(0.,0.,1.));
#21254=DIRECTION('ref_axis',(1.,0.,0.));
#21255=DIRECTION('center_axis',(0.,0.,1.));
#21256=DIRECTION('ref_axis',(1.,0.,0.));
#21257=DIRECTION('',(0.,0.,1.));
#21258=DIRECTION('center_axis',(0.,0.,-1.));
#21259=DIRECTION('ref_axis',(1.,0.,0.));
#21260=DIRECTION('center_axis',(0.,0.,1.));
#21261=DIRECTION('ref_axis',(1.,0.,0.));
#21262=DIRECTION('center_axis',(0.,0.,1.));
#21263=DIRECTION('ref_axis',(1.,0.,0.));
#21264=DIRECTION('center_axis',(0.,0.,1.));
#21265=DIRECTION('ref_axis',(1.,0.,0.));
#21266=DIRECTION('',(0.,0.,1.));
#21267=DIRECTION('center_axis',(0.,0.,-1.));
#21268=DIRECTION('ref_axis',(1.,0.,0.));
#21269=DIRECTION('center_axis',(0.,0.,1.));
#21270=DIRECTION('ref_axis',(1.,0.,0.));
#21271=DIRECTION('center_axis',(0.,0.,1.));
#21272=DIRECTION('ref_axis',(1.,0.,0.));
#21273=DIRECTION('center_axis',(0.,0.,1.));
#21274=DIRECTION('ref_axis',(1.,0.,0.));
#21275=DIRECTION('',(0.,0.,1.));
#21276=DIRECTION('center_axis',(0.,0.,-1.));
#21277=DIRECTION('ref_axis',(1.,0.,0.));
#21278=DIRECTION('center_axis',(0.,0.,1.));
#21279=DIRECTION('ref_axis',(1.,0.,0.));
#21280=DIRECTION('center_axis',(0.,0.,1.));
#21281=DIRECTION('ref_axis',(1.,0.,0.));
#21282=DIRECTION('',(0.,0.,1.));
#21283=DIRECTION('center_axis',(0.,0.,-1.));
#21284=DIRECTION('ref_axis',(1.,0.,0.));
#21285=DIRECTION('center_axis',(0.,0.,1.));
#21286=DIRECTION('ref_axis',(1.,0.,0.));
#21287=DIRECTION('center_axis',(0.,0.,1.));
#21288=DIRECTION('ref_axis',(1.,0.,0.));
#21289=DIRECTION('',(0.,0.,1.));
#21290=DIRECTION('center_axis',(0.,0.,-1.));
#21291=DIRECTION('ref_axis',(1.,0.,0.));
#21292=DIRECTION('center_axis',(0.,0.,1.));
#21293=DIRECTION('ref_axis',(1.,0.,0.));
#21294=DIRECTION('center_axis',(0.,0.,1.));
#21295=DIRECTION('ref_axis',(1.,0.,0.));
#21296=DIRECTION('',(0.,0.,1.));
#21297=DIRECTION('center_axis',(0.,0.,-1.));
#21298=DIRECTION('ref_axis',(1.,0.,0.));
#21299=DIRECTION('center_axis',(0.,0.,1.));
#21300=DIRECTION('ref_axis',(1.,0.,0.));
#21301=DIRECTION('center_axis',(0.,0.,1.));
#21302=DIRECTION('ref_axis',(1.,0.,0.));
#21303=DIRECTION('',(0.,0.,1.));
#21304=DIRECTION('center_axis',(0.,0.,-1.));
#21305=DIRECTION('ref_axis',(1.,0.,0.));
#21306=DIRECTION('center_axis',(0.,0.,1.));
#21307=DIRECTION('ref_axis',(1.,0.,0.));
#21308=DIRECTION('center_axis',(0.,0.,1.));
#21309=DIRECTION('ref_axis',(1.,0.,0.));
#21310=DIRECTION('',(0.,0.,1.));
#21311=DIRECTION('center_axis',(0.,0.,-1.));
#21312=DIRECTION('ref_axis',(1.,0.,0.));
#21313=DIRECTION('center_axis',(0.,0.,1.));
#21314=DIRECTION('ref_axis',(1.,0.,0.));
#21315=DIRECTION('center_axis',(0.,0.,1.));
#21316=DIRECTION('ref_axis',(1.,0.,0.));
#21317=DIRECTION('',(0.,0.,1.));
#21318=DIRECTION('center_axis',(0.,0.,-1.));
#21319=DIRECTION('ref_axis',(1.,0.,0.));
#21320=DIRECTION('center_axis',(0.,0.,1.));
#21321=DIRECTION('ref_axis',(1.,0.,0.));
#21322=DIRECTION('center_axis',(0.,0.,1.));
#21323=DIRECTION('ref_axis',(1.,0.,0.));
#21324=DIRECTION('',(0.,0.,1.));
#21325=DIRECTION('center_axis',(0.,0.,-1.));
#21326=DIRECTION('ref_axis',(1.,0.,0.));
#21327=DIRECTION('center_axis',(0.,0.,1.));
#21328=DIRECTION('ref_axis',(1.,0.,0.));
#21329=DIRECTION('center_axis',(0.,0.,1.));
#21330=DIRECTION('ref_axis',(1.,0.,0.));
#21331=DIRECTION('',(0.,0.,1.));
#21332=DIRECTION('center_axis',(0.,0.,-1.));
#21333=DIRECTION('ref_axis',(1.,0.,0.));
#21334=DIRECTION('center_axis',(0.,0.,1.));
#21335=DIRECTION('ref_axis',(1.,0.,0.));
#21336=DIRECTION('center_axis',(0.,0.,1.));
#21337=DIRECTION('ref_axis',(1.,0.,0.));
#21338=DIRECTION('',(0.,0.,1.));
#21339=DIRECTION('center_axis',(0.,0.,-1.));
#21340=DIRECTION('ref_axis',(1.,0.,0.));
#21341=DIRECTION('center_axis',(0.,0.,1.));
#21342=DIRECTION('ref_axis',(1.,0.,0.));
#21343=DIRECTION('center_axis',(0.,0.,1.));
#21344=DIRECTION('ref_axis',(1.,0.,0.));
#21345=DIRECTION('',(0.,0.,1.));
#21346=DIRECTION('center_axis',(0.,0.,-1.));
#21347=DIRECTION('ref_axis',(1.,0.,0.));
#21348=DIRECTION('center_axis',(0.,0.,1.));
#21349=DIRECTION('ref_axis',(1.,0.,0.));
#21350=DIRECTION('center_axis',(0.,0.,1.));
#21351=DIRECTION('ref_axis',(1.,0.,0.));
#21352=DIRECTION('',(0.,0.,1.));
#21353=DIRECTION('center_axis',(0.,0.,-1.));
#21354=DIRECTION('ref_axis',(1.,0.,0.));
#21355=DIRECTION('center_axis',(0.,0.,1.));
#21356=DIRECTION('ref_axis',(1.,0.,0.));
#21357=DIRECTION('center_axis',(0.,0.,1.));
#21358=DIRECTION('ref_axis',(1.,0.,0.));
#21359=DIRECTION('',(0.,0.,1.));
#21360=DIRECTION('center_axis',(0.,0.,-1.));
#21361=DIRECTION('ref_axis',(1.,0.,0.));
#21362=DIRECTION('center_axis',(0.,0.,1.));
#21363=DIRECTION('ref_axis',(1.,0.,0.));
#21364=DIRECTION('center_axis',(0.,0.,1.));
#21365=DIRECTION('ref_axis',(1.,0.,0.));
#21366=DIRECTION('',(0.,0.,1.));
#21367=DIRECTION('center_axis',(0.,0.,-1.));
#21368=DIRECTION('ref_axis',(1.,0.,0.));
#21369=DIRECTION('center_axis',(0.,0.,1.));
#21370=DIRECTION('ref_axis',(1.,0.,0.));
#21371=DIRECTION('center_axis',(0.,0.,1.));
#21372=DIRECTION('ref_axis',(1.,0.,0.));
#21373=DIRECTION('',(0.,0.,1.));
#21374=DIRECTION('center_axis',(0.,0.,-1.));
#21375=DIRECTION('ref_axis',(1.,0.,0.));
#21376=DIRECTION('center_axis',(0.,1.,0.));
#21377=DIRECTION('ref_axis',(-1.,0.,0.));
#21378=DIRECTION('',(-1.,0.,0.));
#21379=DIRECTION('',(0.,0.,1.));
#21380=DIRECTION('',(-1.,0.,0.));
#21381=DIRECTION('center_axis',(0.,-1.,0.));
#21382=DIRECTION('ref_axis',(1.,0.,0.));
#21383=DIRECTION('',(1.,0.,0.));
#21384=DIRECTION('',(1.,0.,0.));
#21385=DIRECTION('',(0.,0.,1.));
#21386=DIRECTION('center_axis',(-1.,0.,0.));
#21387=DIRECTION('ref_axis',(0.,-1.,0.));
#21388=DIRECTION('',(0.,-1.,0.));
#21389=DIRECTION('',(0.,-1.,0.));
#21390=DIRECTION('center_axis',(0.,0.,1.));
#21391=DIRECTION('ref_axis',(1.,0.,0.));
#21392=DIRECTION('center_axis',(0.,0.,1.));
#21393=DIRECTION('ref_axis',(1.,0.,0.));
#21394=DIRECTION('axis',(0.,0.,1.));
#21395=DIRECTION('refdir',(1.,0.,0.));
#21396=DIRECTION('center_axis',(0.,1.,0.));
#21397=DIRECTION('ref_axis',(-1.,0.,0.));
#21398=DIRECTION('',(-1.,0.,0.));
#21399=DIRECTION('',(0.,0.,1.));
#21400=DIRECTION('',(-1.,0.,0.));
#21401=DIRECTION('',(0.,0.,1.));
#21402=DIRECTION('center_axis',(1.,0.,0.));
#21403=DIRECTION('ref_axis',(0.,1.,0.));
#21404=DIRECTION('',(0.,1.,0.));
#21405=DIRECTION('',(0.,1.,0.));
#21406=DIRECTION('',(0.,0.,1.));
#21407=DIRECTION('center_axis',(0.,-1.,0.));
#21408=DIRECTION('ref_axis',(1.,0.,0.));
#21409=DIRECTION('',(1.,0.,0.));
#21410=DIRECTION('',(1.,0.,0.));
#21411=DIRECTION('',(0.,0.,1.));
#21412=DIRECTION('center_axis',(-1.,0.,0.));
#21413=DIRECTION('ref_axis',(0.,-1.,0.));
#21414=DIRECTION('',(0.,-1.,0.));
#21415=DIRECTION('',(0.,-1.,0.));
#21416=DIRECTION('center_axis',(0.,0.,1.));
#21417=DIRECTION('ref_axis',(1.,0.,0.));
#21418=DIRECTION('center_axis',(0.,0.,1.));
#21419=DIRECTION('ref_axis',(1.,0.,0.));
#21420=DIRECTION('axis',(0.,0.,1.));
#21421=DIRECTION('refdir',(1.,0.,0.));
#21422=DIRECTION('center_axis',(0.,1.,0.));
#21423=DIRECTION('ref_axis',(-1.,0.,0.));
#21424=DIRECTION('',(-1.,0.,0.));
#21425=DIRECTION('',(0.,0.,1.));
#21426=DIRECTION('',(-1.,0.,0.));
#21427=DIRECTION('',(0.,0.,1.));
#21428=DIRECTION('center_axis',(1.,0.,0.));
#21429=DIRECTION('ref_axis',(0.,1.,0.));
#21430=DIRECTION('',(0.,1.,0.));
#21431=DIRECTION('',(0.,1.,0.));
#21432=DIRECTION('',(0.,0.,1.));
#21433=DIRECTION('center_axis',(0.,-1.,0.));
#21434=DIRECTION('ref_axis',(1.,0.,0.));
#21435=DIRECTION('',(1.,0.,0.));
#21436=DIRECTION('',(1.,0.,0.));
#21437=DIRECTION('',(0.,0.,1.));
#21438=DIRECTION('center_axis',(-1.,0.,0.));
#21439=DIRECTION('ref_axis',(0.,-1.,0.));
#21440=DIRECTION('',(0.,-1.,0.));
#21441=DIRECTION('',(0.,-1.,0.));
#21442=DIRECTION('center_axis',(0.,0.,1.));
#21443=DIRECTION('ref_axis',(1.,0.,0.));
#21444=DIRECTION('center_axis',(0.,0.,1.));
#21445=DIRECTION('ref_axis',(1.,0.,0.));
#21446=DIRECTION('axis',(0.,0.,1.));
#21447=DIRECTION('refdir',(1.,0.,0.));
#21448=DIRECTION('center_axis',(0.,0.,1.));
#21449=DIRECTION('ref_axis',(1.,0.,0.));
#21450=DIRECTION('center_axis',(0.,0.,1.));
#21451=DIRECTION('ref_axis',(1.,0.,0.));
#21452=DIRECTION('',(0.,0.,1.));
#21453=DIRECTION('center_axis',(0.,0.,-1.));
#21454=DIRECTION('ref_axis',(1.,0.,0.));
#21455=DIRECTION('center_axis',(0.,0.,1.));
#21456=DIRECTION('ref_axis',(1.,0.,0.));
#21457=DIRECTION('center_axis',(0.,0.,1.));
#21458=DIRECTION('ref_axis',(1.,0.,0.));
#21459=DIRECTION('',(0.,0.,1.));
#21460=DIRECTION('center_axis',(0.,0.,-1.));
#21461=DIRECTION('ref_axis',(1.,0.,0.));
#21462=DIRECTION('center_axis',(0.,0.,1.));
#21463=DIRECTION('ref_axis',(1.,0.,0.));
#21464=DIRECTION('center_axis',(0.,0.,1.));
#21465=DIRECTION('ref_axis',(1.,0.,0.));
#21466=DIRECTION('',(0.,0.,1.));
#21467=DIRECTION('center_axis',(0.,0.,-1.));
#21468=DIRECTION('ref_axis',(1.,0.,0.));
#21469=DIRECTION('center_axis',(0.,0.,1.));
#21470=DIRECTION('ref_axis',(1.,0.,0.));
#21471=DIRECTION('center_axis',(0.,0.,1.));
#21472=DIRECTION('ref_axis',(1.,0.,0.));
#21473=DIRECTION('',(0.,0.,1.));
#21474=DIRECTION('center_axis',(0.,0.,-1.));
#21475=DIRECTION('ref_axis',(1.,0.,0.));
#21476=DIRECTION('center_axis',(0.,0.,1.));
#21477=DIRECTION('ref_axis',(1.,0.,0.));
#21478=DIRECTION('center_axis',(0.,0.,1.));
#21479=DIRECTION('ref_axis',(1.,0.,0.));
#21480=DIRECTION('',(0.,0.,1.));
#21481=DIRECTION('center_axis',(0.,0.,-1.));
#21482=DIRECTION('ref_axis',(1.,0.,0.));
#21483=DIRECTION('center_axis',(0.,0.,1.));
#21484=DIRECTION('ref_axis',(1.,0.,0.));
#21485=DIRECTION('center_axis',(0.,0.,1.));
#21486=DIRECTION('ref_axis',(1.,0.,0.));
#21487=DIRECTION('',(0.,0.,1.));
#21488=DIRECTION('center_axis',(0.,0.,-1.));
#21489=DIRECTION('ref_axis',(1.,0.,0.));
#21490=DIRECTION('center_axis',(0.,0.,1.));
#21491=DIRECTION('ref_axis',(1.,0.,0.));
#21492=DIRECTION('center_axis',(0.,0.,1.));
#21493=DIRECTION('ref_axis',(1.,0.,0.));
#21494=DIRECTION('',(0.,0.,1.));
#21495=DIRECTION('center_axis',(0.,0.,-1.));
#21496=DIRECTION('ref_axis',(1.,0.,0.));
#21497=DIRECTION('center_axis',(0.,0.,1.));
#21498=DIRECTION('ref_axis',(1.,0.,0.));
#21499=DIRECTION('center_axis',(0.,0.,1.));
#21500=DIRECTION('ref_axis',(1.,0.,0.));
#21501=DIRECTION('',(0.,0.,1.));
#21502=DIRECTION('center_axis',(0.,0.,-1.));
#21503=DIRECTION('ref_axis',(1.,0.,0.));
#21504=DIRECTION('center_axis',(0.,-1.,0.));
#21505=DIRECTION('ref_axis',(1.,0.,0.));
#21506=DIRECTION('',(-1.,0.,0.));
#21507=DIRECTION('',(0.,0.,1.));
#21508=DIRECTION('',(1.,0.,0.));
#21509=DIRECTION('',(0.,0.,1.));
#21510=DIRECTION('center_axis',(-1.,0.,0.));
#21511=DIRECTION('ref_axis',(0.,-1.,0.));
#21512=DIRECTION('',(0.,1.,0.));
#21513=DIRECTION('',(0.,-1.,0.));
#21514=DIRECTION('',(0.,0.,1.));
#21515=DIRECTION('center_axis',(0.,1.,0.));
#21516=DIRECTION('ref_axis',(-1.,0.,0.));
#21517=DIRECTION('',(1.,0.,0.));
#21518=DIRECTION('',(-1.,0.,0.));
#21519=DIRECTION('',(0.,0.,1.));
#21520=DIRECTION('center_axis',(1.,0.,0.));
#21521=DIRECTION('ref_axis',(0.,1.,0.));
#21522=DIRECTION('',(0.,-1.,0.));
#21523=DIRECTION('',(0.,1.,0.));
#21524=DIRECTION('center_axis',(0.,0.,1.));
#21525=DIRECTION('ref_axis',(1.,0.,0.));
#21526=DIRECTION('center_axis',(0.,0.,1.));
#21527=DIRECTION('ref_axis',(1.,0.,0.));
#21528=DIRECTION('',(0.,0.,1.));
#21529=DIRECTION('center_axis',(0.,0.,-1.));
#21530=DIRECTION('ref_axis',(1.,0.,0.));
#21531=DIRECTION('center_axis',(0.,0.,1.));
#21532=DIRECTION('ref_axis',(1.,0.,0.));
#21533=DIRECTION('center_axis',(0.,0.,1.));
#21534=DIRECTION('ref_axis',(1.,0.,0.));
#21535=DIRECTION('',(0.,0.,1.));
#21536=DIRECTION('center_axis',(0.,0.,-1.));
#21537=DIRECTION('ref_axis',(1.,0.,0.));
#21538=DIRECTION('center_axis',(0.,1.,0.));
#21539=DIRECTION('ref_axis',(-1.,0.,0.));
#21540=DIRECTION('',(-1.,0.,0.));
#21541=DIRECTION('',(0.,0.,1.));
#21542=DIRECTION('',(-1.,0.,0.));
#21543=DIRECTION('',(0.,0.,1.));
#21544=DIRECTION('center_axis',(1.,0.,0.));
#21545=DIRECTION('ref_axis',(0.,1.,0.));
#21546=DIRECTION('',(0.,1.,0.));
#21547=DIRECTION('',(0.,1.,0.));
#21548=DIRECTION('',(0.,0.,1.));
#21549=DIRECTION('center_axis',(0.,-1.,0.));
#21550=DIRECTION('ref_axis',(1.,0.,0.));
#21551=DIRECTION('',(1.,0.,0.));
#21552=DIRECTION('',(1.,0.,0.));
#21553=DIRECTION('',(0.,0.,1.));
#21554=DIRECTION('center_axis',(-1.,0.,0.));
#21555=DIRECTION('ref_axis',(0.,-1.,0.));
#21556=DIRECTION('',(0.,-1.,0.));
#21557=DIRECTION('',(0.,-1.,0.));
#21558=DIRECTION('center_axis',(0.,0.,1.));
#21559=DIRECTION('ref_axis',(1.,0.,0.));
#21560=DIRECTION('center_axis',(0.,0.,1.));
#21561=DIRECTION('ref_axis',(1.,0.,0.));
#21562=DIRECTION('axis',(0.,0.,1.));
#21563=DIRECTION('refdir',(1.,0.,0.));
#21564=DIRECTION('center_axis',(1.,0.,0.));
#21565=DIRECTION('ref_axis',(0.,0.,-1.));
#21566=DIRECTION('center_axis',(1.,0.,0.));
#21567=DIRECTION('ref_axis',(0.,0.,-1.));
#21568=DIRECTION('',(1.,0.,0.));
#21569=DIRECTION('center_axis',(-1.,0.,0.));
#21570=DIRECTION('ref_axis',(0.,0.,-1.));
#21571=DIRECTION('center_axis',(1.,0.,0.));
#21572=DIRECTION('ref_axis',(0.,0.,-1.));
#21573=DIRECTION('center_axis',(1.,0.,0.));
#21574=DIRECTION('ref_axis',(0.,0.,-1.));
#21575=DIRECTION('',(1.,0.,0.));
#21576=DIRECTION('center_axis',(-1.,0.,0.));
#21577=DIRECTION('ref_axis',(0.,0.,-1.));
#21578=DIRECTION('center_axis',(0.,0.,1.));
#21579=DIRECTION('ref_axis',(1.,0.,0.));
#21580=DIRECTION('center_axis',(0.,0.,1.));
#21581=DIRECTION('ref_axis',(1.,0.,0.));
#21582=DIRECTION('',(0.,0.,1.));
#21583=DIRECTION('center_axis',(0.,0.,-1.));
#21584=DIRECTION('ref_axis',(1.,0.,0.));
#21585=DIRECTION('center_axis',(0.,0.,1.));
#21586=DIRECTION('ref_axis',(1.,0.,0.));
#21587=DIRECTION('center_axis',(0.,0.,1.));
#21588=DIRECTION('ref_axis',(1.,0.,0.));
#21589=DIRECTION('center_axis',(0.,0.,1.));
#21590=DIRECTION('ref_axis',(1.,0.,0.));
#21591=DIRECTION('',(0.,0.,1.));
#21592=DIRECTION('center_axis',(0.,0.,-1.));
#21593=DIRECTION('ref_axis',(1.,0.,0.));
#21594=DIRECTION('center_axis',(0.,0.,1.));
#21595=DIRECTION('ref_axis',(1.,0.,0.));
#21596=DIRECTION('center_axis',(0.,0.,1.));
#21597=DIRECTION('ref_axis',(1.,0.,0.));
#21598=DIRECTION('center_axis',(0.,0.,1.));
#21599=DIRECTION('ref_axis',(1.,0.,0.));
#21600=DIRECTION('',(0.,0.,1.));
#21601=DIRECTION('center_axis',(0.,0.,1.));
#21602=DIRECTION('ref_axis',(1.,0.,0.));
#21603=DIRECTION('center_axis',(0.,0.,1.));
#21604=DIRECTION('ref_axis',(1.,0.,0.));
#21605=DIRECTION('center_axis',(0.,0.,1.));
#21606=DIRECTION('ref_axis',(1.,0.,0.));
#21607=DIRECTION('center_axis',(0.,0.,1.));
#21608=DIRECTION('ref_axis',(1.,0.,0.));
#21609=DIRECTION('',(0.,0.,1.));
#21610=DIRECTION('center_axis',(0.,0.,1.));
#21611=DIRECTION('ref_axis',(1.,0.,0.));
#21612=DIRECTION('center_axis',(0.,0.,1.));
#21613=DIRECTION('ref_axis',(1.,0.,0.));
#21614=DIRECTION('center_axis',(0.,1.,0.));
#21615=DIRECTION('ref_axis',(-1.,0.,0.));
#21616=DIRECTION('',(-1.,0.,0.));
#21617=DIRECTION('',(0.,0.,1.));
#21618=DIRECTION('',(-1.,0.,0.));
#21619=DIRECTION('',(0.,0.,1.));
#21620=DIRECTION('center_axis',(1.,0.,0.));
#21621=DIRECTION('ref_axis',(0.,1.,0.));
#21622=DIRECTION('',(0.,1.,0.));
#21623=DIRECTION('',(0.,1.,0.));
#21624=DIRECTION('',(0.,0.,1.));
#21625=DIRECTION('center_axis',(0.,-1.,0.));
#21626=DIRECTION('ref_axis',(1.,0.,0.));
#21627=DIRECTION('',(1.,0.,0.));
#21628=DIRECTION('',(1.,0.,0.));
#21629=DIRECTION('',(0.,0.,1.));
#21630=DIRECTION('center_axis',(-1.,0.,0.));
#21631=DIRECTION('ref_axis',(0.,-1.,0.));
#21632=DIRECTION('',(0.,-1.,0.));
#21633=DIRECTION('',(0.,-1.,0.));
#21634=DIRECTION('center_axis',(0.,0.,1.));
#21635=DIRECTION('ref_axis',(1.,0.,0.));
#21636=DIRECTION('center_axis',(0.,0.,1.));
#21637=DIRECTION('ref_axis',(1.,0.,0.));
#21638=DIRECTION('axis',(0.,0.,1.));
#21639=DIRECTION('refdir',(1.,0.,0.));
#21640=DIRECTION('center_axis',(1.,0.,0.));
#21641=DIRECTION('ref_axis',(0.,0.,-1.));
#21642=DIRECTION('center_axis',(1.,0.,0.));
#21643=DIRECTION('ref_axis',(0.,0.,-1.));
#21644=DIRECTION('',(1.,0.,0.));
#21645=DIRECTION('center_axis',(-1.,0.,0.));
#21646=DIRECTION('ref_axis',(0.,0.,-1.));
#21647=DIRECTION('center_axis',(1.,0.,0.));
#21648=DIRECTION('ref_axis',(0.,0.,-1.));
#21649=DIRECTION('center_axis',(1.,0.,0.));
#21650=DIRECTION('ref_axis',(0.,0.,-1.));
#21651=DIRECTION('',(1.,0.,0.));
#21652=DIRECTION('center_axis',(-1.,0.,0.));
#21653=DIRECTION('ref_axis',(0.,0.,-1.));
#21654=DIRECTION('center_axis',(0.,0.,1.));
#21655=DIRECTION('ref_axis',(1.,0.,0.));
#21656=DIRECTION('center_axis',(0.,0.,1.));
#21657=DIRECTION('ref_axis',(1.,0.,0.));
#21658=DIRECTION('',(0.,0.,1.));
#21659=DIRECTION('center_axis',(0.,0.,-1.));
#21660=DIRECTION('ref_axis',(1.,0.,0.));
#21661=DIRECTION('center_axis',(0.,0.,1.));
#21662=DIRECTION('ref_axis',(1.,0.,0.));
#21663=DIRECTION('center_axis',(0.,0.,1.));
#21664=DIRECTION('ref_axis',(1.,0.,0.));
#21665=DIRECTION('center_axis',(0.,0.,1.));
#21666=DIRECTION('ref_axis',(1.,0.,0.));
#21667=DIRECTION('',(0.,0.,1.));
#21668=DIRECTION('center_axis',(0.,0.,-1.));
#21669=DIRECTION('ref_axis',(1.,0.,0.));
#21670=DIRECTION('center_axis',(0.,0.,1.));
#21671=DIRECTION('ref_axis',(1.,0.,0.));
#21672=DIRECTION('center_axis',(0.,0.,1.));
#21673=DIRECTION('ref_axis',(1.,0.,0.));
#21674=DIRECTION('center_axis',(0.,0.,1.));
#21675=DIRECTION('ref_axis',(1.,0.,0.));
#21676=DIRECTION('',(0.,0.,1.));
#21677=DIRECTION('center_axis',(0.,0.,1.));
#21678=DIRECTION('ref_axis',(1.,0.,0.));
#21679=DIRECTION('center_axis',(0.,0.,1.));
#21680=DIRECTION('ref_axis',(1.,0.,0.));
#21681=DIRECTION('center_axis',(0.,0.,1.));
#21682=DIRECTION('ref_axis',(1.,0.,0.));
#21683=DIRECTION('center_axis',(0.,0.,1.));
#21684=DIRECTION('ref_axis',(1.,0.,0.));
#21685=DIRECTION('',(0.,0.,1.));
#21686=DIRECTION('center_axis',(0.,0.,1.));
#21687=DIRECTION('ref_axis',(1.,0.,0.));
#21688=DIRECTION('center_axis',(0.,0.,1.));
#21689=DIRECTION('ref_axis',(1.,0.,0.));
#21690=DIRECTION('center_axis',(0.,1.,0.));
#21691=DIRECTION('ref_axis',(-1.,0.,0.));
#21692=DIRECTION('',(-1.,0.,0.));
#21693=DIRECTION('',(0.,0.,1.));
#21694=DIRECTION('',(-1.,0.,0.));
#21695=DIRECTION('',(0.,0.,1.));
#21696=DIRECTION('center_axis',(1.,0.,0.));
#21697=DIRECTION('ref_axis',(0.,1.,0.));
#21698=DIRECTION('',(0.,1.,0.));
#21699=DIRECTION('',(0.,1.,0.));
#21700=DIRECTION('',(0.,0.,1.));
#21701=DIRECTION('center_axis',(0.,-1.,0.));
#21702=DIRECTION('ref_axis',(1.,0.,0.));
#21703=DIRECTION('',(1.,0.,0.));
#21704=DIRECTION('',(1.,0.,0.));
#21705=DIRECTION('',(0.,0.,1.));
#21706=DIRECTION('center_axis',(-1.,0.,0.));
#21707=DIRECTION('ref_axis',(0.,-1.,0.));
#21708=DIRECTION('',(0.,-1.,0.));
#21709=DIRECTION('',(0.,-1.,0.));
#21710=DIRECTION('center_axis',(0.,0.,1.));
#21711=DIRECTION('ref_axis',(1.,0.,0.));
#21712=DIRECTION('center_axis',(0.,0.,1.));
#21713=DIRECTION('ref_axis',(1.,0.,0.));
#21714=DIRECTION('axis',(0.,0.,1.));
#21715=DIRECTION('refdir',(1.,0.,0.));
#21716=DIRECTION('center_axis',(0.,0.,1.));
#21717=DIRECTION('ref_axis',(1.,0.,0.));
#21718=DIRECTION('center_axis',(0.,0.,1.));
#21719=DIRECTION('ref_axis',(1.,0.,0.));
#21720=DIRECTION('',(0.,0.,1.));
#21721=DIRECTION('center_axis',(0.,0.,1.));
#21722=DIRECTION('ref_axis',(1.,0.,0.));
#21723=DIRECTION('center_axis',(0.,0.,1.));
#21724=DIRECTION('ref_axis',(1.,0.,0.));
#21725=DIRECTION('center_axis',(0.,0.,1.));
#21726=DIRECTION('ref_axis',(1.,0.,0.));
#21727=DIRECTION('center_axis',(0.,0.,1.));
#21728=DIRECTION('ref_axis',(1.,0.,0.));
#21729=DIRECTION('',(0.,0.,1.));
#21730=DIRECTION('center_axis',(0.,0.,1.));
#21731=DIRECTION('ref_axis',(1.,0.,0.));
#21732=DIRECTION('center_axis',(0.,0.,1.));
#21733=DIRECTION('ref_axis',(1.,0.,0.));
#21734=DIRECTION('center_axis',(0.,1.,0.));
#21735=DIRECTION('ref_axis',(1.,0.,0.));
#21736=DIRECTION('center_axis',(0.,1.,0.));
#21737=DIRECTION('ref_axis',(1.,0.,0.));
#21738=DIRECTION('',(0.,1.,0.));
#21739=DIRECTION('center_axis',(0.,-1.,0.));
#21740=DIRECTION('ref_axis',(1.,0.,0.));
#21741=DIRECTION('center_axis',(0.,1.,0.));
#21742=DIRECTION('ref_axis',(1.,0.,0.));
#21743=DIRECTION('center_axis',(0.,1.,0.));
#21744=DIRECTION('ref_axis',(1.,0.,0.));
#21745=DIRECTION('',(0.,1.,0.));
#21746=DIRECTION('center_axis',(0.,-1.,0.));
#21747=DIRECTION('ref_axis',(1.,0.,0.));
#21748=DIRECTION('center_axis',(0.,1.,0.));
#21749=DIRECTION('ref_axis',(-1.,0.,0.));
#21750=DIRECTION('',(-1.,0.,0.));
#21751=DIRECTION('',(0.,0.,1.));
#21752=DIRECTION('',(-1.,0.,0.));
#21753=DIRECTION('',(0.,0.,1.));
#21754=DIRECTION('center_axis',(1.,0.,0.));
#21755=DIRECTION('ref_axis',(0.,1.,0.));
#21756=DIRECTION('',(0.,1.,0.));
#21757=DIRECTION('',(0.,1.,0.));
#21758=DIRECTION('',(0.,0.,1.));
#21759=DIRECTION('center_axis',(0.,-1.,0.));
#21760=DIRECTION('ref_axis',(1.,0.,0.));
#21761=DIRECTION('',(1.,0.,0.));
#21762=DIRECTION('',(1.,0.,0.));
#21763=DIRECTION('',(0.,0.,1.));
#21764=DIRECTION('center_axis',(-1.,0.,0.));
#21765=DIRECTION('ref_axis',(0.,-1.,0.));
#21766=DIRECTION('',(0.,-1.,0.));
#21767=DIRECTION('',(0.,-1.,0.));
#21768=DIRECTION('center_axis',(0.,0.,1.));
#21769=DIRECTION('ref_axis',(1.,0.,0.));
#21770=DIRECTION('center_axis',(0.,0.,1.));
#21771=DIRECTION('ref_axis',(1.,0.,0.));
#21772=DIRECTION('axis',(0.,0.,1.));
#21773=DIRECTION('refdir',(1.,0.,0.));
#21774=DIRECTION('center_axis',(0.,0.,1.));
#21775=DIRECTION('ref_axis',(1.,0.,0.));
#21776=DIRECTION('center_axis',(0.,0.,1.));
#21777=DIRECTION('ref_axis',(1.,0.,0.));
#21778=DIRECTION('',(0.,0.,1.));
#21779=DIRECTION('center_axis',(0.,0.,-1.));
#21780=DIRECTION('ref_axis',(1.,0.,0.));
#21781=DIRECTION('center_axis',(0.,0.,1.));
#21782=DIRECTION('ref_axis',(1.,0.,0.));
#21783=DIRECTION('center_axis',(0.,0.,1.));
#21784=DIRECTION('ref_axis',(1.,0.,0.));
#21785=DIRECTION('',(0.,0.,1.));
#21786=DIRECTION('center_axis',(0.,0.,-1.));
#21787=DIRECTION('ref_axis',(1.,0.,0.));
#21788=DIRECTION('center_axis',(0.,1.,0.));
#21789=DIRECTION('ref_axis',(1.,0.,0.));
#21790=DIRECTION('center_axis',(0.,1.,0.));
#21791=DIRECTION('ref_axis',(1.,0.,0.));
#21792=DIRECTION('',(0.,1.,0.));
#21793=DIRECTION('center_axis',(0.,1.,0.));
#21794=DIRECTION('ref_axis',(1.,0.,0.));
#21795=DIRECTION('',(0.,1.,0.));
#21796=DIRECTION('center_axis',(0.,-1.,0.));
#21797=DIRECTION('ref_axis',(1.,0.,0.));
#21798=DIRECTION('',(0.,-1.,0.));
#21799=DIRECTION('center_axis',(0.,1.,0.));
#21800=DIRECTION('ref_axis',(1.,0.,0.));
#21801=DIRECTION('center_axis',(0.,1.,0.));
#21802=DIRECTION('ref_axis',(1.,0.,0.));
#21803=DIRECTION('',(-1.,0.,0.));
#21804=DIRECTION('center_axis',(0.,1.,0.));
#21805=DIRECTION('ref_axis',(1.,0.,0.));
#21806=DIRECTION('center_axis',(0.,1.,0.));
#21807=DIRECTION('ref_axis',(1.,0.,0.));
#21808=DIRECTION('',(0.,1.,0.));
#21809=DIRECTION('center_axis',(0.,1.,0.));
#21810=DIRECTION('ref_axis',(1.,0.,0.));
#21811=DIRECTION('',(0.,1.,0.));
#21812=DIRECTION('center_axis',(0.,-1.,0.));
#21813=DIRECTION('ref_axis',(1.,0.,0.));
#21814=DIRECTION('',(0.,-1.,0.));
#21815=DIRECTION('center_axis',(0.,1.,0.));
#21816=DIRECTION('ref_axis',(1.,0.,0.));
#21817=DIRECTION('center_axis',(0.,1.,0.));
#21818=DIRECTION('ref_axis',(1.,0.,0.));
#21819=DIRECTION('',(-1.,0.,0.));
#21820=DIRECTION('center_axis',(0.,1.,0.));
#21821=DIRECTION('ref_axis',(-1.,0.,0.));
#21822=DIRECTION('',(1.,0.,0.));
#21823=DIRECTION('',(1.,0.,0.));
#21824=DIRECTION('',(0.,0.,1.));
#21825=DIRECTION('',(-1.,0.,0.));
#21826=DIRECTION('',(0.,0.,1.));
#21827=DIRECTION('',(1.,0.,0.));
#21828=DIRECTION('center_axis',(0.,0.,-1.));
#21829=DIRECTION('ref_axis',(-1.,0.,0.));
#21830=DIRECTION('',(0.,1.,0.));
#21831=DIRECTION('',(-1.,0.,0.));
#21832=DIRECTION('',(0.,1.,0.));
#21833=DIRECTION('center_axis',(0.,1.,0.));
#21834=DIRECTION('ref_axis',(0.,0.,1.));
#21835=DIRECTION('',(1.,0.,0.));
#21836=DIRECTION('',(0.,0.,-1.));
#21837=DIRECTION('',(0.,0.,1.));
#21838=DIRECTION('center_axis',(1.,0.,0.));
#21839=DIRECTION('ref_axis',(0.,1.,0.));
#21840=DIRECTION('',(0.,0.,1.));
#21841=DIRECTION('',(0.,1.,0.));
#21842=DIRECTION('',(0.,1.,0.));
#21843=DIRECTION('center_axis',(0.,-1.,0.));
#21844=DIRECTION('ref_axis',(1.,0.,0.));
#21845=DIRECTION('',(0.,0.,1.));
#21846=DIRECTION('',(1.,0.,0.));
#21847=DIRECTION('',(1.,0.,0.));
#21848=DIRECTION('center_axis',(-1.,0.,0.));
#21849=DIRECTION('ref_axis',(0.,-1.,0.));
#21850=DIRECTION('',(0.,-1.,0.));
#21851=DIRECTION('',(0.,1.,0.));
#21852=DIRECTION('center_axis',(0.,0.,1.));
#21853=DIRECTION('ref_axis',(1.,0.,0.));
#21854=DIRECTION('center_axis',(0.,0.,1.));
#21855=DIRECTION('ref_axis',(1.,0.,0.));
#21856=DIRECTION('axis',(0.,0.,1.));
#21857=DIRECTION('refdir',(1.,0.,0.));
#21858=DIRECTION('center_axis',(0.,0.,1.));
#21859=DIRECTION('ref_axis',(1.,0.,0.));
#21860=DIRECTION('center_axis',(0.,0.,1.));
#21861=DIRECTION('ref_axis',(1.,0.,0.));
#21862=DIRECTION('',(0.,0.,1.));
#21863=DIRECTION('center_axis',(0.,0.,1.));
#21864=DIRECTION('ref_axis',(1.,0.,0.));
#21865=DIRECTION('center_axis',(0.,0.,1.));
#21866=DIRECTION('ref_axis',(1.,0.,0.));
#21867=DIRECTION('center_axis',(0.,0.,1.));
#21868=DIRECTION('ref_axis',(1.,0.,0.));
#21869=DIRECTION('center_axis',(0.,0.,1.));
#21870=DIRECTION('ref_axis',(1.,0.,0.));
#21871=DIRECTION('',(0.,0.,1.));
#21872=DIRECTION('center_axis',(0.,0.,1.));
#21873=DIRECTION('ref_axis',(1.,0.,0.));
#21874=DIRECTION('center_axis',(0.,0.,1.));
#21875=DIRECTION('ref_axis',(1.,0.,0.));
#21876=DIRECTION('center_axis',(0.,1.,0.));
#21877=DIRECTION('ref_axis',(1.,0.,0.));
#21878=DIRECTION('center_axis',(0.,1.,0.));
#21879=DIRECTION('ref_axis',(1.,0.,0.));
#21880=DIRECTION('',(0.,1.,0.));
#21881=DIRECTION('center_axis',(0.,-1.,0.));
#21882=DIRECTION('ref_axis',(1.,0.,0.));
#21883=DIRECTION('center_axis',(0.,1.,0.));
#21884=DIRECTION('ref_axis',(1.,0.,0.));
#21885=DIRECTION('center_axis',(0.,1.,0.));
#21886=DIRECTION('ref_axis',(1.,0.,0.));
#21887=DIRECTION('',(0.,1.,0.));
#21888=DIRECTION('center_axis',(0.,-1.,0.));
#21889=DIRECTION('ref_axis',(1.,0.,0.));
#21890=DIRECTION('center_axis',(0.,1.,0.));
#21891=DIRECTION('ref_axis',(-1.,0.,0.));
#21892=DIRECTION('',(-1.,0.,0.));
#21893=DIRECTION('',(0.,0.,1.));
#21894=DIRECTION('',(-1.,0.,0.));
#21895=DIRECTION('',(0.,0.,1.));
#21896=DIRECTION('center_axis',(1.,0.,0.));
#21897=DIRECTION('ref_axis',(0.,1.,0.));
#21898=DIRECTION('',(0.,1.,0.));
#21899=DIRECTION('',(0.,1.,0.));
#21900=DIRECTION('',(0.,0.,1.));
#21901=DIRECTION('center_axis',(0.,-1.,0.));
#21902=DIRECTION('ref_axis',(1.,0.,0.));
#21903=DIRECTION('',(1.,0.,0.));
#21904=DIRECTION('',(1.,0.,0.));
#21905=DIRECTION('',(0.,0.,1.));
#21906=DIRECTION('center_axis',(-1.,0.,0.));
#21907=DIRECTION('ref_axis',(0.,-1.,0.));
#21908=DIRECTION('',(0.,-1.,0.));
#21909=DIRECTION('',(0.,-1.,0.));
#21910=DIRECTION('center_axis',(0.,0.,1.));
#21911=DIRECTION('ref_axis',(1.,0.,0.));
#21912=DIRECTION('center_axis',(0.,0.,1.));
#21913=DIRECTION('ref_axis',(1.,0.,0.));
#21914=DIRECTION('axis',(0.,0.,1.));
#21915=DIRECTION('refdir',(1.,0.,0.));
#21916=DIRECTION('center_axis',(0.,0.,1.));
#21917=DIRECTION('ref_axis',(1.,0.,0.));
#21918=DIRECTION('center_axis',(0.,0.,1.));
#21919=DIRECTION('ref_axis',(1.,0.,0.));
#21920=DIRECTION('',(0.,0.,1.));
#21921=DIRECTION('center_axis',(0.,0.,-1.));
#21922=DIRECTION('ref_axis',(1.,0.,0.));
#21923=DIRECTION('center_axis',(0.,0.,1.));
#21924=DIRECTION('ref_axis',(1.,0.,0.));
#21925=DIRECTION('center_axis',(0.,0.,1.));
#21926=DIRECTION('ref_axis',(1.,0.,0.));
#21927=DIRECTION('',(0.,0.,1.));
#21928=DIRECTION('center_axis',(0.,0.,-1.));
#21929=DIRECTION('ref_axis',(1.,0.,0.));
#21930=DIRECTION('center_axis',(0.,1.,0.));
#21931=DIRECTION('ref_axis',(1.,0.,0.));
#21932=DIRECTION('center_axis',(0.,1.,0.));
#21933=DIRECTION('ref_axis',(1.,0.,0.));
#21934=DIRECTION('',(0.,1.,0.));
#21935=DIRECTION('center_axis',(0.,1.,0.));
#21936=DIRECTION('ref_axis',(1.,0.,0.));
#21937=DIRECTION('',(0.,1.,0.));
#21938=DIRECTION('center_axis',(0.,-1.,0.));
#21939=DIRECTION('ref_axis',(1.,0.,0.));
#21940=DIRECTION('',(0.,-1.,0.));
#21941=DIRECTION('center_axis',(0.,1.,0.));
#21942=DIRECTION('ref_axis',(1.,0.,0.));
#21943=DIRECTION('center_axis',(0.,1.,0.));
#21944=DIRECTION('ref_axis',(1.,0.,0.));
#21945=DIRECTION('',(-1.,0.,0.));
#21946=DIRECTION('center_axis',(0.,1.,0.));
#21947=DIRECTION('ref_axis',(1.,0.,0.));
#21948=DIRECTION('center_axis',(0.,1.,0.));
#21949=DIRECTION('ref_axis',(1.,0.,0.));
#21950=DIRECTION('',(0.,1.,0.));
#21951=DIRECTION('center_axis',(0.,1.,0.));
#21952=DIRECTION('ref_axis',(1.,0.,0.));
#21953=DIRECTION('',(0.,1.,0.));
#21954=DIRECTION('center_axis',(0.,-1.,0.));
#21955=DIRECTION('ref_axis',(1.,0.,0.));
#21956=DIRECTION('',(0.,-1.,0.));
#21957=DIRECTION('center_axis',(0.,1.,0.));
#21958=DIRECTION('ref_axis',(1.,0.,0.));
#21959=DIRECTION('center_axis',(0.,1.,0.));
#21960=DIRECTION('ref_axis',(1.,0.,0.));
#21961=DIRECTION('',(-1.,0.,0.));
#21962=DIRECTION('center_axis',(0.,1.,0.));
#21963=DIRECTION('ref_axis',(-1.,0.,0.));
#21964=DIRECTION('',(1.,0.,0.));
#21965=DIRECTION('',(1.,0.,0.));
#21966=DIRECTION('',(0.,0.,1.));
#21967=DIRECTION('',(-1.,0.,0.));
#21968=DIRECTION('',(0.,0.,1.));
#21969=DIRECTION('',(1.,0.,0.));
#21970=DIRECTION('center_axis',(0.,0.,-1.));
#21971=DIRECTION('ref_axis',(-1.,0.,0.));
#21972=DIRECTION('',(0.,1.,0.));
#21973=DIRECTION('',(-1.,0.,0.));
#21974=DIRECTION('',(0.,1.,0.));
#21975=DIRECTION('center_axis',(0.,1.,0.));
#21976=DIRECTION('ref_axis',(0.,0.,1.));
#21977=DIRECTION('',(1.,0.,0.));
#21978=DIRECTION('',(0.,0.,-1.));
#21979=DIRECTION('',(0.,0.,1.));
#21980=DIRECTION('center_axis',(1.,0.,0.));
#21981=DIRECTION('ref_axis',(0.,1.,0.));
#21982=DIRECTION('',(0.,0.,1.));
#21983=DIRECTION('',(0.,1.,0.));
#21984=DIRECTION('',(0.,1.,0.));
#21985=DIRECTION('center_axis',(0.,-1.,0.));
#21986=DIRECTION('ref_axis',(1.,0.,0.));
#21987=DIRECTION('',(0.,0.,1.));
#21988=DIRECTION('',(1.,0.,0.));
#21989=DIRECTION('',(1.,0.,0.));
#21990=DIRECTION('center_axis',(-1.,0.,0.));
#21991=DIRECTION('ref_axis',(0.,-1.,0.));
#21992=DIRECTION('',(0.,-1.,0.));
#21993=DIRECTION('',(0.,1.,0.));
#21994=DIRECTION('center_axis',(0.,0.,1.));
#21995=DIRECTION('ref_axis',(1.,0.,0.));
#21996=DIRECTION('center_axis',(0.,0.,1.));
#21997=DIRECTION('ref_axis',(1.,0.,0.));
#21998=DIRECTION('axis',(0.,0.,1.));
#21999=DIRECTION('refdir',(1.,0.,0.));
#22000=DIRECTION('center_axis',(0.,0.,1.));
#22001=DIRECTION('ref_axis',(1.,0.,0.));
#22002=DIRECTION('center_axis',(0.,0.,1.));
#22003=DIRECTION('ref_axis',(1.,0.,0.));
#22004=DIRECTION('',(0.,0.,1.));
#22005=DIRECTION('center_axis',(0.,0.,-1.));
#22006=DIRECTION('ref_axis',(1.,0.,0.));
#22007=DIRECTION('center_axis',(0.,0.,1.));
#22008=DIRECTION('ref_axis',(1.,0.,0.));
#22009=DIRECTION('center_axis',(0.,0.,1.));
#22010=DIRECTION('ref_axis',(1.,0.,0.));
#22011=DIRECTION('',(0.,0.,1.));
#22012=DIRECTION('center_axis',(0.,0.,-1.));
#22013=DIRECTION('ref_axis',(1.,0.,0.));
#22014=DIRECTION('center_axis',(0.,0.,1.));
#22015=DIRECTION('ref_axis',(1.,0.,0.));
#22016=DIRECTION('center_axis',(0.,0.,1.));
#22017=DIRECTION('ref_axis',(1.,0.,0.));
#22018=DIRECTION('',(0.,0.,1.));
#22019=DIRECTION('center_axis',(0.,0.,-1.));
#22020=DIRECTION('ref_axis',(1.,0.,0.));
#22021=DIRECTION('center_axis',(0.,0.,1.));
#22022=DIRECTION('ref_axis',(1.,0.,0.));
#22023=DIRECTION('center_axis',(0.,0.,1.));
#22024=DIRECTION('ref_axis',(1.,0.,0.));
#22025=DIRECTION('',(0.,0.,1.));
#22026=DIRECTION('center_axis',(0.,0.,1.));
#22027=DIRECTION('ref_axis',(1.,0.,0.));
#22028=DIRECTION('center_axis',(0.,0.,1.));
#22029=DIRECTION('ref_axis',(1.,0.,0.));
#22030=DIRECTION('center_axis',(0.,0.,1.));
#22031=DIRECTION('ref_axis',(1.,0.,0.));
#22032=DIRECTION('center_axis',(0.,0.,1.));
#22033=DIRECTION('ref_axis',(1.,0.,0.));
#22034=DIRECTION('',(0.,0.,1.));
#22035=DIRECTION('center_axis',(0.,0.,1.));
#22036=DIRECTION('ref_axis',(1.,0.,0.));
#22037=DIRECTION('center_axis',(0.,0.,1.));
#22038=DIRECTION('ref_axis',(1.,0.,0.));
#22039=DIRECTION('center_axis',(0.,0.,1.));
#22040=DIRECTION('ref_axis',(1.,0.,0.));
#22041=DIRECTION('center_axis',(0.,0.,1.));
#22042=DIRECTION('ref_axis',(1.,0.,0.));
#22043=DIRECTION('',(0.,0.,1.));
#22044=DIRECTION('center_axis',(0.,0.,1.));
#22045=DIRECTION('ref_axis',(1.,0.,0.));
#22046=DIRECTION('center_axis',(0.,0.,1.));
#22047=DIRECTION('ref_axis',(1.,0.,0.));
#22048=DIRECTION('center_axis',(0.,0.,1.));
#22049=DIRECTION('ref_axis',(1.,0.,0.));
#22050=DIRECTION('center_axis',(0.,0.,1.));
#22051=DIRECTION('ref_axis',(1.,0.,0.));
#22052=DIRECTION('',(0.,0.,1.));
#22053=DIRECTION('center_axis',(0.,0.,1.));
#22054=DIRECTION('ref_axis',(1.,0.,0.));
#22055=DIRECTION('center_axis',(0.,0.,1.));
#22056=DIRECTION('ref_axis',(1.,0.,0.));
#22057=DIRECTION('center_axis',(0.,0.,1.));
#22058=DIRECTION('ref_axis',(1.,0.,0.));
#22059=DIRECTION('center_axis',(0.,0.,1.));
#22060=DIRECTION('ref_axis',(1.,0.,0.));
#22061=DIRECTION('',(0.,0.,1.));
#22062=DIRECTION('center_axis',(0.,0.,1.));
#22063=DIRECTION('ref_axis',(1.,0.,0.));
#22064=DIRECTION('center_axis',(0.,0.,1.));
#22065=DIRECTION('ref_axis',(1.,0.,0.));
#22066=DIRECTION('center_axis',(0.,0.,-1.));
#22067=DIRECTION('ref_axis',(1.,0.,0.));
#22068=DIRECTION('center_axis',(0.,0.,1.));
#22069=DIRECTION('ref_axis',(1.,0.,0.));
#22070=DIRECTION('',(0.,0.,1.));
#22071=DIRECTION('center_axis',(0.,0.,-1.));
#22072=DIRECTION('ref_axis',(1.,0.,0.));
#22073=DIRECTION('center_axis',(0.,0.,1.));
#22074=DIRECTION('ref_axis',(1.,0.,0.));
#22075=DIRECTION('center_axis',(0.,0.,1.));
#22076=DIRECTION('ref_axis',(1.,0.,0.));
#22077=DIRECTION('',(0.,0.,1.));
#22078=DIRECTION('center_axis',(0.,0.,1.));
#22079=DIRECTION('ref_axis',(1.,0.,0.));
#22080=DIRECTION('center_axis',(0.,0.,1.));
#22081=DIRECTION('ref_axis',(1.,0.,0.));
#22082=DIRECTION('center_axis',(0.,1.,0.));
#22083=DIRECTION('ref_axis',(-1.,0.,0.));
#22084=DIRECTION('',(-1.,0.,0.));
#22085=DIRECTION('',(0.,0.,1.));
#22086=DIRECTION('',(-1.,0.,0.));
#22087=DIRECTION('',(0.,0.,1.));
#22088=DIRECTION('center_axis',(1.,0.,0.));
#22089=DIRECTION('ref_axis',(0.,1.,0.));
#22090=DIRECTION('',(0.,1.,0.));
#22091=DIRECTION('',(0.,1.,0.));
#22092=DIRECTION('',(0.,0.,1.));
#22093=DIRECTION('center_axis',(0.,-1.,0.));
#22094=DIRECTION('ref_axis',(1.,0.,0.));
#22095=DIRECTION('',(1.,0.,0.));
#22096=DIRECTION('',(1.,0.,0.));
#22097=DIRECTION('',(0.,0.,1.));
#22098=DIRECTION('center_axis',(-1.,0.,0.));
#22099=DIRECTION('ref_axis',(0.,-1.,0.));
#22100=DIRECTION('',(0.,-1.,0.));
#22101=DIRECTION('',(0.,-1.,0.));
#22102=DIRECTION('center_axis',(0.,0.,1.));
#22103=DIRECTION('ref_axis',(1.,0.,0.));
#22104=DIRECTION('center_axis',(0.,0.,1.));
#22105=DIRECTION('ref_axis',(1.,0.,0.));
#22106=DIRECTION('axis',(0.,0.,1.));
#22107=DIRECTION('refdir',(1.,0.,0.));
#22108=DIRECTION('center_axis',(0.,0.,1.));
#22109=DIRECTION('ref_axis',(1.,0.,0.));
#22110=DIRECTION('center_axis',(0.,0.,1.));
#22111=DIRECTION('ref_axis',(1.,0.,0.));
#22112=DIRECTION('',(0.,0.,1.));
#22113=DIRECTION('center_axis',(0.,0.,-1.));
#22114=DIRECTION('ref_axis',(1.,0.,0.));
#22115=DIRECTION('center_axis',(0.,0.,1.));
#22116=DIRECTION('ref_axis',(1.,0.,0.));
#22117=DIRECTION('center_axis',(0.,0.,1.));
#22118=DIRECTION('ref_axis',(1.,0.,0.));
#22119=DIRECTION('',(0.,0.,1.));
#22120=DIRECTION('center_axis',(0.,0.,-1.));
#22121=DIRECTION('ref_axis',(1.,0.,0.));
#22122=DIRECTION('center_axis',(0.,0.,1.));
#22123=DIRECTION('ref_axis',(1.,0.,0.));
#22124=DIRECTION('center_axis',(0.,0.,1.));
#22125=DIRECTION('ref_axis',(1.,0.,0.));
#22126=DIRECTION('',(0.,0.,1.));
#22127=DIRECTION('center_axis',(0.,0.,-1.));
#22128=DIRECTION('ref_axis',(1.,0.,0.));
#22129=DIRECTION('center_axis',(0.,0.,1.));
#22130=DIRECTION('ref_axis',(1.,0.,0.));
#22131=DIRECTION('center_axis',(0.,0.,1.));
#22132=DIRECTION('ref_axis',(1.,0.,0.));
#22133=DIRECTION('',(0.,0.,1.));
#22134=DIRECTION('center_axis',(0.,0.,-1.));
#22135=DIRECTION('ref_axis',(1.,0.,0.));
#22136=DIRECTION('center_axis',(0.,0.,1.));
#22137=DIRECTION('ref_axis',(1.,0.,0.));
#22138=DIRECTION('center_axis',(0.,0.,1.));
#22139=DIRECTION('ref_axis',(1.,0.,0.));
#22140=DIRECTION('',(0.,0.,1.));
#22141=DIRECTION('center_axis',(0.,0.,-1.));
#22142=DIRECTION('ref_axis',(1.,0.,0.));
#22143=DIRECTION('center_axis',(1.,0.,0.));
#22144=DIRECTION('ref_axis',(0.,0.,-1.));
#22145=DIRECTION('center_axis',(1.,0.,0.));
#22146=DIRECTION('ref_axis',(0.,0.,-1.));
#22147=DIRECTION('',(1.,0.,0.));
#22148=DIRECTION('center_axis',(-1.,0.,0.));
#22149=DIRECTION('ref_axis',(0.,0.,-1.));
#22150=DIRECTION('center_axis',(1.,0.,0.));
#22151=DIRECTION('ref_axis',(0.,0.,-1.));
#22152=DIRECTION('center_axis',(1.,0.,0.));
#22153=DIRECTION('ref_axis',(0.,0.,-1.));
#22154=DIRECTION('center_axis',(1.,0.,0.));
#22155=DIRECTION('ref_axis',(0.,0.,-1.));
#22156=DIRECTION('',(1.,0.,0.));
#22157=DIRECTION('center_axis',(-1.,0.,0.));
#22158=DIRECTION('ref_axis',(0.,0.,-1.));
#22159=DIRECTION('center_axis',(1.,0.,0.));
#22160=DIRECTION('ref_axis',(0.,0.,-1.));
#22161=DIRECTION('center_axis',(1.,0.,0.));
#22162=DIRECTION('ref_axis',(0.,0.,-1.));
#22163=DIRECTION('center_axis',(1.,0.,0.));
#22164=DIRECTION('ref_axis',(0.,0.,-1.));
#22165=DIRECTION('',(1.,0.,0.));
#22166=DIRECTION('center_axis',(1.,0.,0.));
#22167=DIRECTION('ref_axis',(0.,0.,-1.));
#22168=DIRECTION('center_axis',(1.,0.,0.));
#22169=DIRECTION('ref_axis',(0.,0.,-1.));
#22170=DIRECTION('center_axis',(1.,0.,0.));
#22171=DIRECTION('ref_axis',(0.,0.,-1.));
#22172=DIRECTION('center_axis',(1.,0.,0.));
#22173=DIRECTION('ref_axis',(0.,0.,-1.));
#22174=DIRECTION('',(1.,0.,0.));
#22175=DIRECTION('center_axis',(1.,0.,0.));
#22176=DIRECTION('ref_axis',(0.,0.,-1.));
#22177=DIRECTION('center_axis',(1.,0.,0.));
#22178=DIRECTION('ref_axis',(0.,0.,-1.));
#22179=DIRECTION('center_axis',(0.,0.,1.));
#22180=DIRECTION('ref_axis',(1.,0.,0.));
#22181=DIRECTION('center_axis',(0.,0.,1.));
#22182=DIRECTION('ref_axis',(1.,0.,0.));
#22183=DIRECTION('',(0.,0.,1.));
#22184=DIRECTION('center_axis',(0.,0.,-1.));
#22185=DIRECTION('ref_axis',(1.,0.,0.));
#22186=DIRECTION('center_axis',(0.,0.,1.));
#22187=DIRECTION('ref_axis',(1.,0.,0.));
#22188=DIRECTION('center_axis',(0.,0.,1.));
#22189=DIRECTION('ref_axis',(1.,0.,0.));
#22190=DIRECTION('center_axis',(0.,0.,1.));
#22191=DIRECTION('ref_axis',(1.,0.,0.));
#22192=DIRECTION('center_axis',(0.,0.,1.));
#22193=DIRECTION('ref_axis',(1.,0.,0.));
#22194=DIRECTION('',(0.,0.,1.));
#22195=DIRECTION('center_axis',(0.,0.,1.));
#22196=DIRECTION('ref_axis',(1.,0.,0.));
#22197=DIRECTION('',(0.,0.,1.));
#22198=DIRECTION('center_axis',(0.,0.,1.));
#22199=DIRECTION('ref_axis',(1.,0.,0.));
#22200=DIRECTION('',(0.,0.,-1.));
#22201=DIRECTION('center_axis',(0.,0.,-1.));
#22202=DIRECTION('ref_axis',(1.,0.,0.));
#22203=DIRECTION('center_axis',(0.,0.,1.));
#22204=DIRECTION('ref_axis',(1.,0.,0.));
#22205=DIRECTION('',(0.,0.,1.));
#22206=DIRECTION('center_axis',(0.,0.,1.));
#22207=DIRECTION('ref_axis',(1.,0.,0.));
#22208=DIRECTION('',(0.,0.,-1.));
#22209=DIRECTION('center_axis',(0.,0.,-1.));
#22210=DIRECTION('ref_axis',(1.,0.,0.));
#22211=DIRECTION('center_axis',(1.,0.,0.));
#22212=DIRECTION('ref_axis',(0.,1.,0.));
#22213=DIRECTION('',(0.,1.,0.));
#22214=DIRECTION('',(0.,0.,1.));
#22215=DIRECTION('',(0.,1.,0.));
#22216=DIRECTION('center_axis',(0.,0.,1.));
#22217=DIRECTION('ref_axis',(1.,0.,0.));
#22218=DIRECTION('',(0.,-1.,0.));
#22219=DIRECTION('',(-1.,0.,0.));
#22220=DIRECTION('',(1.,0.,0.));
#22221=DIRECTION('center_axis',(0.,-1.,0.));
#22222=DIRECTION('ref_axis',(1.,0.,0.));
#22223=DIRECTION('',(1.,0.,0.));
#22224=DIRECTION('center_axis',(0.,1.,0.));
#22225=DIRECTION('ref_axis',(-1.,0.,0.));
#22226=DIRECTION('',(0.,0.,1.));
#22227=DIRECTION('',(-1.,0.,0.));
#22228=DIRECTION('center_axis',(-1.,0.,0.));
#22229=DIRECTION('ref_axis',(0.,-1.,0.));
#22230=DIRECTION('',(0.,-1.,0.));
#22231=DIRECTION('center_axis',(0.,0.,1.));
#22232=DIRECTION('ref_axis',(1.,0.,0.));
#22233=DIRECTION('axis',(0.,0.,1.));
#22234=DIRECTION('refdir',(1.,0.,0.));
#22235=DIRECTION('center_axis',(0.,0.,1.));
#22236=DIRECTION('ref_axis',(1.,0.,0.));
#22237=DIRECTION('center_axis',(0.,0.,1.));
#22238=DIRECTION('ref_axis',(1.,0.,0.));
#22239=DIRECTION('',(0.,0.,1.));
#22240=DIRECTION('center_axis',(0.,0.,-1.));
#22241=DIRECTION('ref_axis',(1.,0.,0.));
#22242=DIRECTION('center_axis',(0.,0.,1.));
#22243=DIRECTION('ref_axis',(1.,0.,0.));
#22244=DIRECTION('center_axis',(0.,0.,1.));
#22245=DIRECTION('ref_axis',(1.,0.,0.));
#22246=DIRECTION('',(0.,0.,1.));
#22247=DIRECTION('center_axis',(0.,0.,-1.));
#22248=DIRECTION('ref_axis',(1.,0.,0.));
#22249=DIRECTION('center_axis',(0.,0.,1.));
#22250=DIRECTION('ref_axis',(1.,0.,0.));
#22251=DIRECTION('center_axis',(0.,0.,1.));
#22252=DIRECTION('ref_axis',(1.,0.,0.));
#22253=DIRECTION('',(0.,0.,1.));
#22254=DIRECTION('center_axis',(0.,0.,-1.));
#22255=DIRECTION('ref_axis',(1.,0.,0.));
#22256=DIRECTION('center_axis',(0.,0.,1.));
#22257=DIRECTION('ref_axis',(1.,0.,0.));
#22258=DIRECTION('center_axis',(0.,0.,1.));
#22259=DIRECTION('ref_axis',(1.,0.,0.));
#22260=DIRECTION('',(0.,0.,-1.));
#22261=DIRECTION('center_axis',(0.,0.,-1.));
#22262=DIRECTION('ref_axis',(1.,0.,0.));
#22263=DIRECTION('center_axis',(0.,0.,1.));
#22264=DIRECTION('ref_axis',(1.,0.,0.));
#22265=DIRECTION('center_axis',(0.,0.,-1.));
#22266=DIRECTION('ref_axis',(1.,0.,0.));
#22267=DIRECTION('center_axis',(0.,0.,1.));
#22268=DIRECTION('ref_axis',(1.,0.,0.));
#22269=DIRECTION('',(0.,0.,-1.));
#22270=DIRECTION('center_axis',(0.,0.,-1.));
#22271=DIRECTION('ref_axis',(1.,0.,0.));
#22272=DIRECTION('center_axis',(0.,0.,1.));
#22273=DIRECTION('ref_axis',(1.,0.,0.));
#22274=DIRECTION('center_axis',(0.,0.,1.));
#22275=DIRECTION('ref_axis',(1.,0.,0.));
#22276=DIRECTION('',(0.,0.,-1.));
#22277=DIRECTION('center_axis',(0.,0.,1.));
#22278=DIRECTION('ref_axis',(1.,0.,0.));
#22279=DIRECTION('center_axis',(0.,0.,1.));
#22280=DIRECTION('ref_axis',(1.,0.,0.));
#22281=DIRECTION('center_axis',(0.,0.,1.));
#22282=DIRECTION('ref_axis',(1.,0.,0.));
#22283=DIRECTION('axis',(0.,0.,1.));
#22284=DIRECTION('refdir',(1.,0.,0.));
#22285=DIRECTION('center_axis',(0.,0.,1.));
#22286=DIRECTION('ref_axis',(1.,0.,0.));
#22287=DIRECTION('center_axis',(0.,0.,1.));
#22288=DIRECTION('ref_axis',(1.,0.,0.));
#22289=DIRECTION('',(0.,0.,1.));
#22290=DIRECTION('center_axis',(0.,0.,-1.));
#22291=DIRECTION('ref_axis',(1.,0.,0.));
#22292=DIRECTION('center_axis',(0.,0.,1.));
#22293=DIRECTION('ref_axis',(1.,0.,0.));
#22294=DIRECTION('center_axis',(0.,0.,1.));
#22295=DIRECTION('ref_axis',(1.,0.,0.));
#22296=DIRECTION('',(0.,0.,1.));
#22297=DIRECTION('center_axis',(0.,0.,-1.));
#22298=DIRECTION('ref_axis',(1.,0.,0.));
#22299=DIRECTION('center_axis',(0.,0.,1.));
#22300=DIRECTION('ref_axis',(1.,0.,0.));
#22301=DIRECTION('center_axis',(0.,0.,1.));
#22302=DIRECTION('ref_axis',(1.,0.,0.));
#22303=DIRECTION('',(0.,0.,1.));
#22304=DIRECTION('center_axis',(0.,0.,-1.));
#22305=DIRECTION('ref_axis',(1.,0.,0.));
#22306=DIRECTION('center_axis',(0.,0.,1.));
#22307=DIRECTION('ref_axis',(1.,0.,0.));
#22308=DIRECTION('center_axis',(0.,0.,1.));
#22309=DIRECTION('ref_axis',(1.,0.,0.));
#22310=DIRECTION('',(0.,0.,-1.));
#22311=DIRECTION('center_axis',(0.,0.,1.));
#22312=DIRECTION('ref_axis',(1.,0.,0.));
#22313=DIRECTION('center_axis',(0.,0.,1.));
#22314=DIRECTION('ref_axis',(1.,0.,0.));
#22315=DIRECTION('center_axis',(0.,0.,-1.));
#22316=DIRECTION('ref_axis',(1.,0.,0.));
#22317=DIRECTION('center_axis',(0.,0.,1.));
#22318=DIRECTION('ref_axis',(1.,0.,0.));
#22319=DIRECTION('center_axis',(0.,0.,-1.));
#22320=DIRECTION('ref_axis',(1.,0.,0.));
#22321=DIRECTION('',(0.,0.,-1.));
#22322=DIRECTION('center_axis',(0.,0.,1.));
#22323=DIRECTION('ref_axis',(1.,0.,0.));
#22324=DIRECTION('center_axis',(0.,0.,1.));
#22325=DIRECTION('ref_axis',(1.,0.,0.));
#22326=DIRECTION('',(0.,0.,-1.));
#22327=DIRECTION('center_axis',(0.,0.,1.));
#22328=DIRECTION('ref_axis',(1.,0.,0.));
#22329=DIRECTION('center_axis',(0.,0.,1.));
#22330=DIRECTION('ref_axis',(1.,0.,0.));
#22331=DIRECTION('center_axis',(0.,0.,1.));
#22332=DIRECTION('ref_axis',(1.,0.,0.));
#22333=DIRECTION('axis',(0.,0.,1.));
#22334=DIRECTION('refdir',(1.,0.,0.));
#22335=DIRECTION('center_axis',(0.,0.,1.));
#22336=DIRECTION('ref_axis',(1.,0.,0.));
#22337=DIRECTION('center_axis',(0.,0.,1.));
#22338=DIRECTION('ref_axis',(1.,0.,0.));
#22339=DIRECTION('',(0.,0.,1.));
#22340=DIRECTION('center_axis',(0.,0.,1.));
#22341=DIRECTION('ref_axis',(1.,0.,0.));
#22342=DIRECTION('center_axis',(0.,0.,1.));
#22343=DIRECTION('ref_axis',(1.,0.,0.));
#22344=DIRECTION('center_axis',(0.,0.,1.));
#22345=DIRECTION('ref_axis',(1.,0.,0.));
#22346=DIRECTION('center_axis',(0.,0.,1.));
#22347=DIRECTION('ref_axis',(1.,0.,0.));
#22348=DIRECTION('',(0.,0.,-1.));
#22349=DIRECTION('center_axis',(0.,0.,1.));
#22350=DIRECTION('ref_axis',(1.,0.,0.));
#22351=DIRECTION('center_axis',(0.,0.,1.));
#22352=DIRECTION('ref_axis',(1.,0.,0.));
#22353=DIRECTION('center_axis',(0.,0.,1.));
#22354=DIRECTION('ref_axis',(1.,0.,0.));
#22355=DIRECTION('axis',(0.,0.,1.));
#22356=DIRECTION('refdir',(1.,0.,0.));
#22357=DIRECTION('center_axis',(0.,0.,1.));
#22358=DIRECTION('ref_axis',(1.,0.,0.));
#22359=DIRECTION('center_axis',(0.,0.,1.));
#22360=DIRECTION('ref_axis',(1.,0.,0.));
#22361=DIRECTION('',(0.,0.,1.));
#22362=DIRECTION('center_axis',(0.,0.,-1.));
#22363=DIRECTION('ref_axis',(1.,0.,0.));
#22364=DIRECTION('center_axis',(0.,0.,1.));
#22365=DIRECTION('ref_axis',(1.,0.,0.));
#22366=DIRECTION('center_axis',(0.,0.,1.));
#22367=DIRECTION('ref_axis',(1.,0.,0.));
#22368=DIRECTION('center_axis',(0.,0.,1.));
#22369=DIRECTION('ref_axis',(1.,0.,0.));
#22370=DIRECTION('',(0.,0.,-1.));
#22371=DIRECTION('center_axis',(0.,0.,1.));
#22372=DIRECTION('ref_axis',(1.,0.,0.));
#22373=DIRECTION('center_axis',(0.,0.,1.));
#22374=DIRECTION('ref_axis',(1.,0.,0.));
#22375=DIRECTION('center_axis',(0.,0.,1.));
#22376=DIRECTION('ref_axis',(1.,0.,0.));
#22377=DIRECTION('axis',(0.,0.,1.));
#22378=DIRECTION('refdir',(1.,0.,0.));
#22379=DIRECTION('center_axis',(0.,0.,1.));
#22380=DIRECTION('ref_axis',(1.,0.,0.));
#22381=DIRECTION('center_axis',(0.,0.,1.));
#22382=DIRECTION('ref_axis',(1.,0.,0.));
#22383=DIRECTION('',(0.,0.,1.));
#22384=DIRECTION('center_axis',(0.,0.,1.));
#22385=DIRECTION('ref_axis',(1.,0.,0.));
#22386=DIRECTION('center_axis',(0.,0.,1.));
#22387=DIRECTION('ref_axis',(1.,0.,0.));
#22388=DIRECTION('center_axis',(0.,0.,1.));
#22389=DIRECTION('ref_axis',(1.,0.,0.));
#22390=DIRECTION('center_axis',(0.,0.,1.));
#22391=DIRECTION('ref_axis',(1.,0.,0.));
#22392=DIRECTION('',(0.,0.,-1.));
#22393=DIRECTION('center_axis',(0.,0.,1.));
#22394=DIRECTION('ref_axis',(1.,0.,0.));
#22395=DIRECTION('center_axis',(0.,0.,1.));
#22396=DIRECTION('ref_axis',(1.,0.,0.));
#22397=DIRECTION('center_axis',(0.,0.,1.));
#22398=DIRECTION('ref_axis',(1.,0.,0.));
#22399=DIRECTION('axis',(0.,0.,1.));
#22400=DIRECTION('refdir',(1.,0.,0.));
#22401=DIRECTION('center_axis',(0.,0.,1.));
#22402=DIRECTION('ref_axis',(1.,0.,0.));
#22403=DIRECTION('center_axis',(0.,0.,1.));
#22404=DIRECTION('ref_axis',(1.,0.,0.));
#22405=DIRECTION('',(0.,0.,1.));
#22406=DIRECTION('center_axis',(0.,0.,-1.));
#22407=DIRECTION('ref_axis',(1.,0.,0.));
#22408=DIRECTION('center_axis',(0.,0.,1.));
#22409=DIRECTION('ref_axis',(1.,0.,0.));
#22410=DIRECTION('center_axis',(0.,0.,1.));
#22411=DIRECTION('ref_axis',(1.,0.,0.));
#22412=DIRECTION('center_axis',(0.,0.,1.));
#22413=DIRECTION('ref_axis',(1.,0.,0.));
#22414=DIRECTION('',(0.,0.,-1.));
#22415=DIRECTION('center_axis',(0.,0.,1.));
#22416=DIRECTION('ref_axis',(1.,0.,0.));
#22417=DIRECTION('center_axis',(0.,0.,1.));
#22418=DIRECTION('ref_axis',(1.,0.,0.));
#22419=DIRECTION('center_axis',(0.,0.,1.));
#22420=DIRECTION('ref_axis',(1.,0.,0.));
#22421=DIRECTION('axis',(0.,0.,1.));
#22422=DIRECTION('refdir',(1.,0.,0.));
#22423=DIRECTION('center_axis',(0.,0.,1.));
#22424=DIRECTION('ref_axis',(1.,0.,0.));
#22425=DIRECTION('center_axis',(0.,0.,1.));
#22426=DIRECTION('ref_axis',(1.,0.,0.));
#22427=DIRECTION('',(0.,0.,1.));
#22428=DIRECTION('center_axis',(0.,0.,-1.));
#22429=DIRECTION('ref_axis',(1.,0.,0.));
#22430=DIRECTION('center_axis',(0.,0.,1.));
#22431=DIRECTION('ref_axis',(1.,0.,0.));
#22432=DIRECTION('center_axis',(0.,0.,1.));
#22433=DIRECTION('ref_axis',(1.,0.,0.));
#22434=DIRECTION('center_axis',(0.,0.,1.));
#22435=DIRECTION('ref_axis',(1.,0.,0.));
#22436=DIRECTION('center_axis',(0.,0.,1.));
#22437=DIRECTION('ref_axis',(1.,0.,0.));
#22438=DIRECTION('',(0.,0.,1.));
#22439=DIRECTION('center_axis',(0.,0.,-1.));
#22440=DIRECTION('ref_axis',(1.,0.,0.));
#22441=DIRECTION('center_axis',(0.,0.,1.));
#22442=DIRECTION('ref_axis',(1.,0.,0.));
#22443=DIRECTION('center_axis',(0.,0.,1.));
#22444=DIRECTION('ref_axis',(1.,0.,0.));
#22445=DIRECTION('center_axis',(0.,0.,1.));
#22446=DIRECTION('ref_axis',(1.,0.,0.));
#22447=DIRECTION('center_axis',(0.,0.,1.));
#22448=DIRECTION('ref_axis',(1.,0.,0.));
#22449=DIRECTION('',(0.,0.,1.));
#22450=DIRECTION('center_axis',(0.,0.,-1.));
#22451=DIRECTION('ref_axis',(1.,0.,0.));
#22452=DIRECTION('center_axis',(0.,0.,1.));
#22453=DIRECTION('ref_axis',(1.,0.,0.));
#22454=DIRECTION('center_axis',(0.,0.,1.));
#22455=DIRECTION('ref_axis',(1.,0.,0.));
#22456=DIRECTION('center_axis',(0.,0.,1.));
#22457=DIRECTION('ref_axis',(1.,0.,0.));
#22458=DIRECTION('center_axis',(0.,0.,1.));
#22459=DIRECTION('ref_axis',(1.,0.,0.));
#22460=DIRECTION('',(0.,0.,1.));
#22461=DIRECTION('center_axis',(0.,0.,-1.));
#22462=DIRECTION('ref_axis',(1.,0.,0.));
#22463=DIRECTION('center_axis',(0.,0.,1.));
#22464=DIRECTION('ref_axis',(1.,0.,0.));
#22465=DIRECTION('center_axis',(0.,0.,1.));
#22466=DIRECTION('ref_axis',(1.,0.,0.));
#22467=DIRECTION('center_axis',(0.,0.,1.));
#22468=DIRECTION('ref_axis',(1.,0.,0.));
#22469=DIRECTION('center_axis',(0.,0.,1.));
#22470=DIRECTION('ref_axis',(1.,0.,0.));
#22471=DIRECTION('',(0.,0.,1.));
#22472=DIRECTION('center_axis',(0.,0.,1.));
#22473=DIRECTION('ref_axis',(1.,0.,0.));
#22474=DIRECTION('center_axis',(0.,0.,1.));
#22475=DIRECTION('ref_axis',(1.,0.,0.));
#22476=DIRECTION('',(0.,0.,1.));
#22477=DIRECTION('center_axis',(0.,0.,1.));
#22478=DIRECTION('ref_axis',(1.,0.,0.));
#22479=DIRECTION('center_axis',(0.,0.,1.));
#22480=DIRECTION('ref_axis',(1.,0.,0.));
#22481=DIRECTION('',(0.,0.,1.));
#22482=DIRECTION('center_axis',(0.,0.,1.));
#22483=DIRECTION('ref_axis',(1.,0.,0.));
#22484=DIRECTION('center_axis',(0.,0.,1.));
#22485=DIRECTION('ref_axis',(1.,0.,0.));
#22486=DIRECTION('',(0.,0.,1.));
#22487=DIRECTION('center_axis',(0.,0.,1.));
#22488=DIRECTION('ref_axis',(1.,0.,0.));
#22489=DIRECTION('center_axis',(0.,0.,1.));
#22490=DIRECTION('ref_axis',(1.,0.,0.));
#22491=DIRECTION('',(0.,0.,-1.));
#22492=DIRECTION('center_axis',(0.,0.,1.));
#22493=DIRECTION('ref_axis',(1.,0.,0.));
#22494=DIRECTION('center_axis',(0.,0.,1.));
#22495=DIRECTION('ref_axis',(1.,0.,0.));
#22496=DIRECTION('center_axis',(0.,0.,1.));
#22497=DIRECTION('ref_axis',(1.,0.,0.));
#22498=DIRECTION('axis',(0.,0.,1.));
#22499=DIRECTION('refdir',(1.,0.,0.));
#22500=DIRECTION('center_axis',(0.,0.,-1.));
#22501=DIRECTION('ref_axis',(0.,1.,0.));
#22502=DIRECTION('',(0.,1.,0.));
#22503=DIRECTION('',(1.,0.,0.));
#22504=DIRECTION('',(0.,1.,0.));
#22505=DIRECTION('',(1.,0.,0.));
#22506=DIRECTION('center_axis',(0.,1.,0.));
#22507=DIRECTION('ref_axis',(0.,0.,1.));
#22508=DIRECTION('',(0.,0.,1.));
#22509=DIRECTION('',(0.,0.,1.));
#22510=DIRECTION('',(1.,0.,0.));
#22511=DIRECTION('center_axis',(0.,0.,1.));
#22512=DIRECTION('ref_axis',(0.,-1.,0.));
#22513=DIRECTION('',(0.,-1.,0.));
#22514=DIRECTION('',(0.,-1.,0.));
#22515=DIRECTION('',(1.,0.,0.));
#22516=DIRECTION('center_axis',(0.,-1.,0.));
#22517=DIRECTION('ref_axis',(0.,0.,-1.));
#22518=DIRECTION('',(0.,0.,-1.));
#22519=DIRECTION('',(0.,0.,-1.));
#22520=DIRECTION('center_axis',(1.,0.,0.));
#22521=DIRECTION('ref_axis',(0.,0.,-1.));
#22522=DIRECTION('center_axis',(0.,0.,-1.));
#22523=DIRECTION('ref_axis',(0.,1.,0.));
#22524=DIRECTION('',(0.,1.,0.));
#22525=DIRECTION('',(1.,0.,0.));
#22526=DIRECTION('',(0.,1.,0.));
#22527=DIRECTION('',(1.,0.,0.));
#22528=DIRECTION('center_axis',(0.,1.,0.));
#22529=DIRECTION('ref_axis',(0.,0.,1.));
#22530=DIRECTION('',(0.,0.,1.));
#22531=DIRECTION('',(0.,0.,1.));
#22532=DIRECTION('',(1.,0.,0.));
#22533=DIRECTION('center_axis',(0.,0.,1.));
#22534=DIRECTION('ref_axis',(0.,-1.,0.));
#22535=DIRECTION('',(0.,-1.,0.));
#22536=DIRECTION('',(0.,-1.,0.));
#22537=DIRECTION('',(1.,0.,0.));
#22538=DIRECTION('center_axis',(0.,-1.,0.));
#22539=DIRECTION('ref_axis',(0.,0.,-1.));
#22540=DIRECTION('',(0.,0.,-1.));
#22541=DIRECTION('',(0.,0.,-1.));
#22542=DIRECTION('center_axis',(1.,0.,0.));
#22543=DIRECTION('ref_axis',(0.,0.,-1.));
#22544=DIRECTION('center_axis',(0.,0.,-1.));
#22545=DIRECTION('ref_axis',(0.,1.,0.));
#22546=DIRECTION('',(0.,1.,0.));
#22547=DIRECTION('',(1.,0.,0.));
#22548=DIRECTION('',(0.,1.,0.));
#22549=DIRECTION('',(1.,0.,0.));
#22550=DIRECTION('center_axis',(0.,1.,0.));
#22551=DIRECTION('ref_axis',(0.,0.,1.));
#22552=DIRECTION('',(0.,0.,1.));
#22553=DIRECTION('',(0.,0.,1.));
#22554=DIRECTION('',(1.,0.,0.));
#22555=DIRECTION('center_axis',(0.,0.,1.));
#22556=DIRECTION('ref_axis',(0.,-1.,0.));
#22557=DIRECTION('',(0.,-1.,0.));
#22558=DIRECTION('',(0.,-1.,0.));
#22559=DIRECTION('',(1.,0.,0.));
#22560=DIRECTION('center_axis',(0.,-1.,0.));
#22561=DIRECTION('ref_axis',(0.,0.,-1.));
#22562=DIRECTION('',(0.,0.,-1.));
#22563=DIRECTION('',(0.,0.,-1.));
#22564=DIRECTION('center_axis',(1.,0.,0.));
#22565=DIRECTION('ref_axis',(0.,0.,-1.));
#22566=DIRECTION('center_axis',(0.,0.,-1.));
#22567=DIRECTION('ref_axis',(0.,1.,0.));
#22568=DIRECTION('',(0.,1.,0.));
#22569=DIRECTION('',(1.,0.,0.));
#22570=DIRECTION('',(0.,1.,0.));
#22571=DIRECTION('',(1.,0.,0.));
#22572=DIRECTION('center_axis',(0.,1.,0.));
#22573=DIRECTION('ref_axis',(0.,0.,1.));
#22574=DIRECTION('',(0.,0.,1.));
#22575=DIRECTION('',(0.,0.,1.));
#22576=DIRECTION('',(1.,0.,0.));
#22577=DIRECTION('center_axis',(0.,0.,1.));
#22578=DIRECTION('ref_axis',(0.,-1.,0.));
#22579=DIRECTION('',(0.,-1.,0.));
#22580=DIRECTION('',(0.,-1.,0.));
#22581=DIRECTION('',(1.,0.,0.));
#22582=DIRECTION('center_axis',(0.,-1.,0.));
#22583=DIRECTION('ref_axis',(0.,0.,-1.));
#22584=DIRECTION('',(0.,0.,-1.));
#22585=DIRECTION('',(0.,0.,-1.));
#22586=DIRECTION('center_axis',(1.,0.,0.));
#22587=DIRECTION('ref_axis',(0.,0.,-1.));
#22588=DIRECTION('center_axis',(0.,0.,-1.));
#22589=DIRECTION('ref_axis',(0.,1.,0.));
#22590=DIRECTION('',(0.,1.,0.));
#22591=DIRECTION('',(1.,0.,0.));
#22592=DIRECTION('',(0.,1.,0.));
#22593=DIRECTION('',(1.,0.,0.));
#22594=DIRECTION('center_axis',(0.,1.,0.));
#22595=DIRECTION('ref_axis',(0.,0.,1.));
#22596=DIRECTION('',(0.,0.,1.));
#22597=DIRECTION('',(0.,0.,1.));
#22598=DIRECTION('',(1.,0.,0.));
#22599=DIRECTION('center_axis',(0.,0.,1.));
#22600=DIRECTION('ref_axis',(0.,-1.,0.));
#22601=DIRECTION('',(0.,-1.,0.));
#22602=DIRECTION('',(0.,-1.,0.));
#22603=DIRECTION('',(1.,0.,0.));
#22604=DIRECTION('center_axis',(0.,-1.,0.));
#22605=DIRECTION('ref_axis',(0.,0.,-1.));
#22606=DIRECTION('',(0.,0.,-1.));
#22607=DIRECTION('',(0.,0.,-1.));
#22608=DIRECTION('center_axis',(1.,0.,0.));
#22609=DIRECTION('ref_axis',(0.,0.,-1.));
#22610=DIRECTION('center_axis',(0.,0.,-1.));
#22611=DIRECTION('ref_axis',(0.,1.,0.));
#22612=DIRECTION('',(0.,1.,0.));
#22613=DIRECTION('',(1.,0.,0.));
#22614=DIRECTION('',(0.,1.,0.));
#22615=DIRECTION('',(1.,0.,0.));
#22616=DIRECTION('center_axis',(0.,1.,0.));
#22617=DIRECTION('ref_axis',(0.,0.,1.));
#22618=DIRECTION('',(0.,0.,1.));
#22619=DIRECTION('',(0.,0.,1.));
#22620=DIRECTION('',(1.,0.,0.));
#22621=DIRECTION('center_axis',(0.,0.,1.));
#22622=DIRECTION('ref_axis',(0.,-1.,0.));
#22623=DIRECTION('',(0.,-1.,0.));
#22624=DIRECTION('',(0.,-1.,0.));
#22625=DIRECTION('',(1.,0.,0.));
#22626=DIRECTION('center_axis',(0.,-1.,0.));
#22627=DIRECTION('ref_axis',(0.,0.,-1.));
#22628=DIRECTION('',(0.,0.,-1.));
#22629=DIRECTION('',(0.,0.,-1.));
#22630=DIRECTION('center_axis',(1.,0.,0.));
#22631=DIRECTION('ref_axis',(0.,0.,-1.));
#22632=DIRECTION('center_axis',(0.,0.,-1.));
#22633=DIRECTION('ref_axis',(0.,1.,0.));
#22634=DIRECTION('',(0.,1.,0.));
#22635=DIRECTION('',(1.,0.,0.));
#22636=DIRECTION('',(0.,1.,0.));
#22637=DIRECTION('',(1.,0.,0.));
#22638=DIRECTION('center_axis',(0.,1.,0.));
#22639=DIRECTION('ref_axis',(0.,0.,1.));
#22640=DIRECTION('',(0.,0.,1.));
#22641=DIRECTION('',(0.,0.,1.));
#22642=DIRECTION('',(1.,0.,0.));
#22643=DIRECTION('center_axis',(0.,0.,1.));
#22644=DIRECTION('ref_axis',(0.,-1.,0.));
#22645=DIRECTION('',(0.,-1.,0.));
#22646=DIRECTION('',(0.,-1.,0.));
#22647=DIRECTION('',(1.,0.,0.));
#22648=DIRECTION('center_axis',(0.,-1.,0.));
#22649=DIRECTION('ref_axis',(0.,0.,-1.));
#22650=DIRECTION('',(0.,0.,-1.));
#22651=DIRECTION('',(0.,0.,-1.));
#22652=DIRECTION('center_axis',(1.,0.,0.));
#22653=DIRECTION('ref_axis',(0.,0.,-1.));
#22654=DIRECTION('center_axis',(0.,0.,-1.));
#22655=DIRECTION('ref_axis',(0.,1.,0.));
#22656=DIRECTION('',(0.,1.,0.));
#22657=DIRECTION('',(1.,0.,0.));
#22658=DIRECTION('',(0.,1.,0.));
#22659=DIRECTION('',(1.,0.,0.));
#22660=DIRECTION('center_axis',(0.,1.,0.));
#22661=DIRECTION('ref_axis',(0.,0.,1.));
#22662=DIRECTION('',(0.,0.,1.));
#22663=DIRECTION('',(0.,0.,1.));
#22664=DIRECTION('',(1.,0.,0.));
#22665=DIRECTION('center_axis',(0.,0.,1.));
#22666=DIRECTION('ref_axis',(0.,-1.,0.));
#22667=DIRECTION('',(0.,-1.,0.));
#22668=DIRECTION('',(0.,-1.,0.));
#22669=DIRECTION('',(1.,0.,0.));
#22670=DIRECTION('center_axis',(0.,-1.,0.));
#22671=DIRECTION('ref_axis',(0.,0.,-1.));
#22672=DIRECTION('',(0.,0.,-1.));
#22673=DIRECTION('',(0.,0.,-1.));
#22674=DIRECTION('center_axis',(1.,0.,0.));
#22675=DIRECTION('ref_axis',(0.,0.,-1.));
#22676=DIRECTION('center_axis',(0.,0.,-1.));
#22677=DIRECTION('ref_axis',(0.,1.,0.));
#22678=DIRECTION('',(0.,1.,0.));
#22679=DIRECTION('',(1.,0.,0.));
#22680=DIRECTION('',(0.,1.,0.));
#22681=DIRECTION('',(1.,0.,0.));
#22682=DIRECTION('center_axis',(0.,1.,0.));
#22683=DIRECTION('ref_axis',(0.,0.,1.));
#22684=DIRECTION('',(0.,0.,1.));
#22685=DIRECTION('',(0.,0.,1.));
#22686=DIRECTION('',(1.,0.,0.));
#22687=DIRECTION('center_axis',(0.,0.,1.));
#22688=DIRECTION('ref_axis',(0.,-1.,0.));
#22689=DIRECTION('',(0.,-1.,0.));
#22690=DIRECTION('',(0.,-1.,0.));
#22691=DIRECTION('',(1.,0.,0.));
#22692=DIRECTION('center_axis',(0.,-1.,0.));
#22693=DIRECTION('ref_axis',(0.,0.,-1.));
#22694=DIRECTION('',(0.,0.,-1.));
#22695=DIRECTION('',(0.,0.,-1.));
#22696=DIRECTION('center_axis',(1.,0.,0.));
#22697=DIRECTION('ref_axis',(0.,0.,-1.));
#22698=DIRECTION('center_axis',(0.,0.,-1.));
#22699=DIRECTION('ref_axis',(0.,1.,0.));
#22700=DIRECTION('',(0.,1.,0.));
#22701=DIRECTION('',(1.,0.,0.));
#22702=DIRECTION('',(0.,1.,0.));
#22703=DIRECTION('',(1.,0.,0.));
#22704=DIRECTION('center_axis',(0.,1.,0.));
#22705=DIRECTION('ref_axis',(0.,0.,1.));
#22706=DIRECTION('',(0.,0.,1.));
#22707=DIRECTION('',(0.,0.,1.));
#22708=DIRECTION('',(1.,0.,0.));
#22709=DIRECTION('center_axis',(0.,0.,1.));
#22710=DIRECTION('ref_axis',(0.,-1.,0.));
#22711=DIRECTION('',(0.,-1.,0.));
#22712=DIRECTION('',(0.,-1.,0.));
#22713=DIRECTION('',(1.,0.,0.));
#22714=DIRECTION('center_axis',(0.,-1.,0.));
#22715=DIRECTION('ref_axis',(0.,0.,-1.));
#22716=DIRECTION('',(0.,0.,-1.));
#22717=DIRECTION('',(0.,0.,-1.));
#22718=DIRECTION('center_axis',(1.,0.,0.));
#22719=DIRECTION('ref_axis',(0.,0.,-1.));
#22720=DIRECTION('center_axis',(0.,0.,-1.));
#22721=DIRECTION('ref_axis',(0.,1.,0.));
#22722=DIRECTION('',(0.,1.,0.));
#22723=DIRECTION('',(1.,0.,0.));
#22724=DIRECTION('',(0.,1.,0.));
#22725=DIRECTION('',(1.,0.,0.));
#22726=DIRECTION('center_axis',(0.,1.,0.));
#22727=DIRECTION('ref_axis',(0.,0.,1.));
#22728=DIRECTION('',(0.,0.,1.));
#22729=DIRECTION('',(0.,0.,1.));
#22730=DIRECTION('',(1.,0.,0.));
#22731=DIRECTION('center_axis',(0.,0.,1.));
#22732=DIRECTION('ref_axis',(0.,-1.,0.));
#22733=DIRECTION('',(0.,-1.,0.));
#22734=DIRECTION('',(0.,-1.,0.));
#22735=DIRECTION('',(1.,0.,0.));
#22736=DIRECTION('center_axis',(0.,-1.,0.));
#22737=DIRECTION('ref_axis',(0.,0.,-1.));
#22738=DIRECTION('',(0.,0.,-1.));
#22739=DIRECTION('',(0.,0.,-1.));
#22740=DIRECTION('center_axis',(1.,0.,0.));
#22741=DIRECTION('ref_axis',(0.,0.,-1.));
#22742=DIRECTION('center_axis',(0.,0.,-1.));
#22743=DIRECTION('ref_axis',(0.,1.,0.));
#22744=DIRECTION('',(0.,1.,0.));
#22745=DIRECTION('',(1.,0.,0.));
#22746=DIRECTION('',(0.,1.,0.));
#22747=DIRECTION('',(1.,0.,0.));
#22748=DIRECTION('center_axis',(0.,1.,0.));
#22749=DIRECTION('ref_axis',(0.,0.,1.));
#22750=DIRECTION('',(0.,0.,1.));
#22751=DIRECTION('',(0.,0.,1.));
#22752=DIRECTION('',(1.,0.,0.));
#22753=DIRECTION('center_axis',(0.,0.,1.));
#22754=DIRECTION('ref_axis',(0.,-1.,0.));
#22755=DIRECTION('',(0.,-1.,0.));
#22756=DIRECTION('',(0.,-1.,0.));
#22757=DIRECTION('',(1.,0.,0.));
#22758=DIRECTION('center_axis',(0.,-1.,0.));
#22759=DIRECTION('ref_axis',(0.,0.,-1.));
#22760=DIRECTION('',(0.,0.,-1.));
#22761=DIRECTION('',(0.,0.,-1.));
#22762=DIRECTION('center_axis',(1.,0.,0.));
#22763=DIRECTION('ref_axis',(0.,0.,-1.));
#22764=DIRECTION('center_axis',(0.,0.,-1.));
#22765=DIRECTION('ref_axis',(0.,1.,0.));
#22766=DIRECTION('',(0.,1.,0.));
#22767=DIRECTION('',(1.,0.,0.));
#22768=DIRECTION('',(0.,1.,0.));
#22769=DIRECTION('',(1.,0.,0.));
#22770=DIRECTION('center_axis',(0.,1.,0.));
#22771=DIRECTION('ref_axis',(0.,0.,1.));
#22772=DIRECTION('',(0.,0.,1.));
#22773=DIRECTION('',(0.,0.,1.));
#22774=DIRECTION('',(1.,0.,0.));
#22775=DIRECTION('center_axis',(0.,0.,1.));
#22776=DIRECTION('ref_axis',(0.,-1.,0.));
#22777=DIRECTION('',(0.,-1.,0.));
#22778=DIRECTION('',(0.,-1.,0.));
#22779=DIRECTION('',(1.,0.,0.));
#22780=DIRECTION('center_axis',(0.,-1.,0.));
#22781=DIRECTION('ref_axis',(0.,0.,-1.));
#22782=DIRECTION('',(0.,0.,-1.));
#22783=DIRECTION('',(0.,0.,-1.));
#22784=DIRECTION('center_axis',(1.,0.,0.));
#22785=DIRECTION('ref_axis',(0.,0.,-1.));
#22786=DIRECTION('center_axis',(0.,0.,-1.));
#22787=DIRECTION('ref_axis',(0.,1.,0.));
#22788=DIRECTION('',(0.,1.,0.));
#22789=DIRECTION('',(1.,0.,0.));
#22790=DIRECTION('',(0.,1.,0.));
#22791=DIRECTION('',(1.,0.,0.));
#22792=DIRECTION('center_axis',(0.,1.,0.));
#22793=DIRECTION('ref_axis',(0.,0.,1.));
#22794=DIRECTION('',(0.,0.,1.));
#22795=DIRECTION('',(0.,0.,1.));
#22796=DIRECTION('',(1.,0.,0.));
#22797=DIRECTION('center_axis',(0.,0.,1.));
#22798=DIRECTION('ref_axis',(0.,-1.,0.));
#22799=DIRECTION('',(0.,-1.,0.));
#22800=DIRECTION('',(0.,-1.,0.));
#22801=DIRECTION('',(1.,0.,0.));
#22802=DIRECTION('center_axis',(0.,-1.,0.));
#22803=DIRECTION('ref_axis',(0.,0.,-1.));
#22804=DIRECTION('',(0.,0.,-1.));
#22805=DIRECTION('',(0.,0.,-1.));
#22806=DIRECTION('center_axis',(1.,0.,0.));
#22807=DIRECTION('ref_axis',(0.,0.,-1.));
#22808=DIRECTION('center_axis',(0.,0.,-1.));
#22809=DIRECTION('ref_axis',(0.,1.,0.));
#22810=DIRECTION('',(0.,1.,0.));
#22811=DIRECTION('',(1.,0.,0.));
#22812=DIRECTION('',(0.,1.,0.));
#22813=DIRECTION('',(1.,0.,0.));
#22814=DIRECTION('center_axis',(0.,1.,0.));
#22815=DIRECTION('ref_axis',(0.,0.,1.));
#22816=DIRECTION('',(0.,0.,1.));
#22817=DIRECTION('',(0.,0.,1.));
#22818=DIRECTION('',(1.,0.,0.));
#22819=DIRECTION('center_axis',(0.,0.,1.));
#22820=DIRECTION('ref_axis',(0.,-1.,0.));
#22821=DIRECTION('',(0.,-1.,0.));
#22822=DIRECTION('',(0.,-1.,0.));
#22823=DIRECTION('',(1.,0.,0.));
#22824=DIRECTION('center_axis',(0.,-1.,0.));
#22825=DIRECTION('ref_axis',(0.,0.,-1.));
#22826=DIRECTION('',(0.,0.,-1.));
#22827=DIRECTION('',(0.,0.,-1.));
#22828=DIRECTION('center_axis',(1.,0.,0.));
#22829=DIRECTION('ref_axis',(0.,0.,-1.));
#22830=DIRECTION('center_axis',(0.,0.,-1.));
#22831=DIRECTION('ref_axis',(0.,1.,0.));
#22832=DIRECTION('',(0.,1.,0.));
#22833=DIRECTION('',(1.,0.,0.));
#22834=DIRECTION('',(0.,1.,0.));
#22835=DIRECTION('',(1.,0.,0.));
#22836=DIRECTION('center_axis',(0.,1.,0.));
#22837=DIRECTION('ref_axis',(0.,0.,1.));
#22838=DIRECTION('',(0.,0.,1.));
#22839=DIRECTION('',(0.,0.,1.));
#22840=DIRECTION('',(1.,0.,0.));
#22841=DIRECTION('center_axis',(0.,0.,1.));
#22842=DIRECTION('ref_axis',(0.,-1.,0.));
#22843=DIRECTION('',(0.,-1.,0.));
#22844=DIRECTION('',(0.,-1.,0.));
#22845=DIRECTION('',(1.,0.,0.));
#22846=DIRECTION('center_axis',(0.,-1.,0.));
#22847=DIRECTION('ref_axis',(0.,0.,-1.));
#22848=DIRECTION('',(0.,0.,-1.));
#22849=DIRECTION('',(0.,0.,-1.));
#22850=DIRECTION('center_axis',(1.,0.,0.));
#22851=DIRECTION('ref_axis',(0.,0.,-1.));
#22852=DIRECTION('center_axis',(0.,0.,-1.));
#22853=DIRECTION('ref_axis',(0.,1.,0.));
#22854=DIRECTION('',(0.,1.,0.));
#22855=DIRECTION('',(1.,0.,0.));
#22856=DIRECTION('',(0.,1.,0.));
#22857=DIRECTION('',(1.,0.,0.));
#22858=DIRECTION('center_axis',(0.,1.,0.));
#22859=DIRECTION('ref_axis',(0.,0.,1.));
#22860=DIRECTION('',(0.,0.,1.));
#22861=DIRECTION('',(0.,0.,1.));
#22862=DIRECTION('',(1.,0.,0.));
#22863=DIRECTION('center_axis',(0.,0.,1.));
#22864=DIRECTION('ref_axis',(0.,-1.,0.));
#22865=DIRECTION('',(0.,-1.,0.));
#22866=DIRECTION('',(0.,-1.,0.));
#22867=DIRECTION('',(1.,0.,0.));
#22868=DIRECTION('center_axis',(0.,-1.,0.));
#22869=DIRECTION('ref_axis',(0.,0.,-1.));
#22870=DIRECTION('',(0.,0.,-1.));
#22871=DIRECTION('',(0.,0.,-1.));
#22872=DIRECTION('center_axis',(1.,0.,0.));
#22873=DIRECTION('ref_axis',(0.,0.,-1.));
#22874=DIRECTION('center_axis',(0.,0.,-1.));
#22875=DIRECTION('ref_axis',(0.,1.,0.));
#22876=DIRECTION('',(0.,1.,0.));
#22877=DIRECTION('',(1.,0.,0.));
#22878=DIRECTION('',(0.,1.,0.));
#22879=DIRECTION('',(1.,0.,0.));
#22880=DIRECTION('center_axis',(0.,1.,0.));
#22881=DIRECTION('ref_axis',(0.,0.,1.));
#22882=DIRECTION('',(0.,0.,1.));
#22883=DIRECTION('',(0.,0.,1.));
#22884=DIRECTION('',(1.,0.,0.));
#22885=DIRECTION('center_axis',(0.,0.,1.));
#22886=DIRECTION('ref_axis',(0.,-1.,0.));
#22887=DIRECTION('',(0.,-1.,0.));
#22888=DIRECTION('',(0.,-1.,0.));
#22889=DIRECTION('',(1.,0.,0.));
#22890=DIRECTION('center_axis',(0.,-1.,0.));
#22891=DIRECTION('ref_axis',(0.,0.,-1.));
#22892=DIRECTION('',(0.,0.,-1.));
#22893=DIRECTION('',(0.,0.,-1.));
#22894=DIRECTION('center_axis',(1.,0.,0.));
#22895=DIRECTION('ref_axis',(0.,0.,-1.));
#22896=DIRECTION('center_axis',(0.,0.,-1.));
#22897=DIRECTION('ref_axis',(0.,1.,0.));
#22898=DIRECTION('',(0.,1.,0.));
#22899=DIRECTION('',(1.,0.,0.));
#22900=DIRECTION('',(0.,1.,0.));
#22901=DIRECTION('',(1.,0.,0.));
#22902=DIRECTION('center_axis',(0.,1.,0.));
#22903=DIRECTION('ref_axis',(0.,0.,1.));
#22904=DIRECTION('',(0.,0.,1.));
#22905=DIRECTION('',(0.,0.,1.));
#22906=DIRECTION('',(1.,0.,0.));
#22907=DIRECTION('center_axis',(0.,0.,1.));
#22908=DIRECTION('ref_axis',(0.,-1.,0.));
#22909=DIRECTION('',(0.,-1.,0.));
#22910=DIRECTION('',(0.,-1.,0.));
#22911=DIRECTION('',(1.,0.,0.));
#22912=DIRECTION('center_axis',(0.,-1.,0.));
#22913=DIRECTION('ref_axis',(0.,0.,-1.));
#22914=DIRECTION('',(0.,0.,-1.));
#22915=DIRECTION('',(0.,0.,-1.));
#22916=DIRECTION('center_axis',(1.,0.,0.));
#22917=DIRECTION('ref_axis',(0.,0.,-1.));
#22918=DIRECTION('center_axis',(0.,0.,-1.));
#22919=DIRECTION('ref_axis',(0.,1.,0.));
#22920=DIRECTION('',(0.,1.,0.));
#22921=DIRECTION('',(1.,0.,0.));
#22922=DIRECTION('',(0.,1.,0.));
#22923=DIRECTION('',(1.,0.,0.));
#22924=DIRECTION('center_axis',(0.,1.,0.));
#22925=DIRECTION('ref_axis',(0.,0.,1.));
#22926=DIRECTION('',(0.,0.,1.));
#22927=DIRECTION('',(0.,0.,1.));
#22928=DIRECTION('',(1.,0.,0.));
#22929=DIRECTION('center_axis',(0.,0.,1.));
#22930=DIRECTION('ref_axis',(0.,-1.,0.));
#22931=DIRECTION('',(0.,-1.,0.));
#22932=DIRECTION('',(0.,-1.,0.));
#22933=DIRECTION('',(1.,0.,0.));
#22934=DIRECTION('center_axis',(0.,-1.,0.));
#22935=DIRECTION('ref_axis',(0.,0.,-1.));
#22936=DIRECTION('',(0.,0.,-1.));
#22937=DIRECTION('',(0.,0.,-1.));
#22938=DIRECTION('center_axis',(1.,0.,0.));
#22939=DIRECTION('ref_axis',(0.,0.,-1.));
#22940=DIRECTION('center_axis',(0.,0.,-1.));
#22941=DIRECTION('ref_axis',(0.,1.,0.));
#22942=DIRECTION('',(0.,1.,0.));
#22943=DIRECTION('',(1.,0.,0.));
#22944=DIRECTION('',(0.,1.,0.));
#22945=DIRECTION('',(1.,0.,0.));
#22946=DIRECTION('center_axis',(0.,1.,0.));
#22947=DIRECTION('ref_axis',(0.,0.,1.));
#22948=DIRECTION('',(0.,0.,1.));
#22949=DIRECTION('',(0.,0.,1.));
#22950=DIRECTION('',(1.,0.,0.));
#22951=DIRECTION('center_axis',(0.,0.,1.));
#22952=DIRECTION('ref_axis',(0.,-1.,0.));
#22953=DIRECTION('',(0.,-1.,0.));
#22954=DIRECTION('',(0.,-1.,0.));
#22955=DIRECTION('',(1.,0.,0.));
#22956=DIRECTION('center_axis',(0.,-1.,0.));
#22957=DIRECTION('ref_axis',(0.,0.,-1.));
#22958=DIRECTION('',(0.,0.,-1.));
#22959=DIRECTION('',(0.,0.,-1.));
#22960=DIRECTION('center_axis',(1.,0.,0.));
#22961=DIRECTION('ref_axis',(0.,0.,-1.));
#22962=DIRECTION('center_axis',(0.,0.,-1.));
#22963=DIRECTION('ref_axis',(0.,1.,0.));
#22964=DIRECTION('',(0.,1.,0.));
#22965=DIRECTION('',(1.,0.,0.));
#22966=DIRECTION('',(0.,1.,0.));
#22967=DIRECTION('',(1.,0.,0.));
#22968=DIRECTION('center_axis',(0.,1.,0.));
#22969=DIRECTION('ref_axis',(0.,0.,1.));
#22970=DIRECTION('',(0.,0.,1.));
#22971=DIRECTION('',(0.,0.,1.));
#22972=DIRECTION('',(1.,0.,0.));
#22973=DIRECTION('center_axis',(0.,0.,1.));
#22974=DIRECTION('ref_axis',(0.,-1.,0.));
#22975=DIRECTION('',(0.,-1.,0.));
#22976=DIRECTION('',(0.,-1.,0.));
#22977=DIRECTION('',(1.,0.,0.));
#22978=DIRECTION('center_axis',(0.,-1.,0.));
#22979=DIRECTION('ref_axis',(0.,0.,-1.));
#22980=DIRECTION('',(0.,0.,-1.));
#22981=DIRECTION('',(0.,0.,-1.));
#22982=DIRECTION('center_axis',(1.,0.,0.));
#22983=DIRECTION('ref_axis',(0.,0.,-1.));
#22984=DIRECTION('center_axis',(0.,0.,-1.));
#22985=DIRECTION('ref_axis',(0.,1.,0.));
#22986=DIRECTION('',(0.,1.,0.));
#22987=DIRECTION('',(1.,0.,0.));
#22988=DIRECTION('',(0.,1.,0.));
#22989=DIRECTION('',(1.,0.,0.));
#22990=DIRECTION('center_axis',(0.,1.,0.));
#22991=DIRECTION('ref_axis',(0.,0.,1.));
#22992=DIRECTION('',(0.,0.,1.));
#22993=DIRECTION('',(0.,0.,1.));
#22994=DIRECTION('',(1.,0.,0.));
#22995=DIRECTION('center_axis',(0.,0.,1.));
#22996=DIRECTION('ref_axis',(0.,-1.,0.));
#22997=DIRECTION('',(0.,-1.,0.));
#22998=DIRECTION('',(0.,-1.,0.));
#22999=DIRECTION('',(1.,0.,0.));
#23000=DIRECTION('center_axis',(0.,-1.,0.));
#23001=DIRECTION('ref_axis',(0.,0.,-1.));
#23002=DIRECTION('',(0.,0.,-1.));
#23003=DIRECTION('',(0.,0.,-1.));
#23004=DIRECTION('center_axis',(1.,0.,0.));
#23005=DIRECTION('ref_axis',(0.,0.,-1.));
#23006=DIRECTION('center_axis',(0.,0.,-1.));
#23007=DIRECTION('ref_axis',(0.,1.,0.));
#23008=DIRECTION('',(0.,1.,0.));
#23009=DIRECTION('',(1.,0.,0.));
#23010=DIRECTION('',(0.,1.,0.));
#23011=DIRECTION('',(1.,0.,0.));
#23012=DIRECTION('center_axis',(0.,1.,0.));
#23013=DIRECTION('ref_axis',(0.,0.,1.));
#23014=DIRECTION('',(0.,0.,1.));
#23015=DIRECTION('',(0.,0.,1.));
#23016=DIRECTION('',(1.,0.,0.));
#23017=DIRECTION('center_axis',(0.,0.,1.));
#23018=DIRECTION('ref_axis',(0.,-1.,0.));
#23019=DIRECTION('',(0.,-1.,0.));
#23020=DIRECTION('',(0.,-1.,0.));
#23021=DIRECTION('',(1.,0.,0.));
#23022=DIRECTION('center_axis',(0.,-1.,0.));
#23023=DIRECTION('ref_axis',(0.,0.,-1.));
#23024=DIRECTION('',(0.,0.,-1.));
#23025=DIRECTION('',(0.,0.,-1.));
#23026=DIRECTION('center_axis',(1.,0.,0.));
#23027=DIRECTION('ref_axis',(0.,0.,-1.));
#23028=DIRECTION('center_axis',(0.,0.,-1.));
#23029=DIRECTION('ref_axis',(0.,1.,0.));
#23030=DIRECTION('',(0.,1.,0.));
#23031=DIRECTION('',(1.,0.,0.));
#23032=DIRECTION('',(0.,1.,0.));
#23033=DIRECTION('',(1.,0.,0.));
#23034=DIRECTION('center_axis',(0.,1.,0.));
#23035=DIRECTION('ref_axis',(0.,0.,1.));
#23036=DIRECTION('',(0.,0.,1.));
#23037=DIRECTION('',(0.,0.,1.));
#23038=DIRECTION('',(1.,0.,0.));
#23039=DIRECTION('center_axis',(0.,0.,1.));
#23040=DIRECTION('ref_axis',(0.,-1.,0.));
#23041=DIRECTION('',(0.,-1.,0.));
#23042=DIRECTION('',(0.,-1.,0.));
#23043=DIRECTION('',(1.,0.,0.));
#23044=DIRECTION('center_axis',(0.,-1.,0.));
#23045=DIRECTION('ref_axis',(0.,0.,-1.));
#23046=DIRECTION('',(0.,0.,-1.));
#23047=DIRECTION('',(0.,0.,-1.));
#23048=DIRECTION('center_axis',(1.,0.,0.));
#23049=DIRECTION('ref_axis',(0.,0.,-1.));
#23050=DIRECTION('center_axis',(1.,0.,0.));
#23051=DIRECTION('ref_axis',(0.,0.,-1.));
#23052=DIRECTION('center_axis',(1.,0.,0.));
#23053=DIRECTION('ref_axis',(0.,0.,-1.));
#23054=DIRECTION('',(1.,0.,0.));
#23055=DIRECTION('center_axis',(-1.,0.,0.));
#23056=DIRECTION('ref_axis',(0.,0.,-1.));
#23057=DIRECTION('center_axis',(1.,0.,0.));
#23058=DIRECTION('ref_axis',(0.,0.,-1.));
#23059=DIRECTION('center_axis',(1.,0.,0.));
#23060=DIRECTION('ref_axis',(0.,0.,-1.));
#23061=DIRECTION('',(1.,0.,0.));
#23062=DIRECTION('center_axis',(-1.,0.,0.));
#23063=DIRECTION('ref_axis',(0.,0.,-1.));
#23064=DIRECTION('center_axis',(0.,1.,0.));
#23065=DIRECTION('ref_axis',(-1.,0.,0.));
#23066=DIRECTION('',(-1.,0.,0.));
#23067=DIRECTION('',(0.,0.,1.));
#23068=DIRECTION('',(-1.,0.,0.));
#23069=DIRECTION('',(0.,0.,1.));
#23070=DIRECTION('center_axis',(1.,0.,0.));
#23071=DIRECTION('ref_axis',(0.,1.,0.));
#23072=DIRECTION('',(0.,1.,0.));
#23073=DIRECTION('',(0.,1.,0.));
#23074=DIRECTION('',(0.,0.,1.));
#23075=DIRECTION('center_axis',(0.,-1.,0.));
#23076=DIRECTION('ref_axis',(1.,0.,0.));
#23077=DIRECTION('',(1.,0.,0.));
#23078=DIRECTION('',(1.,0.,0.));
#23079=DIRECTION('',(0.,0.,1.));
#23080=DIRECTION('center_axis',(-1.,0.,0.));
#23081=DIRECTION('ref_axis',(0.,-1.,0.));
#23082=DIRECTION('',(0.,-1.,0.));
#23083=DIRECTION('',(0.,-1.,0.));
#23084=DIRECTION('center_axis',(0.,0.,1.));
#23085=DIRECTION('ref_axis',(1.,0.,0.));
#23086=DIRECTION('center_axis',(0.,0.,1.));
#23087=DIRECTION('ref_axis',(1.,0.,0.));
#23088=DIRECTION('axis',(0.,0.,1.));
#23089=DIRECTION('refdir',(1.,0.,0.));
#23090=DIRECTION('center_axis',(1.,0.,0.));
#23091=DIRECTION('ref_axis',(0.,0.,-1.));
#23092=DIRECTION('center_axis',(-1.,0.,0.));
#23093=DIRECTION('ref_axis',(0.,0.,-1.));
#23094=DIRECTION('',(-0.707106781186548,8.65956056235493E-17,-0.707106781186547));
#23095=DIRECTION('center_axis',(1.,0.,0.));
#23096=DIRECTION('ref_axis',(0.,0.,-1.));
#23097=DIRECTION('center_axis',(1.,0.,0.));
#23098=DIRECTION('ref_axis',(0.,0.,-1.));
#23099=DIRECTION('center_axis',(1.,0.,0.));
#23100=DIRECTION('ref_axis',(0.,0.,-1.));
#23101=DIRECTION('',(-1.,0.,0.));
#23102=DIRECTION('center_axis',(1.,0.,0.));
#23103=DIRECTION('ref_axis',(0.,0.,-1.));
#23104=DIRECTION('center_axis',(-1.,0.,0.));
#23105=DIRECTION('ref_axis',(0.,0.,-1.));
#23106=DIRECTION('center_axis',(-1.,0.,0.));
#23107=DIRECTION('ref_axis',(0.,0.,-1.));
#23108=DIRECTION('',(-0.707106781186553,-8.65956056235487E-17,0.707106781186542));
#23109=DIRECTION('center_axis',(1.,0.,0.));
#23110=DIRECTION('ref_axis',(0.,0.,-1.));
#23111=DIRECTION('axis',(0.,0.,1.));
#23112=DIRECTION('refdir',(1.,0.,0.));
#23113=DIRECTION('center_axis',(0.,0.,1.));
#23114=DIRECTION('ref_axis',(1.,0.,0.));
#23115=DIRECTION('',(0.,-1.,0.));
#23116=DIRECTION('center_axis',(0.,0.,1.));
#23117=DIRECTION('ref_axis',(1.,0.,0.));
#23118=DIRECTION('center_axis',(0.,0.,1.));
#23119=DIRECTION('ref_axis',(1.,0.,0.));
#23120=DIRECTION('',(0.,0.,1.));
#23121=DIRECTION('center_axis',(0.,0.,1.));
#23122=DIRECTION('ref_axis',(1.,0.,0.));
#23123=DIRECTION('',(0.,0.,-1.));
#23124=DIRECTION('center_axis',(0.,0.,1.));
#23125=DIRECTION('ref_axis',(-1.,1.22464679914735E-16,0.));
#23126=DIRECTION('',(0.,0.,-1.));
#23127=DIRECTION('center_axis',(0.,0.,1.));
#23128=DIRECTION('ref_axis',(1.,0.,0.));
#23129=DIRECTION('',(0.,0.,1.));
#23130=DIRECTION('center_axis',(0.,0.,1.));
#23131=DIRECTION('ref_axis',(1.,0.,0.));
#23132=DIRECTION('center_axis',(0.,0.,1.));
#23133=DIRECTION('ref_axis',(1.,0.,0.));
#23134=DIRECTION('',(0.,1.,0.));
#23135=DIRECTION('center_axis',(0.,0.,1.));
#23136=DIRECTION('ref_axis',(1.,0.,0.));
#23137=DIRECTION('',(0.,1.,0.));
#23138=DIRECTION('',(1.,0.,0.));
#23139=DIRECTION('',(0.,-1.,0.));
#23140=DIRECTION('',(-1.,0.,0.));
#23141=DIRECTION('',(0.,1.,0.));
#23142=DIRECTION('center_axis',(0.,0.,-1.));
#23143=DIRECTION('ref_axis',(1.,0.,0.));
#23144=DIRECTION('center_axis',(-1.,0.,0.));
#23145=DIRECTION('ref_axis',(0.,0.,1.));
#23146=DIRECTION('',(0.,0.,-1.));
#23147=DIRECTION('',(0.,1.,0.));
#23148=DIRECTION('',(0.,0.,1.));
#23149=DIRECTION('center_axis',(1.,0.,0.));
#23150=DIRECTION('ref_axis',(0.,0.,-1.));
#23151=DIRECTION('center_axis',(0.,0.,1.));
#23152=DIRECTION('ref_axis',(1.,0.,0.));
#23153=DIRECTION('',(0.,1.,0.));
#23154=DIRECTION('',(1.,0.,0.));
#23155=DIRECTION('',(0.,1.,0.));
#23156=DIRECTION('',(0.,1.,0.));
#23157=DIRECTION('',(-1.,0.,0.));
#23158=DIRECTION('center_axis',(0.,0.,-1.));
#23159=DIRECTION('ref_axis',(1.,0.,0.));
#23160=DIRECTION('center_axis',(1.,0.,0.));
#23161=DIRECTION('ref_axis',(0.,0.,-1.));
#23162=DIRECTION('center_axis',(1.,0.,0.));
#23163=DIRECTION('ref_axis',(0.,0.,-1.));
#23164=DIRECTION('',(1.,0.,0.));
#23165=DIRECTION('center_axis',(-1.,0.,0.));
#23166=DIRECTION('ref_axis',(0.,0.,-1.));
#23167=DIRECTION('center_axis',(1.,0.,0.));
#23168=DIRECTION('ref_axis',(0.,0.,-1.));
#23169=DIRECTION('',(1.,0.,0.));
#23170=DIRECTION('center_axis',(-1.,0.,0.));
#23171=DIRECTION('ref_axis',(0.,0.,-1.));
#23172=DIRECTION('center_axis',(0.,0.,1.));
#23173=DIRECTION('ref_axis',(1.,0.,0.));
#23174=DIRECTION('center_axis',(0.,0.,1.));
#23175=DIRECTION('ref_axis',(1.,0.,0.));
#23176=DIRECTION('',(0.,0.,1.));
#23177=DIRECTION('center_axis',(0.,0.,1.));
#23178=DIRECTION('ref_axis',(1.,0.,0.));
#23179=DIRECTION('center_axis',(0.,0.,1.));
#23180=DIRECTION('ref_axis',(1.,0.,0.));
#23181=DIRECTION('',(0.,0.,1.));
#23182=DIRECTION('center_axis',(0.,1.,0.));
#23183=DIRECTION('ref_axis',(1.,0.,0.));
#23184=DIRECTION('center_axis',(0.,1.,0.));
#23185=DIRECTION('ref_axis',(1.,0.,0.));
#23186=DIRECTION('',(0.,1.,0.));
#23187=DIRECTION('center_axis',(0.,-1.,0.));
#23188=DIRECTION('ref_axis',(1.,0.,0.));
#23189=DIRECTION('center_axis',(0.,-1.,0.));
#23190=DIRECTION('ref_axis',(0.,0.,-1.));
#23191=DIRECTION('',(0.,0.,-1.));
#23192=DIRECTION('',(1.,0.,0.));
#23193=DIRECTION('',(0.,0.,1.));
#23194=DIRECTION('',(0.,0.,1.));
#23195=DIRECTION('',(-1.,0.,0.));
#23196=DIRECTION('',(0.,0.,-1.));
#23197=DIRECTION('',(-1.,0.,0.));
#23198=DIRECTION('',(0.,0.,1.));
#23199=DIRECTION('',(-1.,0.,0.));
#23200=DIRECTION('center_axis',(-1.,0.,0.));
#23201=DIRECTION('ref_axis',(0.,0.,1.));
#23202=DIRECTION('',(0.,0.,1.));
#23203=DIRECTION('',(0.,1.,0.));
#23204=DIRECTION('center_axis',(0.,0.,-1.));
#23205=DIRECTION('ref_axis',(-1.,0.,0.));
#23206=DIRECTION('',(-1.,0.,0.));
#23207=DIRECTION('',(0.,1.,0.));
#23208=DIRECTION('center_axis',(1.,0.,0.));
#23209=DIRECTION('ref_axis',(0.,0.,-1.));
#23210=DIRECTION('',(0.,0.,-1.));
#23211=DIRECTION('center_axis',(1.,0.,0.));
#23212=DIRECTION('ref_axis',(0.,0.,-1.));
#23213=DIRECTION('',(0.,0.,-1.));
#23214=DIRECTION('',(0.,1.,0.));
#23215=DIRECTION('center_axis',(0.,0.,1.));
#23216=DIRECTION('ref_axis',(1.,0.,0.));
#23217=DIRECTION('',(1.,0.,0.));
#23218=DIRECTION('',(0.,1.,0.));
#23219=DIRECTION('center_axis',(-1.,0.,0.));
#23220=DIRECTION('ref_axis',(0.,0.,1.));
#23221=DIRECTION('',(0.,0.,1.));
#23222=DIRECTION('',(0.,1.,0.));
#23223=DIRECTION('center_axis',(0.,0.,1.));
#23224=DIRECTION('ref_axis',(1.,0.,0.));
#23225=DIRECTION('',(1.,0.,0.));
#23226=DIRECTION('',(0.,1.,0.));
#23227=DIRECTION('center_axis',(1.,0.,0.));
#23228=DIRECTION('ref_axis',(0.,0.,-1.));
#23229=DIRECTION('',(0.,0.,-1.));
#23230=DIRECTION('',(0.,1.,0.));
#23231=DIRECTION('center_axis',(0.,0.,1.));
#23232=DIRECTION('ref_axis',(1.,0.,0.));
#23233=DIRECTION('',(1.,0.,0.));
#23234=DIRECTION('center_axis',(0.,1.,0.));
#23235=DIRECTION('ref_axis',(0.,0.,1.));
#23236=DIRECTION('axis',(0.,0.,1.));
#23237=DIRECTION('refdir',(1.,0.,0.));
#23238=DIRECTION('center_axis',(0.866025403784439,0.,-0.5));
#23239=DIRECTION('ref_axis',(0.5,0.,0.866025403784439));
#23240=DIRECTION('',(-0.5,0.,-0.866025403784439));
#23241=DIRECTION('',(0.,-1.,0.));
#23242=DIRECTION('',(0.5,0.,0.866025403784439));
#23243=DIRECTION('',(0.,-1.,0.));
#23244=DIRECTION('center_axis',(1.20185167898973E-16,0.,-1.));
#23245=DIRECTION('ref_axis',(1.,0.,1.20185167898973E-16));
#23246=DIRECTION('',(-1.,0.,-1.20185167898973E-16));
#23247=DIRECTION('',(0.,-1.,0.));
#23248=DIRECTION('',(1.,0.,1.20185167898973E-16));
#23249=DIRECTION('center_axis',(-0.866025403784439,0.,-0.5));
#23250=DIRECTION('ref_axis',(0.5,0.,-0.866025403784439));
#23251=DIRECTION('',(-0.5,0.,0.866025403784439));
#23252=DIRECTION('',(0.,-1.,0.));
#23253=DIRECTION('',(0.5,0.,-0.866025403784439));
#23254=DIRECTION('center_axis',(-0.866025403784439,0.,0.5));
#23255=DIRECTION('ref_axis',(-0.5,0.,-0.866025403784439));
#23256=DIRECTION('',(0.5,0.,0.866025403784439));
#23257=DIRECTION('',(0.,-1.,0.));
#23258=DIRECTION('',(-0.5,0.,-0.866025403784439));
#23259=DIRECTION('center_axis',(-2.40370335797945E-16,0.,1.));
#23260=DIRECTION('ref_axis',(-1.,0.,-2.40370335797945E-16));
#23261=DIRECTION('',(1.,0.,2.40370335797945E-16));
#23262=DIRECTION('',(0.,-1.,0.));
#23263=DIRECTION('',(-1.,0.,-2.40370335797945E-16));
#23264=DIRECTION('center_axis',(0.866025403784439,0.,0.5));
#23265=DIRECTION('ref_axis',(-0.5,0.,0.866025403784439));
#23266=DIRECTION('',(0.5,0.,-0.866025403784439));
#23267=DIRECTION('',(-0.5,0.,0.866025403784439));
#23268=DIRECTION('center_axis',(0.,1.,0.));
#23269=DIRECTION('ref_axis',(1.,0.,0.));
#23270=DIRECTION('center_axis',(0.,-1.,0.));
#23271=DIRECTION('ref_axis',(0.,0.,-1.));
#23272=DIRECTION('center_axis',(0.,1.,0.));
#23273=DIRECTION('ref_axis',(1.,0.,0.));
#23274=DIRECTION('center_axis',(0.,1.,0.));
#23275=DIRECTION('ref_axis',(1.,0.,0.));
#23276=DIRECTION('center_axis',(0.,1.,0.));
#23277=DIRECTION('ref_axis',(0.,0.,1.));
#23278=DIRECTION('center_axis',(0.,-1.,0.));
#23279=DIRECTION('ref_axis',(1.,0.,0.));
#23280=DIRECTION('center_axis',(0.,-1.,0.));
#23281=DIRECTION('ref_axis',(1.,0.,0.));
#23282=DIRECTION('center_axis',(0.,-1.,0.));
#23283=DIRECTION('ref_axis',(1.,0.,0.));
#23284=DIRECTION('',(0.707106781186548,0.707106781186547,8.65956056235493E-17));
#23285=DIRECTION('center_axis',(0.,-1.,0.));
#23286=DIRECTION('ref_axis',(1.,0.,0.));
#23287=DIRECTION('center_axis',(0.,-1.,0.));
#23288=DIRECTION('ref_axis',(1.,0.,0.));
#23289=DIRECTION('',(0.,1.,0.));
#23290=DIRECTION('center_axis',(0.,1.,0.));
#23291=DIRECTION('ref_axis',(1.,0.,0.));
#23292=DIRECTION('center_axis',(0.,-1.,0.));
#23293=DIRECTION('ref_axis',(1.,0.,0.));
#23294=DIRECTION('',(-0.707106781186547,0.707106781186548,-8.65956056235493E-17));
#23295=DIRECTION('center_axis',(0.,-1.,0.));
#23296=DIRECTION('ref_axis',(0.,0.,-1.));
#23297=DIRECTION('center_axis',(0.,-1.,0.));
#23298=DIRECTION('ref_axis',(1.,0.,0.));
#23299=DIRECTION('center_axis',(0.,1.,0.));
#23300=DIRECTION('ref_axis',(1.,0.,0.));
#23301=DIRECTION('center_axis',(0.,1.,0.));
#23302=DIRECTION('ref_axis',(1.,0.,0.));
#23303=DIRECTION('',(-0.447213595499958,0.894427190999916,-5.47678698264203E-17));
#23304=DIRECTION('center_axis',(0.,-1.,0.));
#23305=DIRECTION('ref_axis',(1.,0.,0.));
#23306=DIRECTION('',(0.,1.,0.));
#23307=DIRECTION('axis',(0.,0.,1.));
#23308=DIRECTION('refdir',(1.,0.,0.));
#23309=DIRECTION('axis',(0.,0.,1.));
#23310=DIRECTION('refdir',(1.,0.,0.));
#23311=DIRECTION('center_axis',(0.,-1.,0.));
#23312=DIRECTION('ref_axis',(0.,0.,-1.));
#23313=DIRECTION('center_axis',(0.,-1.,0.));
#23314=DIRECTION('ref_axis',(1.,0.,0.));
#23315=DIRECTION('center_axis',(0.,-1.,0.));
#23316=DIRECTION('ref_axis',(1.,0.,0.));
#23317=DIRECTION('center_axis',(1.,0.,1.22464679914735E-16));
#23318=DIRECTION('ref_axis',(-1.22464679914735E-16,0.,1.));
#23319=DIRECTION('center_axis',(0.,1.,0.));
#23320=DIRECTION('ref_axis',(1.,0.,0.));
#23321=DIRECTION('center_axis',(0.,1.,0.));
#23322=DIRECTION('ref_axis',(1.,0.,0.));
#23323=DIRECTION('center_axis',(0.,-1.,0.));
#23324=DIRECTION('ref_axis',(1.,0.,0.));
#23325=DIRECTION('',(0.,1.,0.));
#23326=DIRECTION('center_axis',(0.,-1.,0.));
#23327=DIRECTION('ref_axis',(1.,0.,0.));
#23328=DIRECTION('center_axis',(0.,-1.,0.));
#23329=DIRECTION('ref_axis',(1.,0.,0.));
#23330=DIRECTION('center_axis',(0.,-1.,0.));
#23331=DIRECTION('ref_axis',(1.,0.,0.));
#23332=DIRECTION('',(0.,1.,0.));
#23333=DIRECTION('center_axis',(0.,-1.,0.));
#23334=DIRECTION('ref_axis',(1.,0.,0.));
#23335=DIRECTION('center_axis',(0.,1.,0.));
#23336=DIRECTION('ref_axis',(1.,0.,0.));
#23337=DIRECTION('',(-0.707106781186548,0.707106781186547,-8.65956056235493E-17));
#23338=DIRECTION('center_axis',(0.,-1.,0.));
#23339=DIRECTION('ref_axis',(1.,0.,0.));
#23340=DIRECTION('center_axis',(0.,1.,0.));
#23341=DIRECTION('ref_axis',(0.,0.,1.));
#23342=DIRECTION('center_axis',(0.,-1.,0.));
#23343=DIRECTION('ref_axis',(1.,0.,0.));
#23344=DIRECTION('center_axis',(0.,-1.,0.));
#23345=DIRECTION('ref_axis',(1.,0.,0.));
#23346=DIRECTION('',(0.,1.,0.));
#23347=DIRECTION('center_axis',(0.,-1.,0.));
#23348=DIRECTION('ref_axis',(0.,0.,-1.));
#23349=DIRECTION('center_axis',(0.,-1.,0.));
#23350=DIRECTION('ref_axis',(1.,0.,0.));
#23351=DIRECTION('center_axis',(0.,-1.,0.));
#23352=DIRECTION('ref_axis',(1.,0.,0.));
#23353=DIRECTION('',(0.707106781186548,0.707106781186547,8.65956056235493E-17));
#23354=DIRECTION('axis',(0.,0.,1.));
#23355=DIRECTION('refdir',(1.,0.,0.));
#23356=DIRECTION('center_axis',(0.,-1.,0.));
#23357=DIRECTION('ref_axis',(0.,0.,-1.));
#23358=DIRECTION('center_axis',(0.,-1.,0.));
#23359=DIRECTION('ref_axis',(1.,0.,0.));
#23360=DIRECTION('center_axis',(0.,-1.,0.));
#23361=DIRECTION('ref_axis',(1.,0.,0.));
#23362=DIRECTION('center_axis',(1.,0.,1.22464679914735E-16));
#23363=DIRECTION('ref_axis',(-1.22464679914735E-16,0.,1.));
#23364=DIRECTION('center_axis',(0.,1.,0.));
#23365=DIRECTION('ref_axis',(1.,0.,0.));
#23366=DIRECTION('center_axis',(0.,1.,0.));
#23367=DIRECTION('ref_axis',(1.,0.,0.));
#23368=DIRECTION('center_axis',(0.,-1.,0.));
#23369=DIRECTION('ref_axis',(1.,0.,0.));
#23370=DIRECTION('center_axis',(0.,-1.,0.));
#23371=DIRECTION('ref_axis',(1.,0.,0.));
#23372=DIRECTION('',(0.,1.,0.));
#23373=DIRECTION('center_axis',(0.,1.,0.));
#23374=DIRECTION('ref_axis',(0.,0.,1.));
#23375=DIRECTION('center_axis',(0.,-1.,0.));
#23376=DIRECTION('ref_axis',(1.,0.,0.));
#23377=DIRECTION('center_axis',(0.,-1.,0.));
#23378=DIRECTION('ref_axis',(1.,0.,0.));
#23379=DIRECTION('center_axis',(0.,-1.,0.));
#23380=DIRECTION('ref_axis',(1.,0.,0.));
#23381=DIRECTION('center_axis',(0.,-1.,0.));
#23382=DIRECTION('ref_axis',(1.,0.,0.));
#23383=DIRECTION('',(0.707106781186548,0.707106781186547,8.65956056235494E-17));
#23384=DIRECTION('center_axis',(0.,-1.,0.));
#23385=DIRECTION('ref_axis',(1.,0.,0.));
#23386=DIRECTION('center_axis',(0.,-1.,0.));
#23387=DIRECTION('ref_axis',(1.,0.,0.));
#23388=DIRECTION('',(0.,1.,0.));
#23389=DIRECTION('center_axis',(0.,1.,0.));
#23390=DIRECTION('ref_axis',(1.,0.,0.));
#23391=DIRECTION('center_axis',(0.,-1.,0.));
#23392=DIRECTION('ref_axis',(1.,0.,0.));
#23393=DIRECTION('',(-0.707106781186548,0.707106781186547,-8.65956056235494E-17));
#23394=DIRECTION('center_axis',(0.,-1.,0.));
#23395=DIRECTION('ref_axis',(0.,0.,-1.));
#23396=DIRECTION('center_axis',(0.,-1.,0.));
#23397=DIRECTION('ref_axis',(1.,0.,0.));
#23398=DIRECTION('',(0.,1.,0.));
#23399=DIRECTION('axis',(0.,0.,1.));
#23400=DIRECTION('refdir',(1.,0.,0.));
#23401=DIRECTION('center_axis',(0.,0.,1.));
#23402=DIRECTION('ref_axis',(1.,0.,0.));
#23403=DIRECTION('center_axis',(1.22464679914735E-16,-1.,0.));
#23404=DIRECTION('ref_axis',(-1.,-1.22464679914735E-16,0.));
#23405=DIRECTION('center_axis',(0.78183148246803,0.,0.623489801858733));
#23406=DIRECTION('ref_axis',(0.623489801858734,0.,-0.78183148246803));
#23407=DIRECTION('center_axis',(7.63554790147315E-17,-1.,-9.57467422477103E-17));
#23408=DIRECTION('ref_axis',(-0.623489801858734,-1.22464679914735E-16,0.78183148246803));
#23409=DIRECTION('center_axis',(0.974927912181824,0.,-0.222520933956314));
#23410=DIRECTION('ref_axis',(-0.222520933956314,0.,-0.974927912181824));
#23411=DIRECTION('center_axis',(-2.7250954951288E-17,-1.,-1.19394234705288E-16));
#23412=DIRECTION('ref_axis',(0.222520933956314,-1.22464679914735E-16,0.974927912181824));
#23413=DIRECTION('center_axis',(0.433883739117558,0.,-0.900968867902419));
#23414=DIRECTION('ref_axis',(-0.900968867902419,0.,-0.433883739117558));
#23415=DIRECTION('center_axis',(-1.10336864020811E-16,-1.,-5.31354332312403E-17));
#23416=DIRECTION('ref_axis',(0.900968867902419,-1.22464679914735E-16,0.433883739117558));
#23417=DIRECTION('center_axis',(-0.433883739117558,0.,-0.900968867902419));
#23418=DIRECTION('ref_axis',(-0.900968867902419,0.,0.433883739117558));
#23419=DIRECTION('center_axis',(-1.10336864020811E-16,-1.,5.31354332312403E-17));
#23420=DIRECTION('ref_axis',(0.900968867902419,-1.22464679914735E-16,-0.433883739117558));
#23421=DIRECTION('center_axis',(-0.974927912181824,0.,-0.222520933956314));
#23422=DIRECTION('ref_axis',(-0.222520933956315,0.,0.974927912181824));
#23423=DIRECTION('center_axis',(-2.7250954951288E-17,-1.,1.19394234705288E-16));
#23424=DIRECTION('ref_axis',(0.222520933956315,-1.22464679914735E-16,-0.974927912181824));
#23425=DIRECTION('center_axis',(-0.78183148246803,0.,0.623489801858734));
#23426=DIRECTION('ref_axis',(0.623489801858733,0.,0.78183148246803));
#23427=DIRECTION('center_axis',(7.63554790147315E-17,-1.,9.57467422477103E-17));
#23428=DIRECTION('ref_axis',(-0.623489801858733,-1.22464679914735E-16,-0.78183148246803));
#23429=DIRECTION('axis',(0.,0.,1.));
#23430=DIRECTION('refdir',(1.,0.,0.));
#23431=DIRECTION('center_axis',(0.,0.,1.));
#23432=DIRECTION('ref_axis',(1.,0.,0.));
#23433=DIRECTION('center_axis',(0.,-1.,0.));
#23434=DIRECTION('ref_axis',(0.,0.,-1.));
#23435=DIRECTION('center_axis',(0.,-1.,0.));
#23436=DIRECTION('ref_axis',(0.,0.,-1.));
#23437=DIRECTION('center_axis',(0.,1.,0.));
#23438=DIRECTION('ref_axis',(1.,0.,0.));
#23439=DIRECTION('center_axis',(0.,1.,0.));
#23440=DIRECTION('ref_axis',(1.,0.,0.));
#23441=DIRECTION('center_axis',(0.,1.,0.));
#23442=DIRECTION('ref_axis',(1.,0.,0.));
#23443=DIRECTION('center_axis',(0.,1.,0.));
#23444=DIRECTION('ref_axis',(1.,0.,0.));
#23445=DIRECTION('',(0.,-1.,0.));
#23446=DIRECTION('center_axis',(0.,-1.,0.));
#23447=DIRECTION('ref_axis',(1.,0.,0.));
#23448=DIRECTION('center_axis',(0.,1.,0.));
#23449=DIRECTION('ref_axis',(1.,0.,0.));
#23450=DIRECTION('center_axis',(0.,1.,0.));
#23451=DIRECTION('ref_axis',(1.,0.,0.));
#23452=DIRECTION('center_axis',(0.,1.,0.));
#23453=DIRECTION('ref_axis',(1.,0.,0.));
#23454=DIRECTION('center_axis',(0.,1.,0.));
#23455=DIRECTION('ref_axis',(1.,0.,0.));
#23456=DIRECTION('center_axis',(0.,1.,0.));
#23457=DIRECTION('ref_axis',(1.,0.,0.));
#23458=DIRECTION('center_axis',(0.,1.,0.));
#23459=DIRECTION('ref_axis',(1.,0.,0.));
#23460=DIRECTION('center_axis',(0.,-1.,0.));
#23461=DIRECTION('ref_axis',(1.,0.,0.));
#23462=DIRECTION('center_axis',(0.,-1.,0.));
#23463=DIRECTION('ref_axis',(0.,0.,-1.));
#23464=DIRECTION('center_axis',(8.96625347776458E-17,0.,1.));
#23465=DIRECTION('ref_axis',(1.,0.,0.));
#23466=DIRECTION('center_axis',(0.,-1.,0.));
#23467=DIRECTION('ref_axis',(0.,0.,-1.));
#23468=DIRECTION('center_axis',(0.,1.,0.));
#23469=DIRECTION('ref_axis',(1.,0.,0.));
#23470=DIRECTION('center_axis',(0.,-1.,0.));
#23471=DIRECTION('ref_axis',(1.,0.,0.));
#23472=DIRECTION('center_axis',(0.,-1.,0.));
#23473=DIRECTION('ref_axis',(0.,0.,-1.));
#23474=DIRECTION('center_axis',(0.,0.,1.));
#23475=DIRECTION('ref_axis',(1.,0.,0.));
#23476=DIRECTION('center_axis',(0.,-1.,0.));
#23477=DIRECTION('ref_axis',(0.,0.,-1.));
#23478=DIRECTION('center_axis',(0.,1.,0.));
#23479=DIRECTION('ref_axis',(1.,0.,0.));
#23480=DIRECTION('center_axis',(0.,-1.,0.));
#23481=DIRECTION('ref_axis',(1.,0.,0.));
#23482=DIRECTION('center_axis',(0.,-1.,0.));
#23483=DIRECTION('ref_axis',(1.,0.,0.));
#23484=DIRECTION('center_axis',(0.,-1.,0.));
#23485=DIRECTION('ref_axis',(0.,0.,-1.));
#23486=DIRECTION('center_axis',(0.,0.,1.));
#23487=DIRECTION('ref_axis',(1.,0.,0.));
#23488=DIRECTION('center_axis',(0.,-1.,0.));
#23489=DIRECTION('ref_axis',(0.,0.,-1.));
#23490=DIRECTION('center_axis',(0.,1.,0.));
#23491=DIRECTION('ref_axis',(1.,0.,0.));
#23492=DIRECTION('center_axis',(0.,-1.,0.));
#23493=DIRECTION('ref_axis',(1.,0.,0.));
#23494=DIRECTION('center_axis',(0.,-1.,0.));
#23495=DIRECTION('ref_axis',(0.,0.,-1.));
#23496=DIRECTION('center_axis',(8.96625347776458E-17,0.,1.));
#23497=DIRECTION('ref_axis',(1.,0.,0.));
#23498=DIRECTION('center_axis',(0.,-1.,0.));
#23499=DIRECTION('ref_axis',(0.,0.,-1.));
#23500=DIRECTION('center_axis',(0.,1.,0.));
#23501=DIRECTION('ref_axis',(1.,0.,0.));
#23502=DIRECTION('center_axis',(0.,-1.,0.));
#23503=DIRECTION('ref_axis',(1.,0.,0.));
#23504=DIRECTION('center_axis',(0.,-1.,0.));
#23505=DIRECTION('ref_axis',(0.,0.,-1.));
#23506=DIRECTION('center_axis',(0.,0.,1.));
#23507=DIRECTION('ref_axis',(1.,0.,0.));
#23508=DIRECTION('center_axis',(0.,-1.,0.));
#23509=DIRECTION('ref_axis',(0.,0.,-1.));
#23510=DIRECTION('center_axis',(0.,1.,0.));
#23511=DIRECTION('ref_axis',(1.,0.,0.));
#23512=DIRECTION('center_axis',(0.,1.,0.));
#23513=DIRECTION('ref_axis',(1.,0.,0.));
#23514=DIRECTION('',(0.,1.,0.));
#23515=DIRECTION('center_axis',(0.,-1.,0.));
#23516=DIRECTION('ref_axis',(1.,0.,0.));
#23517=DIRECTION('center_axis',(0.,-1.,0.));
#23518=DIRECTION('ref_axis',(1.,0.,0.));
#23519=DIRECTION('center_axis',(0.,1.,0.));
#23520=DIRECTION('ref_axis',(1.,0.,0.));
#23521=DIRECTION('center_axis',(0.,-1.,0.));
#23522=DIRECTION('ref_axis',(0.,0.,-1.));
#23523=DIRECTION('center_axis',(0.,0.,1.));
#23524=DIRECTION('ref_axis',(1.,0.,0.));
#23525=DIRECTION('center_axis',(0.,-1.,0.));
#23526=DIRECTION('ref_axis',(0.,0.,-1.));
#23527=DIRECTION('center_axis',(0.,-1.,0.));
#23528=DIRECTION('ref_axis',(-1.,0.,0.));
#23529=DIRECTION('center_axis',(0.,1.,0.));
#23530=DIRECTION('ref_axis',(1.,0.,0.));
#23531=DIRECTION('axis',(0.,0.,1.));
#23532=DIRECTION('refdir',(1.,0.,0.));
#23533=DIRECTION('center_axis',(0.,1.,0.));
#23534=DIRECTION('ref_axis',(0.,0.,1.));
#23535=DIRECTION('center_axis',(0.,-1.,0.));
#23536=DIRECTION('ref_axis',(1.,0.,0.));
#23537=DIRECTION('center_axis',(0.,-1.,0.));
#23538=DIRECTION('ref_axis',(1.,0.,0.));
#23539=DIRECTION('center_axis',(0.,-1.,0.));
#23540=DIRECTION('ref_axis',(1.,0.,0.));
#23541=DIRECTION('center_axis',(0.,-1.,0.));
#23542=DIRECTION('ref_axis',(1.,0.,0.));
#23543=DIRECTION('',(0.,1.,0.));
#23544=DIRECTION('center_axis',(0.,-1.,0.));
#23545=DIRECTION('ref_axis',(0.,0.,-1.));
#23546=DIRECTION('center_axis',(0.,-1.,0.));
#23547=DIRECTION('ref_axis',(1.,0.,0.));
#23548=DIRECTION('center_axis',(0.,-1.,0.));
#23549=DIRECTION('ref_axis',(1.,0.,0.));
#23550=DIRECTION('',(0.,1.,0.));
#23551=DIRECTION('center_axis',(0.,1.,0.));
#23552=DIRECTION('ref_axis',(0.,0.,1.));
#23553=DIRECTION('center_axis',(0.,-1.,0.));
#23554=DIRECTION('ref_axis',(1.,0.,0.));
#23555=DIRECTION('center_axis',(0.,-1.,0.));
#23556=DIRECTION('ref_axis',(1.,0.,0.));
#23557=DIRECTION('center_axis',(0.,-1.,0.));
#23558=DIRECTION('ref_axis',(1.,0.,0.));
#23559=DIRECTION('center_axis',(0.,-1.,0.));
#23560=DIRECTION('ref_axis',(1.,0.,0.));
#23561=DIRECTION('',(0.,1.,0.));
#23562=DIRECTION('center_axis',(0.,-1.,0.));
#23563=DIRECTION('ref_axis',(0.,0.,-1.));
#23564=DIRECTION('center_axis',(0.,-1.,0.));
#23565=DIRECTION('ref_axis',(1.,0.,0.));
#23566=DIRECTION('center_axis',(0.,-1.,0.));
#23567=DIRECTION('ref_axis',(1.,0.,0.));
#23568=DIRECTION('',(0.,1.,0.));
#23569=DIRECTION('',(0.,0.,1.));
#23570=DIRECTION('',(1.,0.,0.));
#23571=DIRECTION('',(0.,0.,1.));
#23572=DIRECTION('',(1.,0.,0.));
#23573=DIRECTION('',(0.,0.,1.));
#23574=DIRECTION('',(1.,0.,0.));
#23575=DIRECTION('',(0.,0.,1.));
#23576=DIRECTION('',(1.,0.,0.));
#23577=DIRECTION('',(0.,0.,1.));
#23578=DIRECTION('',(1.,0.,0.));
#23579=DIRECTION('axis',(0.,0.,1.));
#23580=DIRECTION('refdir',(1.,0.,0.));
#23581=DIRECTION('axis',(0.,0.,1.));
#23582=DIRECTION('refdir',(1.,0.,0.));
#23583=DIRECTION('center_axis',(0.,-1.,0.));
#23584=DIRECTION('ref_axis',(0.,0.,-1.));
#23585=DIRECTION('center_axis',(0.,-1.,0.));
#23586=DIRECTION('ref_axis',(1.,0.,0.));
#23587=DIRECTION('center_axis',(0.,-1.,0.));
#23588=DIRECTION('ref_axis',(1.,0.,0.));
#23589=DIRECTION('center_axis',(1.,0.,1.22464679914735E-16));
#23590=DIRECTION('ref_axis',(-1.22464679914735E-16,0.,1.));
#23591=DIRECTION('center_axis',(0.,1.,0.));
#23592=DIRECTION('ref_axis',(1.,0.,0.));
#23593=DIRECTION('center_axis',(0.,1.,0.));
#23594=DIRECTION('ref_axis',(1.,0.,0.));
#23595=DIRECTION('center_axis',(0.,-1.,0.));
#23596=DIRECTION('ref_axis',(1.,0.,0.));
#23597=DIRECTION('',(0.,1.,0.));
#23598=DIRECTION('center_axis',(0.,-1.,0.));
#23599=DIRECTION('ref_axis',(1.,0.,0.));
#23600=DIRECTION('center_axis',(0.,-1.,0.));
#23601=DIRECTION('ref_axis',(1.,0.,0.));
#23602=DIRECTION('center_axis',(0.,-1.,0.));
#23603=DIRECTION('ref_axis',(1.,0.,0.));
#23604=DIRECTION('',(0.,1.,0.));
#23605=DIRECTION('center_axis',(0.,-1.,0.));
#23606=DIRECTION('ref_axis',(1.,0.,0.));
#23607=DIRECTION('center_axis',(0.,1.,0.));
#23608=DIRECTION('ref_axis',(1.,0.,0.));
#23609=DIRECTION('',(-0.707106781186548,0.707106781186547,-8.65956056235494E-17));
#23610=DIRECTION('center_axis',(0.,-1.,0.));
#23611=DIRECTION('ref_axis',(1.,0.,0.));
#23612=DIRECTION('center_axis',(0.,1.,0.));
#23613=DIRECTION('ref_axis',(0.,0.,1.));
#23614=DIRECTION('center_axis',(0.,-1.,0.));
#23615=DIRECTION('ref_axis',(1.,0.,0.));
#23616=DIRECTION('center_axis',(0.,-1.,0.));
#23617=DIRECTION('ref_axis',(1.,0.,0.));
#23618=DIRECTION('',(0.,1.,0.));
#23619=DIRECTION('center_axis',(0.,-1.,0.));
#23620=DIRECTION('ref_axis',(0.,0.,-1.));
#23621=DIRECTION('center_axis',(0.,-1.,0.));
#23622=DIRECTION('ref_axis',(1.,0.,0.));
#23623=DIRECTION('center_axis',(0.,-1.,0.));
#23624=DIRECTION('ref_axis',(1.,0.,0.));
#23625=DIRECTION('',(0.707106781186548,0.707106781186547,8.65956056235494E-17));
#23626=DIRECTION('axis',(0.,0.,1.));
#23627=DIRECTION('refdir',(1.,0.,0.));
#23628=DIRECTION('center_axis',(0.,-1.,0.));
#23629=DIRECTION('ref_axis',(0.,0.,-1.));
#23630=DIRECTION('center_axis',(0.,-1.,0.));
#23631=DIRECTION('ref_axis',(1.,0.,0.));
#23632=DIRECTION('center_axis',(0.,-1.,0.));
#23633=DIRECTION('ref_axis',(1.,0.,0.));
#23634=DIRECTION('center_axis',(1.,0.,1.22464679914735E-16));
#23635=DIRECTION('ref_axis',(-1.22464679914735E-16,0.,1.));
#23636=DIRECTION('center_axis',(0.,1.,0.));
#23637=DIRECTION('ref_axis',(1.,0.,0.));
#23638=DIRECTION('center_axis',(0.,1.,0.));
#23639=DIRECTION('ref_axis',(1.,0.,0.));
#23640=DIRECTION('center_axis',(0.,-1.,0.));
#23641=DIRECTION('ref_axis',(1.,0.,0.));
#23642=DIRECTION('center_axis',(0.,-1.,0.));
#23643=DIRECTION('ref_axis',(1.,0.,0.));
#23644=DIRECTION('',(0.,1.,0.));
#23645=DIRECTION('center_axis',(0.,1.,0.));
#23646=DIRECTION('ref_axis',(0.,0.,1.));
#23647=DIRECTION('center_axis',(0.,-1.,0.));
#23648=DIRECTION('ref_axis',(1.,0.,0.));
#23649=DIRECTION('center_axis',(0.,-1.,0.));
#23650=DIRECTION('ref_axis',(1.,0.,0.));
#23651=DIRECTION('center_axis',(0.,-1.,0.));
#23652=DIRECTION('ref_axis',(1.,0.,0.));
#23653=DIRECTION('center_axis',(0.,-1.,0.));
#23654=DIRECTION('ref_axis',(1.,0.,0.));
#23655=DIRECTION('',(0.707106781186548,0.707106781186547,8.65956056235494E-17));
#23656=DIRECTION('center_axis',(0.,-1.,0.));
#23657=DIRECTION('ref_axis',(1.,0.,0.));
#23658=DIRECTION('center_axis',(0.,-1.,0.));
#23659=DIRECTION('ref_axis',(1.,0.,0.));
#23660=DIRECTION('',(0.,1.,0.));
#23661=DIRECTION('center_axis',(0.,1.,0.));
#23662=DIRECTION('ref_axis',(1.,0.,0.));
#23663=DIRECTION('center_axis',(0.,-1.,0.));
#23664=DIRECTION('ref_axis',(1.,0.,0.));
#23665=DIRECTION('',(-0.707106781186548,0.707106781186547,-8.65956056235494E-17));
#23666=DIRECTION('center_axis',(0.,-1.,0.));
#23667=DIRECTION('ref_axis',(0.,0.,-1.));
#23668=DIRECTION('center_axis',(0.,-1.,0.));
#23669=DIRECTION('ref_axis',(1.,0.,0.));
#23670=DIRECTION('',(0.,1.,0.));
#23671=DIRECTION('axis',(0.,0.,1.));
#23672=DIRECTION('refdir',(1.,0.,0.));
#23673=DIRECTION('center_axis',(0.,0.,1.));
#23674=DIRECTION('ref_axis',(1.,0.,0.));
#23675=DIRECTION('center_axis',(1.22464679914735E-16,-1.,0.));
#23676=DIRECTION('ref_axis',(-1.,-1.22464679914735E-16,0.));
#23677=DIRECTION('center_axis',(0.707106781186548,0.,0.707106781186548));
#23678=DIRECTION('ref_axis',(0.707106781186548,0.,-0.707106781186548));
#23679=DIRECTION('center_axis',(8.65956056235493E-17,-1.,-8.65956056235493E-17));
#23680=DIRECTION('ref_axis',(-0.707106781186548,-1.22464679914735E-16,0.707106781186548));
#23681=DIRECTION('center_axis',(1.,0.,0.));
#23682=DIRECTION('ref_axis',(6.12323399573677E-17,0.,-1.));
#23683=DIRECTION('center_axis',(7.49879891330929E-33,-1.,-1.22464679914735E-16));
#23684=DIRECTION('ref_axis',(-6.12323399573677E-17,-1.22464679914735E-16,
1.));
#23685=DIRECTION('center_axis',(0.707106781186548,0.,-0.707106781186548));
#23686=DIRECTION('ref_axis',(-0.707106781186548,0.,-0.707106781186548));
#23687=DIRECTION('center_axis',(-8.65956056235493E-17,-1.,-8.65956056235493E-17));
#23688=DIRECTION('ref_axis',(0.707106781186548,-1.22464679914735E-16,0.707106781186548));
#23689=DIRECTION('center_axis',(0.,0.,-1.));
#23690=DIRECTION('ref_axis',(-1.,0.,-1.22464679914735E-16));
#23691=DIRECTION('center_axis',(-1.22464679914735E-16,-1.,-1.49975978266186E-32));
#23692=DIRECTION('ref_axis',(1.,-1.22464679914735E-16,1.22464679914735E-16));
#23693=DIRECTION('center_axis',(-0.707106781186548,0.,-0.707106781186548));
#23694=DIRECTION('ref_axis',(-0.707106781186548,0.,0.707106781186548));
#23695=DIRECTION('center_axis',(-8.65956056235493E-17,-1.,8.65956056235493E-17));
#23696=DIRECTION('ref_axis',(0.707106781186548,-1.22464679914735E-16,-0.707106781186548));
#23697=DIRECTION('center_axis',(-1.,0.,0.));
#23698=DIRECTION('ref_axis',(-1.83697019872103E-16,0.,1.));
#23699=DIRECTION('center_axis',(-2.24963967399279E-32,-1.,1.22464679914735E-16));
#23700=DIRECTION('ref_axis',(1.83697019872103E-16,-1.22464679914735E-16,
-1.));
#23701=DIRECTION('center_axis',(-0.707106781186548,0.,0.707106781186548));
#23702=DIRECTION('ref_axis',(0.707106781186548,0.,0.707106781186548));
#23703=DIRECTION('center_axis',(8.65956056235493E-17,-1.,8.65956056235494E-17));
#23704=DIRECTION('ref_axis',(-0.707106781186548,-1.22464679914735E-16,-0.707106781186548));
#23705=DIRECTION('axis',(0.,0.,1.));
#23706=DIRECTION('refdir',(1.,0.,0.));
#23707=DIRECTION('center_axis',(0.,0.,1.));
#23708=DIRECTION('ref_axis',(1.,0.,0.));
#23709=DIRECTION('center_axis',(0.,-1.,0.));
#23710=DIRECTION('ref_axis',(0.,0.,-1.));
#23711=DIRECTION('center_axis',(0.,-1.,0.));
#23712=DIRECTION('ref_axis',(0.,0.,-1.));
#23713=DIRECTION('center_axis',(0.,1.,0.));
#23714=DIRECTION('ref_axis',(1.,0.,0.));
#23715=DIRECTION('center_axis',(0.,1.,0.));
#23716=DIRECTION('ref_axis',(1.,0.,0.));
#23717=DIRECTION('center_axis',(0.,1.,0.));
#23718=DIRECTION('ref_axis',(1.,0.,0.));
#23719=DIRECTION('center_axis',(0.,1.,0.));
#23720=DIRECTION('ref_axis',(1.,0.,0.));
#23721=DIRECTION('',(0.,-1.,0.));
#23722=DIRECTION('center_axis',(0.,-1.,0.));
#23723=DIRECTION('ref_axis',(1.,0.,0.));
#23724=DIRECTION('center_axis',(0.,1.,0.));
#23725=DIRECTION('ref_axis',(1.,0.,0.));
#23726=DIRECTION('center_axis',(0.,1.,0.));
#23727=DIRECTION('ref_axis',(1.,0.,0.));
#23728=DIRECTION('center_axis',(0.,1.,0.));
#23729=DIRECTION('ref_axis',(1.,0.,0.));
#23730=DIRECTION('center_axis',(0.,1.,0.));
#23731=DIRECTION('ref_axis',(1.,0.,0.));
#23732=DIRECTION('center_axis',(0.,1.,0.));
#23733=DIRECTION('ref_axis',(1.,0.,0.));
#23734=DIRECTION('center_axis',(0.,1.,0.));
#23735=DIRECTION('ref_axis',(1.,0.,0.));
#23736=DIRECTION('center_axis',(0.,-1.,0.));
#23737=DIRECTION('ref_axis',(1.,0.,0.));
#23738=DIRECTION('center_axis',(0.,-1.,0.));
#23739=DIRECTION('ref_axis',(0.,0.,-1.));
#23740=DIRECTION('center_axis',(6.12323399573677E-17,0.,1.));
#23741=DIRECTION('ref_axis',(1.,0.,0.));
#23742=DIRECTION('center_axis',(0.,-1.,0.));
#23743=DIRECTION('ref_axis',(0.,0.,-1.));
#23744=DIRECTION('center_axis',(0.,1.,0.));
#23745=DIRECTION('ref_axis',(1.,0.,0.));
#23746=DIRECTION('center_axis',(0.,-1.,0.));
#23747=DIRECTION('ref_axis',(1.,0.,0.));
#23748=DIRECTION('center_axis',(0.,-1.,0.));
#23749=DIRECTION('ref_axis',(0.,0.,-1.));
#23750=DIRECTION('center_axis',(0.,0.,1.));
#23751=DIRECTION('ref_axis',(1.,0.,0.));
#23752=DIRECTION('center_axis',(0.,-1.,0.));
#23753=DIRECTION('ref_axis',(0.,0.,-1.));
#23754=DIRECTION('center_axis',(0.,1.,0.));
#23755=DIRECTION('ref_axis',(1.,0.,0.));
#23756=DIRECTION('center_axis',(0.,-1.,0.));
#23757=DIRECTION('ref_axis',(1.,0.,0.));
#23758=DIRECTION('center_axis',(0.,-1.,0.));
#23759=DIRECTION('ref_axis',(0.,0.,-1.));
#23760=DIRECTION('center_axis',(0.,0.,1.));
#23761=DIRECTION('ref_axis',(1.,0.,0.));
#23762=DIRECTION('center_axis',(0.,-1.,0.));
#23763=DIRECTION('ref_axis',(0.,0.,-1.));
#23764=DIRECTION('center_axis',(0.,1.,0.));
#23765=DIRECTION('ref_axis',(1.,0.,0.));
#23766=DIRECTION('center_axis',(0.,-1.,0.));
#23767=DIRECTION('ref_axis',(1.,0.,0.));
#23768=DIRECTION('center_axis',(0.,-1.,0.));
#23769=DIRECTION('ref_axis',(0.,0.,-1.));
#23770=DIRECTION('center_axis',(0.,0.,1.));
#23771=DIRECTION('ref_axis',(1.,0.,0.));
#23772=DIRECTION('center_axis',(0.,-1.,0.));
#23773=DIRECTION('ref_axis',(0.,0.,-1.));
#23774=DIRECTION('center_axis',(0.,1.,0.));
#23775=DIRECTION('ref_axis',(1.,0.,0.));
#23776=DIRECTION('center_axis',(0.,-1.,0.));
#23777=DIRECTION('ref_axis',(1.,0.,0.));
#23778=DIRECTION('center_axis',(0.,-1.,0.));
#23779=DIRECTION('ref_axis',(0.,0.,-1.));
#23780=DIRECTION('center_axis',(6.12323399573676E-17,0.,1.));
#23781=DIRECTION('ref_axis',(1.,0.,0.));
#23782=DIRECTION('center_axis',(0.,-1.,0.));
#23783=DIRECTION('ref_axis',(0.,0.,-1.));
#23784=DIRECTION('center_axis',(0.,1.,0.));
#23785=DIRECTION('ref_axis',(1.,0.,0.));
#23786=DIRECTION('center_axis',(0.,-1.,0.));
#23787=DIRECTION('ref_axis',(1.,0.,0.));
#23788=DIRECTION('center_axis',(0.,-1.,0.));
#23789=DIRECTION('ref_axis',(0.,0.,-1.));
#23790=DIRECTION('center_axis',(0.,0.,1.));
#23791=DIRECTION('ref_axis',(1.,0.,0.));
#23792=DIRECTION('center_axis',(0.,-1.,0.));
#23793=DIRECTION('ref_axis',(0.,0.,-1.));
#23794=DIRECTION('center_axis',(0.,1.,0.));
#23795=DIRECTION('ref_axis',(1.,0.,0.));
#23796=DIRECTION('center_axis',(0.,1.,0.));
#23797=DIRECTION('ref_axis',(1.,0.,0.));
#23798=DIRECTION('',(0.,1.,0.));
#23799=DIRECTION('center_axis',(0.,-1.,0.));
#23800=DIRECTION('ref_axis',(1.,0.,0.));
#23801=DIRECTION('center_axis',(0.,-1.,0.));
#23802=DIRECTION('ref_axis',(1.,0.,0.));
#23803=DIRECTION('center_axis',(0.,1.,0.));
#23804=DIRECTION('ref_axis',(1.,0.,0.));
#23805=DIRECTION('center_axis',(0.,-1.,0.));
#23806=DIRECTION('ref_axis',(0.,0.,-1.));
#23807=DIRECTION('center_axis',(0.,0.,1.));
#23808=DIRECTION('ref_axis',(1.,0.,0.));
#23809=DIRECTION('center_axis',(0.,-1.,0.));
#23810=DIRECTION('ref_axis',(0.,0.,-1.));
#23811=DIRECTION('center_axis',(0.,-1.,0.));
#23812=DIRECTION('ref_axis',(-1.,0.,0.));
#23813=DIRECTION('center_axis',(0.,1.,0.));
#23814=DIRECTION('ref_axis',(1.,0.,0.));
#23815=DIRECTION('axis',(0.,0.,1.));
#23816=DIRECTION('refdir',(1.,0.,0.));
#23817=DIRECTION('center_axis',(0.,1.,0.));
#23818=DIRECTION('ref_axis',(0.,0.,1.));
#23819=DIRECTION('center_axis',(0.,-1.,0.));
#23820=DIRECTION('ref_axis',(1.,0.,0.));
#23821=DIRECTION('center_axis',(0.,-1.,0.));
#23822=DIRECTION('ref_axis',(1.,0.,0.));
#23823=DIRECTION('center_axis',(0.,-1.,0.));
#23824=DIRECTION('ref_axis',(1.,0.,0.));
#23825=DIRECTION('center_axis',(0.,-1.,0.));
#23826=DIRECTION('ref_axis',(1.,0.,0.));
#23827=DIRECTION('',(0.,1.,0.));
#23828=DIRECTION('center_axis',(0.,-1.,0.));
#23829=DIRECTION('ref_axis',(0.,0.,-1.));
#23830=DIRECTION('center_axis',(0.,-1.,0.));
#23831=DIRECTION('ref_axis',(1.,0.,0.));
#23832=DIRECTION('center_axis',(0.,-1.,0.));
#23833=DIRECTION('ref_axis',(1.,0.,0.));
#23834=DIRECTION('',(0.,1.,0.));
#23835=DIRECTION('center_axis',(0.,1.,0.));
#23836=DIRECTION('ref_axis',(0.,0.,1.));
#23837=DIRECTION('center_axis',(0.,-1.,0.));
#23838=DIRECTION('ref_axis',(1.,0.,0.));
#23839=DIRECTION('center_axis',(0.,-1.,0.));
#23840=DIRECTION('ref_axis',(1.,0.,0.));
#23841=DIRECTION('center_axis',(0.,-1.,0.));
#23842=DIRECTION('ref_axis',(1.,0.,0.));
#23843=DIRECTION('center_axis',(0.,-1.,0.));
#23844=DIRECTION('ref_axis',(1.,0.,0.));
#23845=DIRECTION('',(0.,1.,0.));
#23846=DIRECTION('center_axis',(0.,-1.,0.));
#23847=DIRECTION('ref_axis',(0.,0.,-1.));
#23848=DIRECTION('center_axis',(0.,-1.,0.));
#23849=DIRECTION('ref_axis',(1.,0.,0.));
#23850=DIRECTION('center_axis',(0.,-1.,0.));
#23851=DIRECTION('ref_axis',(1.,0.,0.));
#23852=DIRECTION('',(0.,1.,0.));
#23853=DIRECTION('',(0.,0.,1.));
#23854=DIRECTION('',(1.,0.,0.));
#23855=DIRECTION('',(0.,0.,1.));
#23856=DIRECTION('',(1.,0.,0.));
#23857=DIRECTION('',(0.,0.,1.));
#23858=DIRECTION('',(1.,0.,0.));
#23859=DIRECTION('',(0.,0.,1.));
#23860=DIRECTION('',(1.,0.,0.));
#23861=DIRECTION('',(0.,0.,1.));
#23862=DIRECTION('',(1.,0.,0.));
#23863=DIRECTION('axis',(0.,0.,1.));
#23864=DIRECTION('refdir',(1.,0.,0.));
#23865=DIRECTION('center_axis',(0.,1.,0.));
#23866=DIRECTION('ref_axis',(1.,0.,0.));
#23867=DIRECTION('center_axis',(0.,1.,0.));
#23868=DIRECTION('ref_axis',(1.,0.,0.));
#23869=DIRECTION('center_axis',(0.,1.,0.));
#23870=DIRECTION('ref_axis',(1.,0.,0.));
#23871=DIRECTION('center_axis',(0.,1.,0.));
#23872=DIRECTION('ref_axis',(1.,0.,0.));
#23873=DIRECTION('center_axis',(0.,1.,0.));
#23874=DIRECTION('ref_axis',(1.,0.,0.));
#23875=DIRECTION('center_axis',(0.,1.,0.));
#23876=DIRECTION('ref_axis',(1.,0.,0.));
#23877=DIRECTION('',(0.,-1.,0.));
#23878=DIRECTION('center_axis',(0.,1.,0.));
#23879=DIRECTION('ref_axis',(0.,0.,1.));
#23880=DIRECTION('center_axis',(0.,-1.,0.));
#23881=DIRECTION('ref_axis',(1.,0.,0.));
#23882=DIRECTION('center_axis',(0.,-1.,0.));
#23883=DIRECTION('ref_axis',(1.,0.,0.));
#23884=DIRECTION('center_axis',(0.,-1.,0.));
#23885=DIRECTION('ref_axis',(1.,0.,0.));
#23886=DIRECTION('',(0.707106781186548,0.707106781186547,8.65956056235493E-17));
#23887=DIRECTION('center_axis',(0.,-1.,0.));
#23888=DIRECTION('ref_axis',(1.,0.,0.));
#23889=DIRECTION('center_axis',(0.,-1.,0.));
#23890=DIRECTION('ref_axis',(1.,0.,0.));
#23891=DIRECTION('',(0.,1.,0.));
#23892=DIRECTION('center_axis',(0.,1.,0.));
#23893=DIRECTION('ref_axis',(1.,0.,0.));
#23894=DIRECTION('center_axis',(0.,-1.,0.));
#23895=DIRECTION('ref_axis',(1.,0.,0.));
#23896=DIRECTION('',(-0.707106781186547,0.707106781186548,-8.65956056235493E-17));
#23897=DIRECTION('center_axis',(0.,-1.,0.));
#23898=DIRECTION('ref_axis',(0.,0.,-1.));
#23899=DIRECTION('center_axis',(0.,-1.,0.));
#23900=DIRECTION('ref_axis',(1.,0.,0.));
#23901=DIRECTION('center_axis',(0.,1.,0.));
#23902=DIRECTION('ref_axis',(1.,0.,0.));
#23903=DIRECTION('center_axis',(0.,1.,0.));
#23904=DIRECTION('ref_axis',(1.,0.,0.));
#23905=DIRECTION('',(-0.447213595499958,0.894427190999916,-5.47678698264203E-17));
#23906=DIRECTION('center_axis',(0.,-1.,0.));
#23907=DIRECTION('ref_axis',(1.,0.,0.));
#23908=DIRECTION('',(0.,1.,0.));
#23909=DIRECTION('center_axis',(0.866025403784439,0.,-0.5));
#23910=DIRECTION('ref_axis',(0.5,0.,0.866025403784439));
#23911=DIRECTION('',(-0.5,0.,-0.866025403784439));
#23912=DIRECTION('',(0.,-1.,0.));
#23913=DIRECTION('',(0.5,0.,0.866025403784439));
#23914=DIRECTION('',(0.,-1.,0.));
#23915=DIRECTION('center_axis',(1.20185167898973E-16,0.,-1.));
#23916=DIRECTION('ref_axis',(1.,0.,1.20185167898973E-16));
#23917=DIRECTION('',(-1.,0.,-1.20185167898973E-16));
#23918=DIRECTION('',(0.,-1.,0.));
#23919=DIRECTION('',(1.,0.,1.20185167898973E-16));
#23920=DIRECTION('center_axis',(-0.866025403784439,0.,-0.5));
#23921=DIRECTION('ref_axis',(0.5,0.,-0.866025403784439));
#23922=DIRECTION('',(-0.5,0.,0.866025403784439));
#23923=DIRECTION('',(0.,-1.,0.));
#23924=DIRECTION('',(0.5,0.,-0.866025403784439));
#23925=DIRECTION('center_axis',(-0.866025403784439,0.,0.5));
#23926=DIRECTION('ref_axis',(-0.5,0.,-0.866025403784439));
#23927=DIRECTION('',(0.5,0.,0.866025403784439));
#23928=DIRECTION('',(0.,-1.,0.));
#23929=DIRECTION('',(-0.5,0.,-0.866025403784439));
#23930=DIRECTION('center_axis',(-2.40370335797945E-16,0.,1.));
#23931=DIRECTION('ref_axis',(-1.,0.,-2.40370335797945E-16));
#23932=DIRECTION('',(1.,0.,2.40370335797945E-16));
#23933=DIRECTION('',(0.,-1.,0.));
#23934=DIRECTION('',(-1.,0.,-2.40370335797945E-16));
#23935=DIRECTION('center_axis',(0.866025403784439,0.,0.5));
#23936=DIRECTION('ref_axis',(-0.5,0.,0.866025403784439));
#23937=DIRECTION('',(0.5,0.,-0.866025403784439));
#23938=DIRECTION('',(-0.5,0.,0.866025403784439));
#23939=DIRECTION('center_axis',(0.,1.,0.));
#23940=DIRECTION('ref_axis',(1.,0.,0.));
#23941=DIRECTION('center_axis',(0.,-1.,0.));
#23942=DIRECTION('ref_axis',(0.,0.,-1.));
#23943=DIRECTION('axis',(0.,0.,1.));
#23944=DIRECTION('refdir',(1.,0.,0.));
#23945=DIRECTION('center_axis',(0.866025403784439,0.,-0.5));
#23946=DIRECTION('ref_axis',(0.5,0.,0.866025403784439));
#23947=DIRECTION('',(-0.5,0.,-0.866025403784439));
#23948=DIRECTION('',(0.,-1.,0.));
#23949=DIRECTION('',(0.5,0.,0.866025403784439));
#23950=DIRECTION('',(0.,-1.,0.));
#23951=DIRECTION('center_axis',(1.60246890531964E-16,0.,-1.));
#23952=DIRECTION('ref_axis',(1.,0.,1.60246890531964E-16));
#23953=DIRECTION('',(-1.,0.,-1.60246890531964E-16));
#23954=DIRECTION('',(0.,-1.,0.));
#23955=DIRECTION('',(1.,0.,1.60246890531964E-16));
#23956=DIRECTION('center_axis',(-0.866025403784439,0.,-0.5));
#23957=DIRECTION('ref_axis',(0.5,0.,-0.866025403784439));
#23958=DIRECTION('',(-0.5,0.,0.866025403784439));
#23959=DIRECTION('',(0.,-1.,0.));
#23960=DIRECTION('',(0.5,0.,-0.866025403784439));
#23961=DIRECTION('center_axis',(-0.866025403784439,0.,0.5));
#23962=DIRECTION('ref_axis',(-0.5,0.,-0.866025403784439));
#23963=DIRECTION('',(0.5,0.,0.866025403784439));
#23964=DIRECTION('',(0.,-1.,0.));
#23965=DIRECTION('',(-0.5,0.,-0.866025403784439));
#23966=DIRECTION('center_axis',(-1.60246890531964E-16,0.,1.));
#23967=DIRECTION('ref_axis',(-1.,0.,-1.60246890531964E-16));
#23968=DIRECTION('',(1.,0.,1.60246890531964E-16));
#23969=DIRECTION('',(0.,-1.,0.));
#23970=DIRECTION('',(-1.,0.,-1.60246890531964E-16));
#23971=DIRECTION('center_axis',(0.866025403784439,0.,0.5));
#23972=DIRECTION('ref_axis',(-0.5,0.,0.866025403784439));
#23973=DIRECTION('',(0.5,0.,-0.866025403784439));
#23974=DIRECTION('',(-0.5,0.,0.866025403784439));
#23975=DIRECTION('center_axis',(0.,1.,0.));
#23976=DIRECTION('ref_axis',(1.,0.,0.));
#23977=DIRECTION('center_axis',(0.,-1.,0.));
#23978=DIRECTION('ref_axis',(0.,0.,-1.));
#23979=DIRECTION('center_axis',(0.,1.,0.));
#23980=DIRECTION('ref_axis',(1.,0.,0.));
#23981=DIRECTION('center_axis',(0.,1.,0.));
#23982=DIRECTION('ref_axis',(1.,0.,0.));
#23983=DIRECTION('center_axis',(0.,1.,0.));
#23984=DIRECTION('ref_axis',(0.,0.,1.));
#23985=DIRECTION('center_axis',(0.,-1.,0.));
#23986=DIRECTION('ref_axis',(1.,0.,0.));
#23987=DIRECTION('center_axis',(0.,-1.,0.));
#23988=DIRECTION('ref_axis',(1.,0.,0.));
#23989=DIRECTION('center_axis',(0.,-1.,0.));
#23990=DIRECTION('ref_axis',(1.,0.,0.));
#23991=DIRECTION('',(0.707106781186547,0.707106781186548,8.65956056235493E-17));
#23992=DIRECTION('center_axis',(0.,-1.,0.));
#23993=DIRECTION('ref_axis',(1.,0.,0.));
#23994=DIRECTION('center_axis',(0.,-1.,0.));
#23995=DIRECTION('ref_axis',(1.,0.,0.));
#23996=DIRECTION('',(0.,1.,0.));
#23997=DIRECTION('center_axis',(0.,1.,0.));
#23998=DIRECTION('ref_axis',(1.,0.,0.));
#23999=DIRECTION('center_axis',(0.,-1.,0.));
#24000=DIRECTION('ref_axis',(1.,0.,0.));
#24001=DIRECTION('',(-0.707106781186547,0.707106781186548,-8.65956056235493E-17));
#24002=DIRECTION('center_axis',(0.,-1.,0.));
#24003=DIRECTION('ref_axis',(0.,0.,-1.));
#24004=DIRECTION('center_axis',(0.,-1.,0.));
#24005=DIRECTION('ref_axis',(1.,0.,0.));
#24006=DIRECTION('center_axis',(0.,1.,0.));
#24007=DIRECTION('ref_axis',(1.,0.,0.));
#24008=DIRECTION('center_axis',(0.,1.,0.));
#24009=DIRECTION('ref_axis',(1.,0.,0.));
#24010=DIRECTION('',(-0.447213595499958,0.894427190999916,-5.47678698264203E-17));
#24011=DIRECTION('center_axis',(0.,-1.,0.));
#24012=DIRECTION('ref_axis',(1.,0.,0.));
#24013=DIRECTION('',(0.,1.,0.));
#24014=DIRECTION('axis',(0.,0.,1.));
#24015=DIRECTION('refdir',(1.,0.,0.));
#24016=DIRECTION('center_axis',(0.,0.,-1.));
#24017=DIRECTION('ref_axis',(0.,1.,0.));
#24018=DIRECTION('',(0.,1.,0.));
#24019=DIRECTION('',(1.,0.,0.));
#24020=DIRECTION('',(0.,-1.,0.));
#24021=DIRECTION('',(1.,0.,0.));
#24022=DIRECTION('center_axis',(0.,1.,-8.88178419700125E-16));
#24023=DIRECTION('ref_axis',(0.,8.88178419700125E-16,1.));
#24024=DIRECTION('',(0.,8.88178419700125E-16,1.));
#24025=DIRECTION('',(1.,0.,0.));
#24026=DIRECTION('',(0.,-8.88178419700125E-16,-1.));
#24027=DIRECTION('center_axis',(0.,-7.40148683083439E-16,-1.));
#24028=DIRECTION('ref_axis',(0.,1.,-7.40148683083439E-16));
#24029=DIRECTION('',(0.,1.,-7.40148683083439E-16));
#24030=DIRECTION('',(1.,0.,0.));
#24031=DIRECTION('',(0.,-1.,7.40148683083439E-16));
#24032=DIRECTION('center_axis',(0.,-0.707106781186547,-0.707106781186548));
#24033=DIRECTION('ref_axis',(0.,0.707106781186548,-0.707106781186547));
#24034=DIRECTION('',(0.,0.707106781186548,-0.707106781186547));
#24035=DIRECTION('',(1.,0.,0.));
#24036=DIRECTION('',(0.,-0.707106781186548,0.707106781186547));
#24037=DIRECTION('center_axis',(0.,-1.,2.77555756156289E-16));
#24038=DIRECTION('ref_axis',(0.,-2.77555756156289E-16,-1.));
#24039=DIRECTION('',(0.,-2.77555756156289E-16,-1.));
#24040=DIRECTION('',(1.,0.,0.));
#24041=DIRECTION('',(0.,2.77555756156289E-16,1.));
#24042=DIRECTION('center_axis',(0.,-0.707106781186547,0.707106781186548));
#24043=DIRECTION('ref_axis',(0.,-0.707106781186548,-0.707106781186547));
#24044=DIRECTION('',(0.,-0.707106781186548,-0.707106781186547));
#24045=DIRECTION('',(1.,0.,0.));
#24046=DIRECTION('',(0.,0.707106781186548,0.707106781186547));
#24047=DIRECTION('center_axis',(0.,7.40148683083438E-16,1.));
#24048=DIRECTION('ref_axis',(0.,-1.,7.40148683083438E-16));
#24049=DIRECTION('',(0.,-1.,7.40148683083438E-16));
#24050=DIRECTION('',(1.,0.,0.));
#24051=DIRECTION('',(0.,1.,-7.40148683083438E-16));
#24052=DIRECTION('center_axis',(0.,1.,-4.44089209850063E-16));
#24053=DIRECTION('ref_axis',(0.,4.44089209850063E-16,1.));
#24054=DIRECTION('',(0.,4.44089209850063E-16,1.));
#24055=DIRECTION('',(1.,0.,0.));
#24056=DIRECTION('',(0.,-4.44089209850063E-16,-1.));
#24057=DIRECTION('center_axis',(0.,2.41352831440251E-16,1.));
#24058=DIRECTION('ref_axis',(0.,-1.,2.41352831440251E-16));
#24059=DIRECTION('',(0.,-1.,2.41352831440251E-16));
#24060=DIRECTION('',(-1.,0.,0.));
#24061=DIRECTION('',(0.,1.,-2.41352831440251E-16));
#24062=DIRECTION('center_axis',(0.,-1.,2.41352831440251E-16));
#24063=DIRECTION('ref_axis',(0.,-2.41352831440251E-16,-1.));
#24064=DIRECTION('',(0.,-2.41352831440251E-16,-1.));
#24065=DIRECTION('',(1.,0.,0.));
#24066=DIRECTION('',(0.,2.41352831440251E-16,1.));
#24067=DIRECTION('',(1.,0.,0.));
#24068=DIRECTION('center_axis',(0.,0.,-1.));
#24069=DIRECTION('ref_axis',(0.,1.,0.));
#24070=DIRECTION('',(0.,1.,0.));
#24071=DIRECTION('',(1.,0.,0.));
#24072=DIRECTION('',(0.,-1.,0.));
#24073=DIRECTION('center_axis',(0.,-1.,0.));
#24074=DIRECTION('ref_axis',(0.,0.,-1.));
#24075=DIRECTION('',(0.,0.,-1.));
#24076=DIRECTION('',(1.,0.,0.));
#24077=DIRECTION('',(0.,0.,1.));
#24078=DIRECTION('center_axis',(0.,-0.707106781186547,0.707106781186548));
#24079=DIRECTION('ref_axis',(0.,-0.707106781186548,-0.707106781186547));
#24080=DIRECTION('',(0.,-0.707106781186548,-0.707106781186547));
#24081=DIRECTION('',(1.,0.,0.));
#24082=DIRECTION('',(0.,0.707106781186548,0.707106781186547));
#24083=DIRECTION('center_axis',(0.,0.,1.));
#24084=DIRECTION('ref_axis',(0.,-1.,0.));
#24085=DIRECTION('',(0.,-1.,0.));
#24086=DIRECTION('',(1.,0.,0.));
#24087=DIRECTION('',(0.,1.,0.));
#24088=DIRECTION('center_axis',(0.,0.707106781186548,0.707106781186547));
#24089=DIRECTION('ref_axis',(0.,-0.707106781186547,0.707106781186548));
#24090=DIRECTION('',(0.,-0.707106781186547,0.707106781186548));
#24091=DIRECTION('',(1.,0.,0.));
#24092=DIRECTION('',(0.,0.707106781186547,-0.707106781186548));
#24093=DIRECTION('center_axis',(0.,1.,0.));
#24094=DIRECTION('ref_axis',(0.,0.,1.));
#24095=DIRECTION('',(0.,0.,1.));
#24096=DIRECTION('',(1.,0.,0.));
#24097=DIRECTION('',(0.,0.,-1.));
#24098=DIRECTION('center_axis',(0.,0.,-1.));
#24099=DIRECTION('ref_axis',(0.,1.,0.));
#24100=DIRECTION('',(0.,1.,0.));
#24101=DIRECTION('',(1.,0.,0.));
#24102=DIRECTION('',(0.,-1.,0.));
#24103=DIRECTION('center_axis',(0.,1.,-2.41352831440251E-16));
#24104=DIRECTION('ref_axis',(0.,2.41352831440251E-16,1.));
#24105=DIRECTION('',(0.,2.41352831440251E-16,1.));
#24106=DIRECTION('',(-1.,0.,0.));
#24107=DIRECTION('',(0.,-2.41352831440251E-16,-1.));
#24108=DIRECTION('center_axis',(0.,0.,1.));
#24109=DIRECTION('ref_axis',(0.,-1.,0.));
#24110=DIRECTION('',(0.,-1.,0.));
#24111=DIRECTION('',(1.,0.,0.));
#24112=DIRECTION('',(0.,1.,0.));
#24113=DIRECTION('',(1.,0.,0.));
#24114=DIRECTION('center_axis',(0.,-1.,0.));
#24115=DIRECTION('ref_axis',(0.,0.,-1.));
#24116=DIRECTION('',(0.,0.,-1.));
#24117=DIRECTION('',(1.,0.,0.));
#24118=DIRECTION('',(0.,0.,1.));
#24119=DIRECTION('center_axis',(0.,0.,1.));
#24120=DIRECTION('ref_axis',(0.,-1.,0.));
#24121=DIRECTION('',(0.,-1.,0.));
#24122=DIRECTION('',(1.,0.,0.));
#24123=DIRECTION('',(0.,1.,0.));
#24124=DIRECTION('center_axis',(0.,0.707106781186548,0.707106781186548));
#24125=DIRECTION('ref_axis',(0.,-0.707106781186548,0.707106781186548));
#24126=DIRECTION('',(0.,-0.707106781186548,0.707106781186548));
#24127=DIRECTION('',(1.,0.,0.));
#24128=DIRECTION('',(0.,0.707106781186548,-0.707106781186548));
#24129=DIRECTION('center_axis',(0.,1.,0.));
#24130=DIRECTION('ref_axis',(0.,0.,1.));
#24131=DIRECTION('',(0.,0.,1.));
#24132=DIRECTION('',(1.,0.,0.));
#24133=DIRECTION('',(0.,0.,-1.));
#24134=DIRECTION('center_axis',(0.,0.707106781186548,-0.707106781186547));
#24135=DIRECTION('ref_axis',(0.,0.707106781186547,0.707106781186548));
#24136=DIRECTION('',(0.,0.707106781186547,0.707106781186548));
#24137=DIRECTION('',(1.,0.,0.));
#24138=DIRECTION('',(0.,-0.707106781186547,-0.707106781186548));
#24139=DIRECTION('center_axis',(0.,-7.40148683083438E-16,-1.));
#24140=DIRECTION('ref_axis',(0.,1.,-7.40148683083438E-16));
#24141=DIRECTION('',(0.,1.,-7.40148683083438E-16));
#24142=DIRECTION('',(1.,0.,0.));
#24143=DIRECTION('',(0.,-1.,7.40148683083438E-16));
#24144=DIRECTION('center_axis',(0.,-1.,0.));
#24145=DIRECTION('ref_axis',(0.,0.,-1.));
#24146=DIRECTION('',(0.,0.,-1.));
#24147=DIRECTION('',(1.,0.,0.));
#24148=DIRECTION('',(0.,0.,1.));
#24149=DIRECTION('center_axis',(0.,0.,-1.));
#24150=DIRECTION('ref_axis',(0.,1.,0.));
#24151=DIRECTION('',(0.,1.,0.));
#24152=DIRECTION('',(-1.,0.,0.));
#24153=DIRECTION('',(0.,-1.,0.));
#24154=DIRECTION('center_axis',(0.,1.,0.));
#24155=DIRECTION('ref_axis',(0.,0.,1.));
#24156=DIRECTION('',(0.,0.,1.));
#24157=DIRECTION('',(1.,0.,0.));
#24158=DIRECTION('',(0.,0.,-1.));
#24159=DIRECTION('',(1.,0.,0.));
#24160=DIRECTION('center_axis',(0.,0.,1.));
#24161=DIRECTION('ref_axis',(0.,-1.,0.));
#24162=DIRECTION('',(0.,-1.,0.));
#24163=DIRECTION('',(1.,0.,0.));
#24164=DIRECTION('',(0.,1.,0.));
#24165=DIRECTION('center_axis',(0.,1.,0.));
#24166=DIRECTION('ref_axis',(0.,0.,1.));
#24167=DIRECTION('',(0.,0.,1.));
#24168=DIRECTION('',(1.,0.,0.));
#24169=DIRECTION('',(0.,0.,-1.));
#24170=DIRECTION('center_axis',(0.,0.707106781186547,-0.707106781186548));
#24171=DIRECTION('ref_axis',(0.,0.707106781186548,0.707106781186547));
#24172=DIRECTION('',(0.,0.707106781186548,0.707106781186547));
#24173=DIRECTION('',(1.,0.,0.));
#24174=DIRECTION('',(0.,-0.707106781186548,-0.707106781186547));
#24175=DIRECTION('center_axis',(0.,0.,-1.));
#24176=DIRECTION('ref_axis',(0.,1.,0.));
#24177=DIRECTION('',(0.,1.,0.));
#24178=DIRECTION('',(1.,0.,0.));
#24179=DIRECTION('',(0.,-1.,0.));
#24180=DIRECTION('center_axis',(0.,-0.707106781186547,-0.707106781186548));
#24181=DIRECTION('ref_axis',(0.,0.707106781186548,-0.707106781186547));
#24182=DIRECTION('',(0.,0.707106781186548,-0.707106781186547));
#24183=DIRECTION('',(1.,0.,0.));
#24184=DIRECTION('',(0.,-0.707106781186548,0.707106781186547));
#24185=DIRECTION('center_axis',(0.,-1.,0.));
#24186=DIRECTION('ref_axis',(0.,0.,-1.));
#24187=DIRECTION('',(0.,0.,-1.));
#24188=DIRECTION('',(1.,0.,0.));
#24189=DIRECTION('',(0.,0.,1.));
#24190=DIRECTION('center_axis',(0.,0.,1.));
#24191=DIRECTION('ref_axis',(0.,-1.,0.));
#24192=DIRECTION('',(0.,-1.,0.));
#24193=DIRECTION('',(1.,0.,0.));
#24194=DIRECTION('',(0.,1.,0.));
#24195=DIRECTION('center_axis',(0.,-1.,0.));
#24196=DIRECTION('ref_axis',(0.,0.,-1.));
#24197=DIRECTION('',(0.,0.,-1.));
#24198=DIRECTION('',(-1.,0.,0.));
#24199=DIRECTION('',(0.,0.,1.));
#24200=DIRECTION('center_axis',(1.,0.,0.));
#24201=DIRECTION('ref_axis',(0.,0.,-1.));
#24202=DIRECTION('center_axis',(1.,0.,0.));
#24203=DIRECTION('ref_axis',(0.,0.,-1.));
#24204=DIRECTION('',(1.,0.,0.));
#24205=DIRECTION('center_axis',(-1.,0.,0.));
#24206=DIRECTION('ref_axis',(0.,0.,-1.));
#24207=DIRECTION('center_axis',(0.,1.,0.));
#24208=DIRECTION('ref_axis',(0.,0.,1.));
#24209=DIRECTION('',(0.,0.,1.));
#24210=DIRECTION('',(1.,0.,0.));
#24211=DIRECTION('',(0.,0.,1.));
#24212=DIRECTION('center_axis',(0.,1.,0.));
#24213=DIRECTION('ref_axis',(0.,0.,1.));
#24214=DIRECTION('',(0.,0.,1.));
#24215=DIRECTION('',(1.,0.,0.));
#24216=DIRECTION('',(0.,0.,1.));
#24217=DIRECTION('center_axis',(0.,0.,-1.));
#24218=DIRECTION('ref_axis',(0.,1.,0.));
#24219=DIRECTION('',(0.,1.,0.));
#24220=DIRECTION('',(0.,1.,0.));
#24221=DIRECTION('center_axis',(0.,0.,-1.));
#24222=DIRECTION('ref_axis',(0.,1.,0.));
#24223=DIRECTION('',(0.,1.,0.));
#24224=DIRECTION('',(1.,0.,0.));
#24225=DIRECTION('',(0.,1.,0.));
#24226=DIRECTION('center_axis',(0.,-1.,0.));
#24227=DIRECTION('ref_axis',(0.,0.,-1.));
#24228=DIRECTION('',(0.,0.,-1.));
#24229=DIRECTION('',(0.,0.,-1.));
#24230=DIRECTION('center_axis',(0.,-1.,0.));
#24231=DIRECTION('ref_axis',(0.,0.,-1.));
#24232=DIRECTION('',(0.,0.,-1.));
#24233=DIRECTION('',(1.,0.,0.));
#24234=DIRECTION('',(0.,0.,-1.));
#24235=DIRECTION('center_axis',(0.,0.,1.));
#24236=DIRECTION('ref_axis',(0.,-1.,0.));
#24237=DIRECTION('',(0.,-1.,0.));
#24238=DIRECTION('',(0.,-1.,0.));
#24239=DIRECTION('center_axis',(0.,0.,1.));
#24240=DIRECTION('ref_axis',(0.,-1.,0.));
#24241=DIRECTION('',(0.,-1.,0.));
#24242=DIRECTION('',(0.,-1.,0.));
#24243=DIRECTION('center_axis',(1.,0.,0.));
#24244=DIRECTION('ref_axis',(0.,0.,-1.));
#24245=DIRECTION('center_axis',(1.,0.,0.));
#24246=DIRECTION('ref_axis',(0.,0.,-1.));
#24247=DIRECTION('axis',(0.,0.,1.));
#24248=DIRECTION('refdir',(1.,0.,0.));
#24249=DIRECTION('center_axis',(0.,1.,0.));
#24250=DIRECTION('ref_axis',(0.,0.,1.));
#24251=DIRECTION('center_axis',(0.,-1.,0.));
#24252=DIRECTION('ref_axis',(1.,0.,0.));
#24253=DIRECTION('center_axis',(0.,-1.,0.));
#24254=DIRECTION('ref_axis',(1.,0.,0.));
#24255=DIRECTION('center_axis',(0.,-1.,0.));
#24256=DIRECTION('ref_axis',(1.,0.,0.));
#24257=DIRECTION('',(0.707106781186548,0.707106781186547,8.65956056235493E-17));
#24258=DIRECTION('center_axis',(0.,-1.,0.));
#24259=DIRECTION('ref_axis',(1.,0.,0.));
#24260=DIRECTION('center_axis',(0.,-1.,0.));
#24261=DIRECTION('ref_axis',(1.,0.,0.));
#24262=DIRECTION('',(0.,1.,0.));
#24263=DIRECTION('center_axis',(0.,1.,0.));
#24264=DIRECTION('ref_axis',(1.,0.,0.));
#24265=DIRECTION('center_axis',(0.,-1.,0.));
#24266=DIRECTION('ref_axis',(1.,0.,0.));
#24267=DIRECTION('',(-0.707106781186547,0.707106781186548,-8.65956056235493E-17));
#24268=DIRECTION('center_axis',(0.,-1.,0.));
#24269=DIRECTION('ref_axis',(0.,0.,-1.));
#24270=DIRECTION('center_axis',(0.,-1.,0.));
#24271=DIRECTION('ref_axis',(1.,0.,0.));
#24272=DIRECTION('center_axis',(0.,1.,0.));
#24273=DIRECTION('ref_axis',(1.,0.,0.));
#24274=DIRECTION('center_axis',(0.,1.,0.));
#24275=DIRECTION('ref_axis',(1.,0.,0.));
#24276=DIRECTION('',(-0.447213595499958,0.894427190999916,-5.47678698264203E-17));
#24277=DIRECTION('center_axis',(0.,-1.,0.));
#24278=DIRECTION('ref_axis',(1.,0.,0.));
#24279=DIRECTION('center_axis',(0.,1.,0.));
#24280=DIRECTION('ref_axis',(1.,0.,0.));
#24281=DIRECTION('',(0.,1.,0.));
#24282=DIRECTION('center_axis',(0.,1.,0.));
#24283=DIRECTION('ref_axis',(1.,0.,0.));
#24284=DIRECTION('center_axis',(0.,-1.,0.));
#24285=DIRECTION('ref_axis',(1.,0.,0.));
#24286=DIRECTION('',(-0.707106781186547,0.707106781186548,-8.65956056235493E-17));
#24287=DIRECTION('center_axis',(0.,-1.,0.));
#24288=DIRECTION('ref_axis',(0.,0.,-1.));
#24289=DIRECTION('center_axis',(0.866025403784439,0.,-0.5));
#24290=DIRECTION('ref_axis',(0.5,0.,0.866025403784439));
#24291=DIRECTION('',(-0.5,0.,-0.866025403784439));
#24292=DIRECTION('',(0.,-1.,0.));
#24293=DIRECTION('',(0.5,0.,0.866025403784439));
#24294=DIRECTION('',(0.,-1.,0.));
#24295=DIRECTION('center_axis',(1.20185167898973E-16,0.,-1.));
#24296=DIRECTION('ref_axis',(1.,0.,1.20185167898973E-16));
#24297=DIRECTION('',(-1.,0.,-1.20185167898973E-16));
#24298=DIRECTION('',(0.,-1.,0.));
#24299=DIRECTION('',(1.,0.,1.20185167898973E-16));
#24300=DIRECTION('center_axis',(-0.866025403784439,0.,-0.5));
#24301=DIRECTION('ref_axis',(0.5,0.,-0.866025403784439));
#24302=DIRECTION('',(-0.5,0.,0.866025403784439));
#24303=DIRECTION('',(0.,-1.,0.));
#24304=DIRECTION('',(0.5,0.,-0.866025403784439));
#24305=DIRECTION('center_axis',(-0.866025403784439,0.,0.5));
#24306=DIRECTION('ref_axis',(-0.5,0.,-0.866025403784439));
#24307=DIRECTION('',(0.5,0.,0.866025403784439));
#24308=DIRECTION('',(0.,-1.,0.));
#24309=DIRECTION('',(-0.5,0.,-0.866025403784439));
#24310=DIRECTION('center_axis',(-2.40370335797945E-16,0.,1.));
#24311=DIRECTION('ref_axis',(-1.,0.,-2.40370335797945E-16));
#24312=DIRECTION('',(1.,0.,2.40370335797945E-16));
#24313=DIRECTION('',(0.,-1.,0.));
#24314=DIRECTION('',(-1.,0.,-2.40370335797945E-16));
#24315=DIRECTION('center_axis',(0.866025403784439,0.,0.5));
#24316=DIRECTION('ref_axis',(-0.5,0.,0.866025403784439));
#24317=DIRECTION('',(0.5,0.,-0.866025403784439));
#24318=DIRECTION('',(-0.5,0.,0.866025403784439));
#24319=DIRECTION('center_axis',(0.,1.,0.));
#24320=DIRECTION('ref_axis',(1.,0.,0.));
#24321=DIRECTION('center_axis',(0.,-1.,0.));
#24322=DIRECTION('ref_axis',(0.,0.,-1.));
#24323=DIRECTION('axis',(0.,0.,1.));
#24324=DIRECTION('refdir',(1.,0.,0.));
#24325=DIRECTION('center_axis',(0.,0.,1.));
#24326=DIRECTION('ref_axis',(1.,0.,0.));
#24327=DIRECTION('',(1.,0.,0.));
#24328=DIRECTION('',(0.,-1.,0.));
#24329=DIRECTION('',(-1.,0.,0.));
#24330=DIRECTION('',(0.,1.,0.));
#24331=DIRECTION('center_axis',(0.,1.,0.));
#24332=DIRECTION('ref_axis',(-1.,0.,0.));
#24333=DIRECTION('',(0.,0.,1.));
#24334=DIRECTION('',(-1.,0.,0.));
#24335=DIRECTION('',(0.,0.,1.));
#24336=DIRECTION('center_axis',(0.,0.,1.));
#24337=DIRECTION('ref_axis',(1.,0.,0.));
#24338=DIRECTION('',(0.,-1.,0.));
#24339=DIRECTION('',(1.,0.,0.));
#24340=DIRECTION('',(0.,1.,0.));
#24341=DIRECTION('center_axis',(0.,0.,-1.));
#24342=DIRECTION('ref_axis',(1.,0.,0.));
#24343=DIRECTION('center_axis',(-1.,0.,0.));
#24344=DIRECTION('ref_axis',(0.,-1.,0.));
#24345=DIRECTION('',(0.,0.,1.));
#24346=DIRECTION('',(0.,0.707106781186548,0.707106781186548));
#24347=DIRECTION('',(0.,-1.,0.));
#24348=DIRECTION('',(0.,0.707106781186548,-0.707106781186548));
#24349=DIRECTION('',(0.,0.,1.));
#24350=DIRECTION('',(0.,-1.,0.));
#24351=DIRECTION('',(0.,0.,1.));
#24352=DIRECTION('center_axis',(0.,-1.,0.));
#24353=DIRECTION('ref_axis',(1.,0.,0.));
#24354=DIRECTION('',(1.,0.,0.));
#24355=DIRECTION('',(0.,0.,1.));
#24356=DIRECTION('center_axis',(0.,0.,1.));
#24357=DIRECTION('ref_axis',(1.,0.,0.));
#24358=DIRECTION('',(-1.,0.,0.));
#24359=DIRECTION('',(0.,1.,0.));
#24360=DIRECTION('center_axis',(1.,0.,0.));
#24361=DIRECTION('ref_axis',(0.,1.,0.));
#24362=DIRECTION('',(0.,0.,1.));
#24363=DIRECTION('',(0.,-0.707106781186548,0.707106781186548));
#24364=DIRECTION('',(0.,1.,0.));
#24365=DIRECTION('',(0.,-0.707106781186548,-0.707106781186548));
#24366=DIRECTION('',(0.,0.,1.));
#24367=DIRECTION('center_axis',(0.,-1.,0.));
#24368=DIRECTION('ref_axis',(1.,0.,0.));
#24369=DIRECTION('',(-1.,0.,0.));
#24370=DIRECTION('center_axis',(0.,-0.707106781186548,-0.707106781186548));
#24371=DIRECTION('ref_axis',(-1.,0.,0.));
#24372=DIRECTION('',(1.,0.,0.));
#24373=DIRECTION('center_axis',(0.,0.707106781186548,0.707106781186548));
#24374=DIRECTION('ref_axis',(0.,0.707106781186547,-0.707106781186547));
#24375=DIRECTION('',(1.,0.,0.));
#24376=DIRECTION('center_axis',(0.,0.,1.));
#24377=DIRECTION('ref_axis',(1.,0.,0.));
#24378=DIRECTION('center_axis',(0.,0.,-1.));
#24379=DIRECTION('ref_axis',(1.,0.,0.));
#24380=DIRECTION('',(0.,0.,1.));
#24381=DIRECTION('center_axis',(0.,0.,-1.));
#24382=DIRECTION('ref_axis',(1.,0.,0.));
#24383=DIRECTION('center_axis',(0.,-0.707106781186548,0.707106781186548));
#24384=DIRECTION('ref_axis',(0.,0.707106781186547,0.707106781186547));
#24385=DIRECTION('center_axis',(0.,0.,-1.));
#24386=DIRECTION('ref_axis',(1.,0.,0.));
#24387=DIRECTION('center_axis',(0.,0.,1.));
#24388=DIRECTION('ref_axis',(1.,0.,0.));
#24389=DIRECTION('',(-1.,0.,0.));
#24390=DIRECTION('center_axis',(0.,0.,1.));
#24391=DIRECTION('ref_axis',(1.,0.,0.));
#24392=DIRECTION('',(-1.,0.,0.));
#24393=DIRECTION('center_axis',(0.,0.707106781186548,-0.707106781186548));
#24394=DIRECTION('ref_axis',(-1.,0.,0.));
#24395=DIRECTION('',(1.,0.,0.));
#24396=DIRECTION('center_axis',(0.,1.,0.));
#24397=DIRECTION('ref_axis',(-1.,0.,0.));
#24398=DIRECTION('axis',(0.,0.,1.));
#24399=DIRECTION('refdir',(1.,0.,0.));
#24400=DIRECTION('center_axis',(0.,1.,0.));
#24401=DIRECTION('ref_axis',(1.,0.,0.));
#24402=DIRECTION('center_axis',(0.,1.,0.));
#24403=DIRECTION('ref_axis',(1.,0.,0.));
#24404=DIRECTION('',(0.5,0.,0.866025403784439));
#24405=DIRECTION('',(1.,0.,1.20185167898973E-16));
#24406=DIRECTION('',(0.5,0.,-0.866025403784439));
#24407=DIRECTION('',(-0.5,0.,-0.866025403784439));
#24408=DIRECTION('',(-1.,0.,-2.40370335797945E-16));
#24409=DIRECTION('',(-0.5,0.,0.866025403784439));
#24410=DIRECTION('center_axis',(0.,1.,0.));
#24411=DIRECTION('ref_axis',(0.,0.,1.));
#24412=DIRECTION('center_axis',(0.,-1.,0.));
#24413=DIRECTION('ref_axis',(1.,0.,0.));
#24414=DIRECTION('center_axis',(0.,-1.,0.));
#24415=DIRECTION('ref_axis',(1.,0.,0.));
#24416=DIRECTION('center_axis',(0.,-1.,0.));
#24417=DIRECTION('ref_axis',(1.,0.,0.));
#24418=DIRECTION('',(0.707106781186548,0.707106781186547,8.65956056235493E-17));
#24419=DIRECTION('center_axis',(0.,-1.,0.));
#24420=DIRECTION('ref_axis',(1.,0.,0.));
#24421=DIRECTION('center_axis',(0.,-1.,0.));
#24422=DIRECTION('ref_axis',(1.,0.,0.));
#24423=DIRECTION('',(0.,1.,0.));
#24424=DIRECTION('center_axis',(0.,1.,0.));
#24425=DIRECTION('ref_axis',(1.,0.,0.));
#24426=DIRECTION('center_axis',(0.,-1.,0.));
#24427=DIRECTION('ref_axis',(1.,0.,0.));
#24428=DIRECTION('',(-0.707106781186547,0.707106781186548,-8.65956056235493E-17));
#24429=DIRECTION('center_axis',(0.,-1.,0.));
#24430=DIRECTION('ref_axis',(0.,0.,-1.));
#24431=DIRECTION('center_axis',(0.,-1.,0.));
#24432=DIRECTION('ref_axis',(1.,0.,0.));
#24433=DIRECTION('center_axis',(0.,1.,0.));
#24434=DIRECTION('ref_axis',(1.,0.,0.));
#24435=DIRECTION('center_axis',(0.,1.,0.));
#24436=DIRECTION('ref_axis',(1.,0.,0.));
#24437=DIRECTION('',(-0.447213595499958,0.894427190999916,-5.47678698264203E-17));
#24438=DIRECTION('center_axis',(0.,-1.,0.));
#24439=DIRECTION('ref_axis',(1.,0.,0.));
#24440=DIRECTION('',(0.,1.,0.));
#24441=DIRECTION('center_axis',(0.866025403784439,0.,-0.5));
#24442=DIRECTION('ref_axis',(0.5,0.,0.866025403784439));
#24443=DIRECTION('',(-0.5,0.,-0.866025403784439));
#24444=DIRECTION('',(0.,-1.,0.));
#24445=DIRECTION('',(0.,-1.,0.));
#24446=DIRECTION('center_axis',(1.20185167898973E-16,0.,-1.));
#24447=DIRECTION('ref_axis',(1.,0.,1.20185167898973E-16));
#24448=DIRECTION('',(-1.,0.,-1.20185167898973E-16));
#24449=DIRECTION('',(0.,-1.,0.));
#24450=DIRECTION('center_axis',(-0.866025403784439,0.,-0.5));
#24451=DIRECTION('ref_axis',(0.5,0.,-0.866025403784439));
#24452=DIRECTION('',(-0.5,0.,0.866025403784439));
#24453=DIRECTION('',(0.,-1.,0.));
#24454=DIRECTION('center_axis',(-0.866025403784439,0.,0.5));
#24455=DIRECTION('ref_axis',(-0.5,0.,-0.866025403784439));
#24456=DIRECTION('',(0.5,0.,0.866025403784439));
#24457=DIRECTION('',(0.,-1.,0.));
#24458=DIRECTION('center_axis',(-2.40370335797945E-16,0.,1.));
#24459=DIRECTION('ref_axis',(-1.,0.,-2.40370335797945E-16));
#24460=DIRECTION('',(1.,0.,2.40370335797945E-16));
#24461=DIRECTION('',(0.,-1.,0.));
#24462=DIRECTION('center_axis',(0.866025403784439,0.,0.5));
#24463=DIRECTION('ref_axis',(-0.5,0.,0.866025403784439));
#24464=DIRECTION('',(0.5,0.,-0.866025403784439));
#24465=DIRECTION('center_axis',(0.,1.,0.));
#24466=DIRECTION('ref_axis',(1.,0.,0.));
#24467=DIRECTION('axis',(0.,0.,1.));
#24468=DIRECTION('refdir',(1.,0.,0.));
#24469=DIRECTION('axis',(0.,0.,1.));
#24470=DIRECTION('refdir',(1.,0.,0.));
#24471=DIRECTION('center_axis',(0.,0.,1.));
#24472=DIRECTION('ref_axis',(1.,0.,0.));
#24473=DIRECTION('center_axis',(0.,0.,1.));
#24474=DIRECTION('ref_axis',(1.,0.,0.));
#24475=DIRECTION('',(0.,0.,1.));
#24476=DIRECTION('center_axis',(0.,0.,-1.));
#24477=DIRECTION('ref_axis',(1.,0.,0.));
#24478=DIRECTION('center_axis',(0.,0.,1.));
#24479=DIRECTION('ref_axis',(1.,0.,0.));
#24480=DIRECTION('center_axis',(0.,0.,1.));
#24481=DIRECTION('ref_axis',(1.,0.,0.));
#24482=DIRECTION('',(0.,0.,1.));
#24483=DIRECTION('center_axis',(0.,0.,-1.));
#24484=DIRECTION('ref_axis',(1.,0.,0.));
#24485=DIRECTION('center_axis',(0.,0.,1.));
#24486=DIRECTION('ref_axis',(1.,0.,0.));
#24487=DIRECTION('center_axis',(0.,0.,1.));
#24488=DIRECTION('ref_axis',(1.,0.,0.));
#24489=DIRECTION('',(0.,0.,1.));
#24490=DIRECTION('center_axis',(0.,0.,-1.));
#24491=DIRECTION('ref_axis',(1.,0.,0.));
#24492=DIRECTION('center_axis',(0.,0.,1.));
#24493=DIRECTION('ref_axis',(1.,0.,0.));
#24494=DIRECTION('center_axis',(0.,0.,1.));
#24495=DIRECTION('ref_axis',(1.,0.,0.));
#24496=DIRECTION('',(0.,0.,1.));
#24497=DIRECTION('center_axis',(0.,0.,-1.));
#24498=DIRECTION('ref_axis',(1.,0.,0.));
#24499=DIRECTION('center_axis',(0.,0.,1.));
#24500=DIRECTION('ref_axis',(1.,0.,0.));
#24501=DIRECTION('center_axis',(0.,0.,1.));
#24502=DIRECTION('ref_axis',(1.,0.,0.));
#24503=DIRECTION('',(0.,0.,1.));
#24504=DIRECTION('center_axis',(0.,0.,-1.));
#24505=DIRECTION('ref_axis',(1.,0.,0.));
#24506=DIRECTION('center_axis',(0.,0.,1.));
#24507=DIRECTION('ref_axis',(1.,0.,0.));
#24508=DIRECTION('center_axis',(0.,0.,1.));
#24509=DIRECTION('ref_axis',(1.,0.,0.));
#24510=DIRECTION('',(0.,0.,1.));
#24511=DIRECTION('center_axis',(0.,0.,-1.));
#24512=DIRECTION('ref_axis',(1.,0.,0.));
#24513=DIRECTION('center_axis',(0.,0.,1.));
#24514=DIRECTION('ref_axis',(1.,0.,0.));
#24515=DIRECTION('center_axis',(0.,0.,1.));
#24516=DIRECTION('ref_axis',(1.,0.,0.));
#24517=DIRECTION('',(0.,0.,1.));
#24518=DIRECTION('center_axis',(0.,0.,-1.));
#24519=DIRECTION('ref_axis',(1.,0.,0.));
#24520=DIRECTION('center_axis',(0.,0.,1.));
#24521=DIRECTION('ref_axis',(1.,0.,0.));
#24522=DIRECTION('center_axis',(0.,0.,1.));
#24523=DIRECTION('ref_axis',(1.,0.,0.));
#24524=DIRECTION('',(0.,0.,1.));
#24525=DIRECTION('center_axis',(0.,0.,-1.));
#24526=DIRECTION('ref_axis',(1.,0.,0.));
#24527=DIRECTION('center_axis',(0.,0.,1.));
#24528=DIRECTION('ref_axis',(1.,0.,0.));
#24529=DIRECTION('center_axis',(0.,0.,1.));
#24530=DIRECTION('ref_axis',(1.,0.,0.));
#24531=DIRECTION('',(0.,0.,1.));
#24532=DIRECTION('center_axis',(0.,0.,-1.));
#24533=DIRECTION('ref_axis',(1.,0.,0.));
#24534=DIRECTION('center_axis',(0.,0.,1.));
#24535=DIRECTION('ref_axis',(1.,0.,0.));
#24536=DIRECTION('center_axis',(0.,0.,1.));
#24537=DIRECTION('ref_axis',(1.,0.,0.));
#24538=DIRECTION('',(0.,0.,1.));
#24539=DIRECTION('center_axis',(0.,0.,-1.));
#24540=DIRECTION('ref_axis',(1.,0.,0.));
#24541=DIRECTION('center_axis',(0.,0.,1.));
#24542=DIRECTION('ref_axis',(1.,0.,0.));
#24543=DIRECTION('center_axis',(0.,0.,1.));
#24544=DIRECTION('ref_axis',(1.,0.,0.));
#24545=DIRECTION('',(0.,0.,1.));
#24546=DIRECTION('center_axis',(0.,0.,-1.));
#24547=DIRECTION('ref_axis',(1.,0.,0.));
#24548=DIRECTION('center_axis',(0.,0.,1.));
#24549=DIRECTION('ref_axis',(1.,0.,0.));
#24550=DIRECTION('center_axis',(0.,0.,1.));
#24551=DIRECTION('ref_axis',(1.,0.,0.));
#24552=DIRECTION('',(0.,0.,1.));
#24553=DIRECTION('center_axis',(0.,0.,-1.));
#24554=DIRECTION('ref_axis',(1.,0.,0.));
#24555=DIRECTION('center_axis',(0.,0.,1.));
#24556=DIRECTION('ref_axis',(1.,0.,0.));
#24557=DIRECTION('center_axis',(0.,0.,1.));
#24558=DIRECTION('ref_axis',(1.,0.,0.));
#24559=DIRECTION('',(0.,0.,1.));
#24560=DIRECTION('center_axis',(0.,0.,-1.));
#24561=DIRECTION('ref_axis',(1.,0.,0.));
#24562=DIRECTION('center_axis',(0.,0.,1.));
#24563=DIRECTION('ref_axis',(1.,0.,0.));
#24564=DIRECTION('center_axis',(0.,0.,1.));
#24565=DIRECTION('ref_axis',(1.,0.,0.));
#24566=DIRECTION('',(0.,0.,1.));
#24567=DIRECTION('center_axis',(0.,0.,-1.));
#24568=DIRECTION('ref_axis',(1.,0.,0.));
#24569=DIRECTION('center_axis',(0.,0.,1.));
#24570=DIRECTION('ref_axis',(1.,0.,0.));
#24571=DIRECTION('center_axis',(0.,0.,1.));
#24572=DIRECTION('ref_axis',(1.,0.,0.));
#24573=DIRECTION('',(0.,0.,1.));
#24574=DIRECTION('center_axis',(0.,0.,-1.));
#24575=DIRECTION('ref_axis',(1.,0.,0.));
#24576=DIRECTION('center_axis',(0.,0.,1.));
#24577=DIRECTION('ref_axis',(1.,0.,0.));
#24578=DIRECTION('center_axis',(0.,0.,1.));
#24579=DIRECTION('ref_axis',(1.,0.,0.));
#24580=DIRECTION('',(0.,0.,1.));
#24581=DIRECTION('center_axis',(0.,0.,-1.));
#24582=DIRECTION('ref_axis',(1.,0.,0.));
#24583=DIRECTION('center_axis',(0.,0.,1.));
#24584=DIRECTION('ref_axis',(1.,0.,0.));
#24585=DIRECTION('center_axis',(0.,0.,1.));
#24586=DIRECTION('ref_axis',(1.,0.,0.));
#24587=DIRECTION('',(0.,0.,1.));
#24588=DIRECTION('center_axis',(0.,0.,-1.));
#24589=DIRECTION('ref_axis',(1.,0.,0.));
#24590=DIRECTION('center_axis',(0.,0.,1.));
#24591=DIRECTION('ref_axis',(1.,0.,0.));
#24592=DIRECTION('center_axis',(0.,0.,1.));
#24593=DIRECTION('ref_axis',(1.,0.,0.));
#24594=DIRECTION('',(0.,0.,1.));
#24595=DIRECTION('center_axis',(0.,0.,-1.));
#24596=DIRECTION('ref_axis',(1.,0.,0.));
#24597=DIRECTION('center_axis',(0.,1.,0.));
#24598=DIRECTION('ref_axis',(-1.,0.,0.));
#24599=DIRECTION('',(-1.,0.,0.));
#24600=DIRECTION('',(0.,0.,1.));
#24601=DIRECTION('',(-1.,0.,0.));
#24602=DIRECTION('',(0.,0.,1.));
#24603=DIRECTION('center_axis',(1.,0.,0.));
#24604=DIRECTION('ref_axis',(0.,1.,0.));
#24605=DIRECTION('',(0.,1.,0.));
#24606=DIRECTION('',(0.,1.,0.));
#24607=DIRECTION('',(0.,0.,1.));
#24608=DIRECTION('center_axis',(0.,-1.,0.));
#24609=DIRECTION('ref_axis',(1.,0.,0.));
#24610=DIRECTION('',(1.,0.,0.));
#24611=DIRECTION('',(1.,0.,0.));
#24612=DIRECTION('',(0.,0.,1.));
#24613=DIRECTION('center_axis',(-1.,0.,0.));
#24614=DIRECTION('ref_axis',(0.,-1.,0.));
#24615=DIRECTION('',(0.,-1.,0.));
#24616=DIRECTION('',(0.,-1.,0.));
#24617=DIRECTION('center_axis',(0.,0.,1.));
#24618=DIRECTION('ref_axis',(1.,0.,0.));
#24619=DIRECTION('center_axis',(0.,0.,1.));
#24620=DIRECTION('ref_axis',(1.,0.,0.));
#24621=DIRECTION('axis',(0.,0.,1.));
#24622=DIRECTION('refdir',(1.,0.,0.));
#24623=DIRECTION('center_axis',(0.,0.,1.));
#24624=DIRECTION('ref_axis',(1.,0.,0.));
#24625=DIRECTION('center_axis',(0.,0.,-1.));
#24626=DIRECTION('ref_axis',(1.,0.,0.));
#24627=DIRECTION('center_axis',(0.,0.,1.));
#24628=DIRECTION('ref_axis',(1.,0.,0.));
#24629=DIRECTION('center_axis',(0.,0.,1.));
#24630=DIRECTION('ref_axis',(1.,0.,0.));
#24631=DIRECTION('',(0.,0.,-1.));
#24632=DIRECTION('center_axis',(0.,0.,1.));
#24633=DIRECTION('ref_axis',(1.,0.,0.));
#24634=DIRECTION('',(0.,0.,1.));
#24635=DIRECTION('center_axis',(0.,0.,-1.));
#24636=DIRECTION('ref_axis',(1.,0.,0.));
#24637=DIRECTION('center_axis',(0.,0.,1.));
#24638=DIRECTION('ref_axis',(1.,0.,0.));
#24639=DIRECTION('',(0.,0.,1.));
#24640=DIRECTION('center_axis',(0.,0.,1.));
#24641=DIRECTION('ref_axis',(1.,0.,0.));
#24642=DIRECTION('center_axis',(0.,0.,-1.));
#24643=DIRECTION('ref_axis',(1.,0.,0.));
#24644=DIRECTION('center_axis',(0.,0.,1.));
#24645=DIRECTION('ref_axis',(1.,0.,0.));
#24646=DIRECTION('center_axis',(0.,0.,1.));
#24647=DIRECTION('ref_axis',(1.,0.,0.));
#24648=DIRECTION('',(0.,0.,-1.));
#24649=DIRECTION('center_axis',(0.,0.,1.));
#24650=DIRECTION('ref_axis',(1.,0.,0.));
#24651=DIRECTION('',(0.,0.,1.));
#24652=DIRECTION('center_axis',(0.,0.,-1.));
#24653=DIRECTION('ref_axis',(1.,0.,0.));
#24654=DIRECTION('center_axis',(0.,0.,1.));
#24655=DIRECTION('ref_axis',(1.,0.,0.));
#24656=DIRECTION('',(0.,0.,1.));
#24657=DIRECTION('center_axis',(0.,0.,1.));
#24658=DIRECTION('ref_axis',(1.,0.,0.));
#24659=DIRECTION('center_axis',(0.,0.,-1.));
#24660=DIRECTION('ref_axis',(1.,0.,0.));
#24661=DIRECTION('center_axis',(0.,0.,1.));
#24662=DIRECTION('ref_axis',(1.,0.,0.));
#24663=DIRECTION('center_axis',(0.,0.,1.));
#24664=DIRECTION('ref_axis',(1.,0.,0.));
#24665=DIRECTION('center_axis',(0.,0.,1.));
#24666=DIRECTION('ref_axis',(1.,0.,0.));
#24667=DIRECTION('',(0.,0.,-1.));
#24668=DIRECTION('center_axis',(0.,0.,1.));
#24669=DIRECTION('ref_axis',(1.,0.,0.));
#24670=DIRECTION('',(0.,0.,1.));
#24671=DIRECTION('',(0.,0.,1.));
#24672=DIRECTION('center_axis',(0.,0.,-1.));
#24673=DIRECTION('ref_axis',(1.,0.,0.));
#24674=DIRECTION('center_axis',(0.,0.,1.));
#24675=DIRECTION('ref_axis',(1.,0.,0.));
#24676=DIRECTION('center_axis',(0.,0.,-1.));
#24677=DIRECTION('ref_axis',(1.,0.,0.));
#24678=DIRECTION('center_axis',(0.,0.,1.));
#24679=DIRECTION('ref_axis',(1.,0.,0.));
#24680=DIRECTION('center_axis',(0.,0.,1.));
#24681=DIRECTION('ref_axis',(1.,0.,0.));
#24682=DIRECTION('center_axis',(0.,0.,1.));
#24683=DIRECTION('ref_axis',(1.,0.,0.));
#24684=DIRECTION('',(0.,0.,-1.));
#24685=DIRECTION('center_axis',(0.,0.,1.));
#24686=DIRECTION('ref_axis',(1.,0.,0.));
#24687=DIRECTION('',(0.,0.,1.));
#24688=DIRECTION('',(0.,0.,1.));
#24689=DIRECTION('center_axis',(0.,0.,-1.));
#24690=DIRECTION('ref_axis',(1.,0.,0.));
#24691=DIRECTION('center_axis',(0.,0.,1.));
#24692=DIRECTION('ref_axis',(1.,0.,0.));
#24693=DIRECTION('center_axis',(0.,0.,-1.));
#24694=DIRECTION('ref_axis',(1.,0.,0.));
#24695=DIRECTION('',(0.,0.,-1.));
#24696=DIRECTION('center_axis',(0.,0.,1.));
#24697=DIRECTION('ref_axis',(1.,0.,0.));
#24698=DIRECTION('center_axis',(0.,0.,-1.));
#24699=DIRECTION('ref_axis',(1.,0.,0.));
#24700=DIRECTION('center_axis',(0.,0.,-1.));
#24701=DIRECTION('ref_axis',(1.,0.,0.));
#24702=DIRECTION('center_axis',(0.,0.,-1.));
#24703=DIRECTION('ref_axis',(1.,0.,0.));
#24704=DIRECTION('center_axis',(0.,0.,-1.));
#24705=DIRECTION('ref_axis',(1.,0.,0.));
#24706=DIRECTION('center_axis',(0.,0.,1.));
#24707=DIRECTION('ref_axis',(1.,0.,0.));
#24708=DIRECTION('center_axis',(0.,0.,1.));
#24709=DIRECTION('ref_axis',(1.,0.,0.));
#24710=DIRECTION('',(0.,0.,1.));
#24711=DIRECTION('center_axis',(0.,0.,-1.));
#24712=DIRECTION('ref_axis',(1.,0.,0.));
#24713=DIRECTION('center_axis',(0.,0.,1.));
#24714=DIRECTION('ref_axis',(1.,0.,0.));
#24715=DIRECTION('center_axis',(0.,0.,1.));
#24716=DIRECTION('ref_axis',(1.,0.,0.));
#24717=DIRECTION('center_axis',(0.,0.,1.));
#24718=DIRECTION('ref_axis',(1.,0.,0.));
#24719=DIRECTION('center_axis',(0.,0.,1.));
#24720=DIRECTION('ref_axis',(1.,0.,0.));
#24721=DIRECTION('center_axis',(0.,0.,1.));
#24722=DIRECTION('ref_axis',(1.,0.,0.));
#24723=DIRECTION('center_axis',(0.,0.,1.));
#24724=DIRECTION('ref_axis',(1.,0.,0.));
#24725=DIRECTION('',(0.,0.,-1.));
#24726=DIRECTION('center_axis',(0.,0.,1.));
#24727=DIRECTION('ref_axis',(1.,0.,0.));
#24728=DIRECTION('',(0.,0.,-1.));
#24729=DIRECTION('center_axis',(0.,0.,-1.));
#24730=DIRECTION('ref_axis',(1.,0.,0.));
#24731=DIRECTION('center_axis',(0.,0.,1.));
#24732=DIRECTION('ref_axis',(1.,0.,0.));
#24733=DIRECTION('center_axis',(0.,0.,1.));
#24734=DIRECTION('ref_axis',(1.,0.,0.));
#24735=DIRECTION('axis',(0.,0.,1.));
#24736=DIRECTION('refdir',(1.,0.,0.));
#24737=DIRECTION('center_axis',(0.,0.,1.));
#24738=DIRECTION('ref_axis',(1.,0.,0.));
#24739=DIRECTION('center_axis',(0.,0.,-1.));
#24740=DIRECTION('ref_axis',(1.,0.,0.));
#24741=DIRECTION('center_axis',(0.,0.,1.));
#24742=DIRECTION('ref_axis',(1.,0.,0.));
#24743=DIRECTION('center_axis',(0.,0.,1.));
#24744=DIRECTION('ref_axis',(1.,0.,0.));
#24745=DIRECTION('',(0.,0.,-1.));
#24746=DIRECTION('center_axis',(0.,0.,1.));
#24747=DIRECTION('ref_axis',(1.,0.,0.));
#24748=DIRECTION('',(0.,0.,1.));
#24749=DIRECTION('center_axis',(0.,0.,-1.));
#24750=DIRECTION('ref_axis',(1.,0.,0.));
#24751=DIRECTION('center_axis',(0.,0.,1.));
#24752=DIRECTION('ref_axis',(1.,0.,0.));
#24753=DIRECTION('',(0.,0.,1.));
#24754=DIRECTION('center_axis',(0.,0.,1.));
#24755=DIRECTION('ref_axis',(1.,0.,0.));
#24756=DIRECTION('center_axis',(0.,0.,-1.));
#24757=DIRECTION('ref_axis',(1.,0.,0.));
#24758=DIRECTION('center_axis',(0.,0.,1.));
#24759=DIRECTION('ref_axis',(1.,0.,0.));
#24760=DIRECTION('center_axis',(0.,0.,1.));
#24761=DIRECTION('ref_axis',(1.,0.,0.));
#24762=DIRECTION('',(0.,0.,-1.));
#24763=DIRECTION('center_axis',(0.,0.,1.));
#24764=DIRECTION('ref_axis',(1.,0.,0.));
#24765=DIRECTION('',(0.,0.,1.));
#24766=DIRECTION('center_axis',(0.,0.,-1.));
#24767=DIRECTION('ref_axis',(1.,0.,0.));
#24768=DIRECTION('center_axis',(0.,0.,1.));
#24769=DIRECTION('ref_axis',(1.,0.,0.));
#24770=DIRECTION('',(0.,0.,1.));
#24771=DIRECTION('center_axis',(0.,0.,1.));
#24772=DIRECTION('ref_axis',(1.,0.,0.));
#24773=DIRECTION('center_axis',(0.,0.,-1.));
#24774=DIRECTION('ref_axis',(1.,0.,0.));
#24775=DIRECTION('center_axis',(0.,0.,1.));
#24776=DIRECTION('ref_axis',(1.,0.,0.));
#24777=DIRECTION('center_axis',(0.,0.,1.));
#24778=DIRECTION('ref_axis',(1.,0.,0.));
#24779=DIRECTION('center_axis',(0.,0.,1.));
#24780=DIRECTION('ref_axis',(1.,0.,0.));
#24781=DIRECTION('',(0.,0.,-1.));
#24782=DIRECTION('center_axis',(0.,0.,1.));
#24783=DIRECTION('ref_axis',(1.,0.,0.));
#24784=DIRECTION('',(0.,0.,1.));
#24785=DIRECTION('',(0.,0.,1.));
#24786=DIRECTION('center_axis',(0.,0.,-1.));
#24787=DIRECTION('ref_axis',(1.,0.,0.));
#24788=DIRECTION('center_axis',(0.,0.,1.));
#24789=DIRECTION('ref_axis',(1.,0.,0.));
#24790=DIRECTION('center_axis',(0.,0.,-1.));
#24791=DIRECTION('ref_axis',(1.,0.,0.));
#24792=DIRECTION('center_axis',(0.,0.,1.));
#24793=DIRECTION('ref_axis',(1.,0.,0.));
#24794=DIRECTION('center_axis',(0.,0.,1.));
#24795=DIRECTION('ref_axis',(1.,0.,0.));
#24796=DIRECTION('center_axis',(0.,0.,1.));
#24797=DIRECTION('ref_axis',(1.,0.,0.));
#24798=DIRECTION('',(0.,0.,-1.));
#24799=DIRECTION('center_axis',(0.,0.,1.));
#24800=DIRECTION('ref_axis',(1.,0.,0.));
#24801=DIRECTION('',(0.,0.,1.));
#24802=DIRECTION('',(0.,0.,1.));
#24803=DIRECTION('center_axis',(0.,0.,-1.));
#24804=DIRECTION('ref_axis',(1.,0.,0.));
#24805=DIRECTION('center_axis',(0.,0.,1.));
#24806=DIRECTION('ref_axis',(1.,0.,0.));
#24807=DIRECTION('center_axis',(0.,0.,-1.));
#24808=DIRECTION('ref_axis',(1.,0.,0.));
#24809=DIRECTION('',(0.,0.,-1.));
#24810=DIRECTION('center_axis',(0.,0.,1.));
#24811=DIRECTION('ref_axis',(1.,0.,0.));
#24812=DIRECTION('center_axis',(0.,0.,-1.));
#24813=DIRECTION('ref_axis',(1.,0.,0.));
#24814=DIRECTION('center_axis',(0.,0.,-1.));
#24815=DIRECTION('ref_axis',(1.,0.,0.));
#24816=DIRECTION('center_axis',(0.,0.,-1.));
#24817=DIRECTION('ref_axis',(1.,0.,0.));
#24818=DIRECTION('center_axis',(0.,0.,-1.));
#24819=DIRECTION('ref_axis',(1.,0.,0.));
#24820=DIRECTION('center_axis',(0.,0.,1.));
#24821=DIRECTION('ref_axis',(1.,0.,0.));
#24822=DIRECTION('center_axis',(0.,0.,1.));
#24823=DIRECTION('ref_axis',(1.,0.,0.));
#24824=DIRECTION('',(0.,0.,1.));
#24825=DIRECTION('center_axis',(0.,0.,-1.));
#24826=DIRECTION('ref_axis',(1.,0.,0.));
#24827=DIRECTION('center_axis',(0.,0.,1.));
#24828=DIRECTION('ref_axis',(1.,0.,0.));
#24829=DIRECTION('center_axis',(0.,0.,1.));
#24830=DIRECTION('ref_axis',(1.,0.,0.));
#24831=DIRECTION('center_axis',(0.,0.,1.));
#24832=DIRECTION('ref_axis',(1.,0.,0.));
#24833=DIRECTION('center_axis',(0.,0.,1.));
#24834=DIRECTION('ref_axis',(1.,0.,0.));
#24835=DIRECTION('center_axis',(0.,0.,1.));
#24836=DIRECTION('ref_axis',(1.,0.,0.));
#24837=DIRECTION('center_axis',(0.,0.,1.));
#24838=DIRECTION('ref_axis',(1.,0.,0.));
#24839=DIRECTION('',(0.,0.,-1.));
#24840=DIRECTION('center_axis',(0.,0.,1.));
#24841=DIRECTION('ref_axis',(1.,0.,0.));
#24842=DIRECTION('',(0.,0.,-1.));
#24843=DIRECTION('center_axis',(0.,0.,-1.));
#24844=DIRECTION('ref_axis',(1.,0.,0.));
#24845=DIRECTION('center_axis',(0.,0.,1.));
#24846=DIRECTION('ref_axis',(1.,0.,0.));
#24847=DIRECTION('center_axis',(0.,0.,1.));
#24848=DIRECTION('ref_axis',(1.,0.,0.));
#24849=DIRECTION('axis',(0.,0.,1.));
#24850=DIRECTION('refdir',(1.,0.,0.));
#24851=DIRECTION('center_axis',(0.,0.,1.));
#24852=DIRECTION('ref_axis',(1.,0.,0.));
#24853=DIRECTION('center_axis',(0.,0.,1.));
#24854=DIRECTION('ref_axis',(1.,0.,0.));
#24855=DIRECTION('',(0.,0.,1.));
#24856=DIRECTION('center_axis',(0.,0.,-1.));
#24857=DIRECTION('ref_axis',(1.,0.,0.));
#24858=DIRECTION('center_axis',(0.,0.,1.));
#24859=DIRECTION('ref_axis',(1.,0.,0.));
#24860=DIRECTION('center_axis',(0.,0.,1.));
#24861=DIRECTION('ref_axis',(1.,0.,0.));
#24862=DIRECTION('center_axis',(0.,0.,1.));
#24863=DIRECTION('ref_axis',(1.,0.,0.));
#24864=DIRECTION('',(0.,0.,1.));
#24865=DIRECTION('center_axis',(0.,0.,-1.));
#24866=DIRECTION('ref_axis',(1.,0.,0.));
#24867=DIRECTION('center_axis',(0.,0.,1.));
#24868=DIRECTION('ref_axis',(1.,0.,0.));
#24869=DIRECTION('center_axis',(0.,0.,1.));
#24870=DIRECTION('ref_axis',(1.,0.,0.));
#24871=DIRECTION('center_axis',(0.,0.,1.));
#24872=DIRECTION('ref_axis',(1.,0.,0.));
#24873=DIRECTION('',(0.,0.,1.));
#24874=DIRECTION('center_axis',(0.,0.,-1.));
#24875=DIRECTION('ref_axis',(1.,0.,0.));
#24876=DIRECTION('center_axis',(0.,0.,1.));
#24877=DIRECTION('ref_axis',(1.,0.,0.));
#24878=DIRECTION('center_axis',(0.,0.,1.));
#24879=DIRECTION('ref_axis',(1.,0.,0.));
#24880=DIRECTION('center_axis',(0.,0.,-1.));
#24881=DIRECTION('ref_axis',(1.,0.,0.));
#24882=DIRECTION('',(0.,0.,-1.));
#24883=DIRECTION('center_axis',(0.,0.,-1.));
#24884=DIRECTION('ref_axis',(1.,0.,0.));
#24885=DIRECTION('center_axis',(0.,0.,1.));
#24886=DIRECTION('ref_axis',(1.,0.,0.));
#24887=DIRECTION('center_axis',(0.,0.,1.));
#24888=DIRECTION('ref_axis',(1.,0.,0.));
#24889=DIRECTION('',(0.,0.,-1.));
#24890=DIRECTION('center_axis',(0.,0.,1.));
#24891=DIRECTION('ref_axis',(1.,0.,0.));
#24892=DIRECTION('center_axis',(0.,0.,1.));
#24893=DIRECTION('ref_axis',(1.,0.,0.));
#24894=DIRECTION('center_axis',(0.,0.,1.));
#24895=DIRECTION('ref_axis',(1.,0.,0.));
#24896=DIRECTION('axis',(0.,0.,1.));
#24897=DIRECTION('refdir',(1.,0.,0.));
#24898=DIRECTION('center_axis',(0.,0.,1.));
#24899=DIRECTION('ref_axis',(1.,0.,0.));
#24900=DIRECTION('center_axis',(0.,0.,1.));
#24901=DIRECTION('ref_axis',(1.,0.,0.));
#24902=DIRECTION('',(0.,0.,1.));
#24903=DIRECTION('center_axis',(0.,0.,-1.));
#24904=DIRECTION('ref_axis',(1.,0.,0.));
#24905=DIRECTION('center_axis',(0.,0.,1.));
#24906=DIRECTION('ref_axis',(1.,0.,0.));
#24907=DIRECTION('center_axis',(0.,0.,1.));
#24908=DIRECTION('ref_axis',(1.,0.,0.));
#24909=DIRECTION('',(0.,0.,1.));
#24910=DIRECTION('center_axis',(0.,0.,-1.));
#24911=DIRECTION('ref_axis',(1.,0.,0.));
#24912=DIRECTION('center_axis',(0.,0.,1.));
#24913=DIRECTION('ref_axis',(1.,0.,0.));
#24914=DIRECTION('center_axis',(0.,0.,1.));
#24915=DIRECTION('ref_axis',(1.,0.,0.));
#24916=DIRECTION('',(0.,0.,-1.));
#24917=DIRECTION('center_axis',(0.,0.,1.));
#24918=DIRECTION('ref_axis',(1.,0.,0.));
#24919=DIRECTION('center_axis',(0.,0.,1.));
#24920=DIRECTION('ref_axis',(1.,0.,0.));
#24921=DIRECTION('center_axis',(0.,0.,1.));
#24922=DIRECTION('ref_axis',(1.,0.,0.));
#24923=DIRECTION('axis',(0.,0.,1.));
#24924=DIRECTION('refdir',(1.,0.,0.));
#24925=DIRECTION('center_axis',(0.,0.,1.));
#24926=DIRECTION('ref_axis',(1.,0.,0.));
#24927=DIRECTION('center_axis',(0.,0.,1.));
#24928=DIRECTION('ref_axis',(1.,0.,0.));
#24929=DIRECTION('',(0.,0.,1.));
#24930=DIRECTION('center_axis',(0.,0.,-1.));
#24931=DIRECTION('ref_axis',(1.,0.,0.));
#24932=DIRECTION('center_axis',(0.,0.,1.));
#24933=DIRECTION('ref_axis',(1.,0.,0.));
#24934=DIRECTION('center_axis',(0.,0.,1.));
#24935=DIRECTION('ref_axis',(1.,0.,0.));
#24936=DIRECTION('',(0.,0.,1.));
#24937=DIRECTION('center_axis',(0.,0.,-1.));
#24938=DIRECTION('ref_axis',(1.,0.,0.));
#24939=DIRECTION('center_axis',(0.294085848837523,0.95577900872195,0.));
#24940=DIRECTION('ref_axis',(-0.95577900872195,0.294085848837523,0.));
#24941=DIRECTION('',(-0.95577900872195,0.294085848837523,0.));
#24942=DIRECTION('',(0.,0.,-1.));
#24943=DIRECTION('',(-0.95577900872195,0.294085848837523,0.));
#24944=DIRECTION('',(0.,0.,1.));
#24945=DIRECTION('center_axis',(0.294085848837523,-0.95577900872195,0.));
#24946=DIRECTION('ref_axis',(0.95577900872195,0.294085848837523,0.));
#24947=DIRECTION('',(0.95577900872195,0.294085848837523,0.));
#24948=DIRECTION('',(0.95577900872195,0.294085848837523,0.));
#24949=DIRECTION('',(0.,0.,1.));
#24950=DIRECTION('center_axis',(0.,0.,1.));
#24951=DIRECTION('ref_axis',(1.,0.,0.));
#24952=DIRECTION('',(0.,1.,0.));
#24953=DIRECTION('center_axis',(0.,1.,0.));
#24954=DIRECTION('ref_axis',(-1.,0.,0.));
#24955=DIRECTION('',(0.,0.,1.));
#24956=DIRECTION('',(-1.,0.,0.));
#24957=DIRECTION('',(0.,0.,1.));
#24958=DIRECTION('',(-1.,0.,0.));
#24959=DIRECTION('center_axis',(0.,0.,1.));
#24960=DIRECTION('ref_axis',(1.,0.,0.));
#24961=DIRECTION('',(0.,1.,0.));
#24962=DIRECTION('',(1.,0.,0.));
#24963=DIRECTION('',(0.,-1.,0.));
#24964=DIRECTION('center_axis',(0.,-1.,0.));
#24965=DIRECTION('ref_axis',(1.,0.,0.));
#24966=DIRECTION('',(0.,0.,-1.));
#24967=DIRECTION('',(1.,0.,0.));
#24968=DIRECTION('',(0.,0.,1.));
#24969=DIRECTION('center_axis',(-1.,0.,0.));
#24970=DIRECTION('ref_axis',(0.,-1.,0.));
#24971=DIRECTION('',(0.,-1.,0.));
#24972=DIRECTION('center_axis',(1.,0.,0.));
#24973=DIRECTION('ref_axis',(0.,1.,0.));
#24974=DIRECTION('',(0.,1.,0.));
#24975=DIRECTION('',(0.,0.,1.));
#24976=DIRECTION('',(0.,1.,0.));
#24977=DIRECTION('',(0.,0.,1.));
#24978=DIRECTION('',(0.,1.,0.));
#24979=DIRECTION('center_axis',(0.,1.,0.));
#24980=DIRECTION('ref_axis',(-1.,0.,0.));
#24981=DIRECTION('',(-1.,0.,0.));
#24982=DIRECTION('',(0.,0.,1.));
#24983=DIRECTION('',(-1.,0.,0.));
#24984=DIRECTION('center_axis',(0.,-1.,0.));
#24985=DIRECTION('ref_axis',(1.,0.,0.));
#24986=DIRECTION('',(1.,0.,0.));
#24987=DIRECTION('',(1.,0.,0.));
#24988=DIRECTION('',(0.,0.,1.));
#24989=DIRECTION('center_axis',(-1.,0.,0.));
#24990=DIRECTION('ref_axis',(0.,-1.,0.));
#24991=DIRECTION('',(0.,-1.,0.));
#24992=DIRECTION('',(0.,-1.,0.));
#24993=DIRECTION('',(0.,-1.,0.));
#24994=DIRECTION('center_axis',(0.,0.,1.));
#24995=DIRECTION('ref_axis',(1.,0.,0.));
#24996=DIRECTION('center_axis',(0.,0.,1.));
#24997=DIRECTION('ref_axis',(1.,0.,0.));
#24998=DIRECTION('axis',(0.,0.,1.));
#24999=DIRECTION('refdir',(1.,0.,0.));
#25000=DIRECTION('axis',(0.,0.,1.));
#25001=DIRECTION('refdir',(1.,0.,0.));
#25002=DIRECTION('center_axis',(0.,1.,0.));
#25003=DIRECTION('ref_axis',(0.,0.,1.));
#25004=DIRECTION('center_axis',(0.,-1.,0.));
#25005=DIRECTION('ref_axis',(1.,0.,0.));
#25006=DIRECTION('',(-1.,0.,0.));
#25007=DIRECTION('',(0.,0.,-1.));
#25008=DIRECTION('',(1.,0.,0.));
#25009=DIRECTION('center_axis',(0.,0.,1.));
#25010=DIRECTION('ref_axis',(1.,0.,0.));
#25011=DIRECTION('',(0.,-1.,0.));
#25012=DIRECTION('',(0.,1.,0.));
#25013=DIRECTION('',(-1.,0.,0.));
#25014=DIRECTION('center_axis',(0.,-1.,0.));
#25015=DIRECTION('ref_axis',(0.,0.,-1.));
#25016=DIRECTION('center_axis',(0.,1.,0.));
#25017=DIRECTION('ref_axis',(1.,0.,0.));
#25018=DIRECTION('',(0.,0.,1.));
#25019=DIRECTION('',(1.,0.,0.));
#25020=DIRECTION('center_axis',(0.,0.,-1.));
#25021=DIRECTION('ref_axis',(-1.,0.,0.));
#25022=DIRECTION('',(0.,1.,0.));
#25023=DIRECTION('',(0.,1.,0.));
#25024=DIRECTION('center_axis',(1.,0.,0.));
#25025=DIRECTION('ref_axis',(0.,0.,-1.));
#25026=DIRECTION('center_axis',(0.,1.,0.));
#25027=DIRECTION('ref_axis',(0.,0.,1.));
#25028=DIRECTION('center_axis',(0.,-1.,0.));
#25029=DIRECTION('ref_axis',(1.,0.,0.));
#25030=DIRECTION('center_axis',(0.,-1.,0.));
#25031=DIRECTION('ref_axis',(1.,0.,0.));
#25032=DIRECTION('center_axis',(0.,-1.,0.));
#25033=DIRECTION('ref_axis',(1.,0.,0.));
#25034=DIRECTION('center_axis',(0.,-1.,0.));
#25035=DIRECTION('ref_axis',(1.,0.,0.));
#25036=DIRECTION('',(0.,1.,0.));
#25037=DIRECTION('center_axis',(0.,-1.,0.));
#25038=DIRECTION('ref_axis',(0.,0.,-1.));
#25039=DIRECTION('center_axis',(0.,-1.,0.));
#25040=DIRECTION('ref_axis',(1.,0.,0.));
#25041=DIRECTION('center_axis',(0.,-1.,0.));
#25042=DIRECTION('ref_axis',(1.,0.,0.));
#25043=DIRECTION('center_axis',(0.,-1.,0.));
#25044=DIRECTION('ref_axis',(1.,0.,0.));
#25045=DIRECTION('',(0.,1.,0.));
#25046=DIRECTION('center_axis',(0.,1.,0.));
#25047=DIRECTION('ref_axis',(0.,0.,1.));
#25048=DIRECTION('center_axis',(0.,-1.,0.));
#25049=DIRECTION('ref_axis',(1.,0.,0.));
#25050=DIRECTION('center_axis',(0.,-1.,0.));
#25051=DIRECTION('ref_axis',(1.,0.,0.));
#25052=DIRECTION('center_axis',(0.,-1.,0.));
#25053=DIRECTION('ref_axis',(1.,0.,0.));
#25054=DIRECTION('',(0.,1.,0.));
#25055=DIRECTION('center_axis',(0.,-1.,0.));
#25056=DIRECTION('ref_axis',(0.,0.,-1.));
#25057=DIRECTION('center_axis',(0.,-1.,0.));
#25058=DIRECTION('ref_axis',(1.,0.,0.));
#25059=DIRECTION('center_axis',(0.,-1.,0.));
#25060=DIRECTION('ref_axis',(1.,0.,0.));
#25061=DIRECTION('center_axis',(0.,-1.,0.));
#25062=DIRECTION('ref_axis',(1.,0.,0.));
#25063=DIRECTION('',(0.,1.,0.));
#25064=DIRECTION('center_axis',(0.,1.,0.));
#25065=DIRECTION('ref_axis',(0.,0.,1.));
#25066=DIRECTION('center_axis',(0.,-1.,0.));
#25067=DIRECTION('ref_axis',(1.,0.,0.));
#25068=DIRECTION('center_axis',(0.,-1.,0.));
#25069=DIRECTION('ref_axis',(1.,0.,0.));
#25070=DIRECTION('center_axis',(0.,-1.,0.));
#25071=DIRECTION('ref_axis',(1.,0.,0.));
#25072=DIRECTION('',(0.,1.,0.));
#25073=DIRECTION('center_axis',(0.,-1.,0.));
#25074=DIRECTION('ref_axis',(0.,0.,-1.));
#25075=DIRECTION('center_axis',(0.,-1.,0.));
#25076=DIRECTION('ref_axis',(1.,0.,0.));
#25077=DIRECTION('center_axis',(0.,-1.,0.));
#25078=DIRECTION('ref_axis',(1.,0.,0.));
#25079=DIRECTION('',(0.,1.,0.));
#25080=DIRECTION('axis',(0.,0.,1.));
#25081=DIRECTION('refdir',(1.,0.,0.));
#25082=DIRECTION('center_axis',(0.,1.,0.));
#25083=DIRECTION('ref_axis',(0.,0.,1.));
#25084=DIRECTION('center_axis',(0.,1.,0.));
#25085=DIRECTION('ref_axis',(1.,0.,0.));
#25086=DIRECTION('',(1.,0.,0.));
#25087=DIRECTION('center_axis',(0.,-1.,0.));
#25088=DIRECTION('ref_axis',(1.,0.,0.));
#25089=DIRECTION('',(-1.,0.,0.));
#25090=DIRECTION('center_axis',(0.,0.,-1.));
#25091=DIRECTION('ref_axis',(-1.,0.,0.));
#25092=DIRECTION('',(0.,-1.,0.));
#25093=DIRECTION('',(0.,1.,0.));
#25094=DIRECTION('',(1.,0.,0.));
#25095=DIRECTION('center_axis',(0.,-1.,0.));
#25096=DIRECTION('ref_axis',(0.,0.,-1.));
#25097=DIRECTION('center_axis',(0.,-1.,0.));
#25098=DIRECTION('ref_axis',(1.,0.,0.));
#25099=DIRECTION('center_axis',(0.,1.,0.));
#25100=DIRECTION('ref_axis',(1.,0.,0.));
#25101=DIRECTION('',(-1.,0.,0.));
#25102=DIRECTION('center_axis',(0.,0.,1.));
#25103=DIRECTION('ref_axis',(1.,0.,0.));
#25104=DIRECTION('',(0.,1.,0.));
#25105=DIRECTION('',(0.,-1.,0.));
#25106=DIRECTION('center_axis',(0.,1.,0.));
#25107=DIRECTION('ref_axis',(0.,0.,1.));
#25108=DIRECTION('center_axis',(0.,-1.,0.));
#25109=DIRECTION('ref_axis',(1.,0.,0.));
#25110=DIRECTION('center_axis',(0.,-1.,0.));
#25111=DIRECTION('ref_axis',(1.,0.,0.));
#25112=DIRECTION('center_axis',(0.,-1.,0.));
#25113=DIRECTION('ref_axis',(1.,0.,0.));
#25114=DIRECTION('center_axis',(0.,-1.,0.));
#25115=DIRECTION('ref_axis',(1.,0.,0.));
#25116=DIRECTION('',(0.,1.,0.));
#25117=DIRECTION('center_axis',(0.,-1.,0.));
#25118=DIRECTION('ref_axis',(0.,0.,-1.));
#25119=DIRECTION('center_axis',(0.,-1.,0.));
#25120=DIRECTION('ref_axis',(1.,0.,0.));
#25121=DIRECTION('center_axis',(0.,-1.,0.));
#25122=DIRECTION('ref_axis',(1.,0.,0.));
#25123=DIRECTION('',(0.,1.,0.));
#25124=DIRECTION('',(0.,0.,1.));
#25125=DIRECTION('',(1.,0.,0.));
#25126=DIRECTION('',(0.,0.,1.));
#25127=DIRECTION('',(1.,0.,0.));
#25128=DIRECTION('axis',(0.,0.,1.));
#25129=DIRECTION('refdir',(1.,0.,0.));
#25130=DIRECTION('center_axis',(1.,0.,0.));
#25131=DIRECTION('ref_axis',(0.,0.207879895528894,-0.978154358490978));
#25132=DIRECTION('',(-1.,0.,0.));
#25133=DIRECTION('center_axis',(1.,0.,0.));
#25134=DIRECTION('ref_axis',(0.,0.,-1.));
#25135=DIRECTION('center_axis',(1.,0.,0.));
#25136=DIRECTION('ref_axis',(0.,0.,-1.));
#25137=DIRECTION('',(-1.,0.,0.));
#25138=DIRECTION('center_axis',(1.,0.,0.));
#25139=DIRECTION('ref_axis',(0.,0.,-1.));
#25140=DIRECTION('',(-1.,0.,0.));
#25141=DIRECTION('center_axis',(1.,0.,0.));
#25142=DIRECTION('ref_axis',(0.,0.,-1.));
#25143=DIRECTION('',(-1.,0.,0.));
#25144=DIRECTION('center_axis',(1.,0.,0.));
#25145=DIRECTION('ref_axis',(0.,0.,-1.));
#25146=DIRECTION('',(-1.,0.,0.));
#25147=DIRECTION('center_axis',(1.,0.,0.));
#25148=DIRECTION('ref_axis',(0.,0.,-1.));
#25149=DIRECTION('',(-1.,0.,0.));
#25150=DIRECTION('center_axis',(1.,0.,0.));
#25151=DIRECTION('ref_axis',(0.,0.,-1.));
#25152=DIRECTION('',(-1.,0.,0.));
#25153=DIRECTION('center_axis',(1.,0.,0.));
#25154=DIRECTION('ref_axis',(0.,0.,-1.));
#25155=DIRECTION('',(-1.,0.,0.));
#25156=DIRECTION('center_axis',(1.,0.,0.));
#25157=DIRECTION('ref_axis',(0.,0.,-1.));
#25158=DIRECTION('',(-1.,0.,0.));
#25159=DIRECTION('center_axis',(1.,0.,0.));
#25160=DIRECTION('ref_axis',(0.,0.,-1.));
#25161=DIRECTION('center_axis',(1.,0.,0.));
#25162=DIRECTION('ref_axis',(0.,2.68771689099506E-14,-1.));
#25163=DIRECTION('',(1.,3.30650148539799E-30,-1.22464679914735E-16));
#25164=DIRECTION('center_axis',(-1.,0.,0.));
#25165=DIRECTION('ref_axis',(0.,2.68771689099506E-14,-1.));
#25166=DIRECTION('center_axis',(1.,0.,0.));
#25167=DIRECTION('ref_axis',(0.,2.68771689099506E-14,-1.));
#25168=DIRECTION('',(1.,3.30650148539799E-30,-1.22464679914735E-16));
#25169=DIRECTION('center_axis',(1.,0.,0.));
#25170=DIRECTION('ref_axis',(0.,2.68771689099506E-14,-1.));
#25171=DIRECTION('',(1.,3.30650148539799E-30,-1.22464679914735E-16));
#25172=DIRECTION('center_axis',(1.,0.,0.));
#25173=DIRECTION('ref_axis',(0.,2.68771689099506E-14,-1.));
#25174=DIRECTION('',(1.,3.30650148539799E-30,-1.22464679914735E-16));
#25175=DIRECTION('center_axis',(1.,0.,0.));
#25176=DIRECTION('ref_axis',(0.,2.68771689099506E-14,-1.));
#25177=DIRECTION('',(1.,3.30650148539799E-30,-1.22464679914735E-16));
#25178=DIRECTION('center_axis',(1.,0.,0.));
#25179=DIRECTION('ref_axis',(0.,2.68771689099506E-14,-1.));
#25180=DIRECTION('',(1.,3.30650148539799E-30,-1.22464679914735E-16));
#25181=DIRECTION('center_axis',(1.,0.,0.));
#25182=DIRECTION('ref_axis',(0.,2.68771689099506E-14,-1.));
#25183=DIRECTION('',(1.,3.30650148539799E-30,-1.22464679914735E-16));
#25184=DIRECTION('center_axis',(1.,0.,0.));
#25185=DIRECTION('ref_axis',(0.,2.68771689099506E-14,-1.));
#25186=DIRECTION('',(1.,3.30650148539799E-30,-1.22464679914735E-16));
#25187=DIRECTION('center_axis',(1.,0.,0.));
#25188=DIRECTION('ref_axis',(0.,2.68771689099506E-14,-1.));
#25189=DIRECTION('',(1.,3.30650148539799E-30,-1.22464679914735E-16));
#25190=DIRECTION('center_axis',(1.,0.,0.));
#25191=DIRECTION('ref_axis',(0.,2.68771689099506E-14,-1.));
#25192=DIRECTION('center_axis',(1.,0.,0.));
#25193=DIRECTION('ref_axis',(0.,2.68771689099506E-14,-1.));
#25194=DIRECTION('center_axis',(1.,0.,0.));
#25195=DIRECTION('ref_axis',(0.,0.,-1.));
#25196=DIRECTION('',(0.,1.,0.));
#25197=DIRECTION('center_axis',(1.,0.,0.));
#25198=DIRECTION('ref_axis',(0.,0.,-1.));
#25199=DIRECTION('center_axis',(1.,0.,0.));
#25200=DIRECTION('ref_axis',(0.,0.,-1.));
#25201=DIRECTION('center_axis',(-1.,0.,0.));
#25202=DIRECTION('ref_axis',(0.,0.,-1.));
#25203=DIRECTION('center_axis',(-1.,0.,0.));
#25204=DIRECTION('ref_axis',(0.,0.,-1.));
#25205=DIRECTION('center_axis',(-1.,0.,0.));
#25206=DIRECTION('ref_axis',(0.,0.,-1.));
#25207=DIRECTION('center_axis',(1.,0.,0.));
#25208=DIRECTION('ref_axis',(0.,0.,-1.));
#25209=DIRECTION('center_axis',(1.,0.,0.));
#25210=DIRECTION('ref_axis',(0.,0.,-1.));
#25211=DIRECTION('',(1.,0.,0.));
#25212=DIRECTION('center_axis',(1.,0.,0.));
#25213=DIRECTION('ref_axis',(0.,0.,-1.));
#25214=DIRECTION('center_axis',(1.,0.,0.));
#25215=DIRECTION('ref_axis',(0.,0.,-1.));
#25216=DIRECTION('',(1.,0.,0.));
#25217=DIRECTION('center_axis',(1.,0.,0.));
#25218=DIRECTION('ref_axis',(0.,0.,-1.));
#25219=DIRECTION('center_axis',(1.,0.,0.));
#25220=DIRECTION('ref_axis',(0.,0.,-1.));
#25221=DIRECTION('',(1.,0.,0.));
#25222=DIRECTION('center_axis',(0.,0.,1.));
#25223=DIRECTION('ref_axis',(0.,-1.,0.));
#25224=DIRECTION('',(0.,-1.,0.));
#25225=DIRECTION('',(-1.,0.,0.));
#25226=DIRECTION('',(1.,0.,0.));
#25227=DIRECTION('center_axis',(1.,0.,0.));
#25228=DIRECTION('ref_axis',(0.,0.,-1.));
#25229=DIRECTION('center_axis',(1.,0.,0.));
#25230=DIRECTION('ref_axis',(0.,0.,-1.));
#25231=DIRECTION('center_axis',(1.,0.,0.));
#25232=DIRECTION('ref_axis',(0.,0.,-1.));
#25233=DIRECTION('center_axis',(1.,0.,0.));
#25234=DIRECTION('ref_axis',(0.,-1.22464679914735E-16,1.));
#25235=DIRECTION('center_axis',(1.,0.,0.));
#25236=DIRECTION('ref_axis',(0.,0.,-1.));
#25237=DIRECTION('center_axis',(1.,0.,0.));
#25238=DIRECTION('ref_axis',(0.,0.,-1.));
#25239=DIRECTION('',(-1.,0.,0.));
#25240=DIRECTION('center_axis',(1.,0.,0.));
#25241=DIRECTION('ref_axis',(0.,0.,-1.));
#25242=DIRECTION('center_axis',(1.,0.,0.));
#25243=DIRECTION('ref_axis',(0.,0.,-1.));
#25244=DIRECTION('axis',(0.,0.,1.));
#25245=DIRECTION('refdir',(1.,0.,0.));
#25246=DIRECTION('center_axis',(0.866025403784439,0.,-0.5));
#25247=DIRECTION('ref_axis',(0.5,0.,0.866025403784439));
#25248=DIRECTION('',(-0.5,0.,-0.866025403784439));
#25249=DIRECTION('',(0.,-1.,0.));
#25250=DIRECTION('',(0.5,0.,0.866025403784439));
#25251=DIRECTION('',(0.,-1.,0.));
#25252=DIRECTION('center_axis',(1.60246890531964E-16,0.,-1.));
#25253=DIRECTION('ref_axis',(1.,0.,1.60246890531964E-16));
#25254=DIRECTION('',(-1.,0.,-1.60246890531964E-16));
#25255=DIRECTION('',(0.,-1.,0.));
#25256=DIRECTION('',(1.,0.,1.60246890531964E-16));
#25257=DIRECTION('center_axis',(-0.866025403784439,0.,-0.5));
#25258=DIRECTION('ref_axis',(0.5,0.,-0.866025403784439));
#25259=DIRECTION('',(-0.5,0.,0.866025403784439));
#25260=DIRECTION('',(0.,-1.,0.));
#25261=DIRECTION('',(0.5,0.,-0.866025403784439));
#25262=DIRECTION('center_axis',(-0.866025403784439,0.,0.5));
#25263=DIRECTION('ref_axis',(-0.5,0.,-0.866025403784439));
#25264=DIRECTION('',(0.5,0.,0.866025403784439));
#25265=DIRECTION('',(0.,-1.,0.));
#25266=DIRECTION('',(-0.5,0.,-0.866025403784439));
#25267=DIRECTION('center_axis',(-1.60246890531964E-16,0.,1.));
#25268=DIRECTION('ref_axis',(-1.,0.,-1.60246890531964E-16));
#25269=DIRECTION('',(1.,0.,1.60246890531964E-16));
#25270=DIRECTION('',(0.,-1.,0.));
#25271=DIRECTION('',(-1.,0.,-1.60246890531964E-16));
#25272=DIRECTION('center_axis',(0.866025403784439,0.,0.5));
#25273=DIRECTION('ref_axis',(-0.5,0.,0.866025403784439));
#25274=DIRECTION('',(0.5,0.,-0.866025403784439));
#25275=DIRECTION('',(-0.5,0.,0.866025403784439));
#25276=DIRECTION('center_axis',(0.,1.,0.));
#25277=DIRECTION('ref_axis',(1.,0.,0.));
#25278=DIRECTION('center_axis',(0.,-1.,0.));
#25279=DIRECTION('ref_axis',(0.,0.,-1.));
#25280=DIRECTION('center_axis',(0.,1.,0.));
#25281=DIRECTION('ref_axis',(1.,0.,0.));
#25282=DIRECTION('center_axis',(0.,1.,0.));
#25283=DIRECTION('ref_axis',(1.,0.,0.));
#25284=DIRECTION('center_axis',(0.,1.,0.));
#25285=DIRECTION('ref_axis',(1.,0.,0.));
#25286=DIRECTION('center_axis',(0.,1.,0.));
#25287=DIRECTION('ref_axis',(1.,0.,0.));
#25288=DIRECTION('',(0.,-1.,0.));
#25289=DIRECTION('center_axis',(0.,1.,0.));
#25290=DIRECTION('ref_axis',(1.,0.,0.));
#25291=DIRECTION('center_axis',(0.,1.,0.));
#25292=DIRECTION('ref_axis',(1.,0.,0.));
#25293=DIRECTION('center_axis',(0.,1.,0.));
#25294=DIRECTION('ref_axis',(0.,0.,1.));
#25295=DIRECTION('center_axis',(0.,-1.,0.));
#25296=DIRECTION('ref_axis',(1.,0.,0.));
#25297=DIRECTION('center_axis',(0.,-1.,0.));
#25298=DIRECTION('ref_axis',(1.,0.,0.));
#25299=DIRECTION('center_axis',(0.,-1.,0.));
#25300=DIRECTION('ref_axis',(1.,0.,0.));
#25301=DIRECTION('',(0.707106781186547,0.707106781186548,8.65956056235493E-17));
#25302=DIRECTION('center_axis',(0.,-1.,0.));
#25303=DIRECTION('ref_axis',(1.,0.,0.));
#25304=DIRECTION('center_axis',(0.,-1.,0.));
#25305=DIRECTION('ref_axis',(1.,0.,0.));
#25306=DIRECTION('',(0.,1.,0.));
#25307=DIRECTION('center_axis',(0.,1.,0.));
#25308=DIRECTION('ref_axis',(1.,0.,0.));
#25309=DIRECTION('center_axis',(0.,-1.,0.));
#25310=DIRECTION('ref_axis',(1.,0.,0.));
#25311=DIRECTION('',(-0.707106781186547,0.707106781186548,-8.65956056235493E-17));
#25312=DIRECTION('center_axis',(0.,-1.,0.));
#25313=DIRECTION('ref_axis',(0.,0.,-1.));
#25314=DIRECTION('center_axis',(0.,-1.,0.));
#25315=DIRECTION('ref_axis',(1.,0.,0.));
#25316=DIRECTION('center_axis',(0.,1.,0.));
#25317=DIRECTION('ref_axis',(1.,0.,0.));
#25318=DIRECTION('center_axis',(0.,1.,0.));
#25319=DIRECTION('ref_axis',(1.,0.,0.));
#25320=DIRECTION('',(-0.447213595499958,0.894427190999916,-5.47678698264203E-17));
#25321=DIRECTION('center_axis',(0.,-1.,0.));
#25322=DIRECTION('ref_axis',(1.,0.,0.));
#25323=DIRECTION('',(0.,1.,0.));
#25324=DIRECTION('axis',(0.,0.,1.));
#25325=DIRECTION('refdir',(1.,0.,0.));
#25326=DIRECTION('center_axis',(0.,1.,0.));
#25327=DIRECTION('ref_axis',(0.,0.,1.));
#25328=DIRECTION('center_axis',(0.,-1.,0.));
#25329=DIRECTION('ref_axis',(1.,0.,0.));
#25330=DIRECTION('center_axis',(0.,-1.,0.));
#25331=DIRECTION('ref_axis',(1.,0.,0.));
#25332=DIRECTION('center_axis',(0.,-1.,0.));
#25333=DIRECTION('ref_axis',(1.,0.,0.));
#25334=DIRECTION('',(0.707106781186547,0.707106781186548,8.65956056235493E-17));
#25335=DIRECTION('center_axis',(0.,-1.,0.));
#25336=DIRECTION('ref_axis',(1.,0.,0.));
#25337=DIRECTION('center_axis',(0.,-1.,0.));
#25338=DIRECTION('ref_axis',(1.,0.,0.));
#25339=DIRECTION('',(0.,1.,0.));
#25340=DIRECTION('center_axis',(0.,1.,0.));
#25341=DIRECTION('ref_axis',(1.,0.,0.));
#25342=DIRECTION('center_axis',(0.,-1.,0.));
#25343=DIRECTION('ref_axis',(1.,0.,0.));
#25344=DIRECTION('',(-0.707106781186547,0.707106781186548,-8.65956056235493E-17));
#25345=DIRECTION('center_axis',(0.,-1.,0.));
#25346=DIRECTION('ref_axis',(0.,0.,-1.));
#25347=DIRECTION('center_axis',(0.,-1.,0.));
#25348=DIRECTION('ref_axis',(1.,0.,0.));
#25349=DIRECTION('center_axis',(0.,1.,0.));
#25350=DIRECTION('ref_axis',(1.,0.,0.));
#25351=DIRECTION('center_axis',(0.,1.,0.));
#25352=DIRECTION('ref_axis',(1.,0.,0.));
#25353=DIRECTION('',(-0.447213595499958,0.894427190999916,-5.47678698264203E-17));
#25354=DIRECTION('center_axis',(0.,-1.,0.));
#25355=DIRECTION('ref_axis',(1.,0.,0.));
#25356=DIRECTION('center_axis',(0.,1.,0.));
#25357=DIRECTION('ref_axis',(1.,0.,0.));
#25358=DIRECTION('',(0.,1.,0.));
#25359=DIRECTION('center_axis',(0.,1.,0.));
#25360=DIRECTION('ref_axis',(1.,0.,0.));
#25361=DIRECTION('center_axis',(0.,-1.,0.));
#25362=DIRECTION('ref_axis',(1.,0.,0.));
#25363=DIRECTION('',(-0.707106781186547,0.707106781186548,-8.65956056235493E-17));
#25364=DIRECTION('center_axis',(0.,-1.,0.));
#25365=DIRECTION('ref_axis',(0.,0.,-1.));
#25366=DIRECTION('center_axis',(0.866025403784439,0.,-0.5));
#25367=DIRECTION('ref_axis',(0.5,0.,0.866025403784439));
#25368=DIRECTION('',(-0.5,0.,-0.866025403784439));
#25369=DIRECTION('',(0.,-1.,0.));
#25370=DIRECTION('',(0.5,0.,0.866025403784439));
#25371=DIRECTION('',(0.,-1.,0.));
#25372=DIRECTION('center_axis',(1.60246890531964E-16,0.,-1.));
#25373=DIRECTION('ref_axis',(1.,0.,1.60246890531964E-16));
#25374=DIRECTION('',(-1.,0.,-1.60246890531964E-16));
#25375=DIRECTION('',(0.,-1.,0.));
#25376=DIRECTION('',(1.,0.,1.60246890531964E-16));
#25377=DIRECTION('center_axis',(-0.866025403784439,0.,-0.5));
#25378=DIRECTION('ref_axis',(0.5,0.,-0.866025403784439));
#25379=DIRECTION('',(-0.5,0.,0.866025403784439));
#25380=DIRECTION('',(0.,-1.,0.));
#25381=DIRECTION('',(0.5,0.,-0.866025403784439));
#25382=DIRECTION('center_axis',(-0.866025403784439,0.,0.5));
#25383=DIRECTION('ref_axis',(-0.5,0.,-0.866025403784439));
#25384=DIRECTION('',(0.5,0.,0.866025403784439));
#25385=DIRECTION('',(0.,-1.,0.));
#25386=DIRECTION('',(-0.5,0.,-0.866025403784439));
#25387=DIRECTION('center_axis',(-1.60246890531964E-16,0.,1.));
#25388=DIRECTION('ref_axis',(-1.,0.,-1.60246890531964E-16));
#25389=DIRECTION('',(1.,0.,1.60246890531964E-16));
#25390=DIRECTION('',(0.,-1.,0.));
#25391=DIRECTION('',(-1.,0.,-1.60246890531964E-16));
#25392=DIRECTION('center_axis',(0.866025403784439,0.,0.5));
#25393=DIRECTION('ref_axis',(-0.5,0.,0.866025403784439));
#25394=DIRECTION('',(0.5,0.,-0.866025403784439));
#25395=DIRECTION('',(-0.5,0.,0.866025403784439));
#25396=DIRECTION('center_axis',(0.,1.,0.));
#25397=DIRECTION('ref_axis',(1.,0.,0.));
#25398=DIRECTION('center_axis',(0.,-1.,0.));
#25399=DIRECTION('ref_axis',(0.,0.,-1.));
#25400=DIRECTION('',(0.,0.,1.));
#25401=DIRECTION('',(1.,0.,0.));
#25402=DIRECTION('',(0.,0.,1.));
#25403=DIRECTION('',(1.,0.,0.));
#25404=DIRECTION('',(0.,0.,1.));
#25405=DIRECTION('',(1.,0.,0.));
#25406=DIRECTION('',(0.,0.,1.));
#25407=DIRECTION('',(1.,0.,0.));
#25408=DIRECTION('',(0.,0.,1.));
#25409=DIRECTION('',(1.,0.,0.));
#25410=DIRECTION('',(0.,0.,1.));
#25411=DIRECTION('',(1.,0.,0.));
#25412=DIRECTION('',(0.,0.,1.));
#25413=DIRECTION('',(1.,0.,0.));
#25414=DIRECTION('',(0.,0.,1.));
#25415=DIRECTION('',(1.,0.,0.));
#25416=DIRECTION('',(0.,0.,1.));
#25417=DIRECTION('',(1.,0.,0.));
#25418=DIRECTION('',(0.,0.,1.));
#25419=DIRECTION('',(1.,0.,0.));
#25420=DIRECTION('',(0.,0.,1.));
#25421=DIRECTION('',(1.,0.,0.));
#25422=DIRECTION('',(0.,0.,1.));
#25423=DIRECTION('',(1.,0.,0.));
#25424=DIRECTION('',(0.,0.,1.));
#25425=DIRECTION('',(1.,0.,0.));
#25426=DIRECTION('',(0.,0.,1.));
#25427=DIRECTION('',(1.,0.,0.));
#25428=DIRECTION('',(0.,0.,1.));
#25429=DIRECTION('',(1.,0.,0.));
#25430=DIRECTION('',(0.,0.,1.));
#25431=DIRECTION('',(1.,0.,0.));
#25432=DIRECTION('',(0.,0.,1.));
#25433=DIRECTION('',(1.,0.,0.));
#25434=DIRECTION('',(0.,0.,1.));
#25435=DIRECTION('',(1.,0.,0.));
#25436=DIRECTION('',(0.,0.,1.));
#25437=DIRECTION('',(1.,0.,0.));
#25438=DIRECTION('',(0.,0.,1.));
#25439=DIRECTION('',(1.,0.,0.));
#25440=DIRECTION('',(0.,1.,2.22044604925031E-16));
#25441=DIRECTION('',(1.,0.,0.));
#25442=DIRECTION('',(0.,-1.,2.22044604925031E-16));
#25443=DIRECTION('',(1.,0.,0.));
#25444=DIRECTION('',(0.,1.,2.22044604925031E-16));
#25445=DIRECTION('',(1.,0.,0.));
#25446=DIRECTION('',(0.,-1.,2.22044604925031E-16));
#25447=DIRECTION('',(1.,0.,0.));
#25448=DIRECTION('',(0.,1.,2.22044604925031E-16));
#25449=DIRECTION('',(1.,0.,0.));
#25450=DIRECTION('',(0.,-1.,2.22044604925031E-16));
#25451=DIRECTION('',(1.,0.,0.));
#25452=DIRECTION('',(0.,1.,2.22044604925031E-16));
#25453=DIRECTION('',(1.,0.,0.));
#25454=DIRECTION('',(0.,-1.,2.22044604925031E-16));
#25455=DIRECTION('',(1.,0.,0.));
#25456=DIRECTION('',(-1.,0.,2.22044604925031E-16));
#25457=DIRECTION('',(2.22044604925031E-16,0.,1.));
#25458=DIRECTION('',(0.,-1.,2.22044604925031E-16));
#25459=DIRECTION('',(1.,0.,0.));
#25460=DIRECTION('',(0.,0.,1.));
#25461=DIRECTION('',(-1.,1.22464679914735E-16,0.));
#25462=DIRECTION('',(0.,0.,1.));
#25463=DIRECTION('',(-1.,1.22464679914735E-16,0.));
#25464=DIRECTION('',(0.,0.,1.));
#25465=DIRECTION('',(2.22044604925031E-16,-1.,0.));
#25466=DIRECTION('',(0.,1.,2.22044604925031E-16));
#25467=DIRECTION('',(1.,0.,0.));
#25468=DIRECTION('',(0.,1.,2.22044604925031E-16));
#25469=DIRECTION('',(1.,0.,0.));
#25470=DIRECTION('',(0.,-1.,2.22044604925031E-16));
#25471=DIRECTION('',(1.,0.,0.));
#25472=DIRECTION('',(0.,0.,1.));
#25473=DIRECTION('',(-1.,1.22464679914735E-16,0.));
#25474=DIRECTION('',(0.,0.,1.));
#25475=DIRECTION('',(-1.,1.22464679914735E-16,0.));
#25476=DIRECTION('',(0.,0.,1.));
#25477=DIRECTION('',(2.22044604925031E-16,-1.,0.));
#25478=DIRECTION('',(0.,-1.,2.22044604925031E-16));
#25479=DIRECTION('',(1.,0.,0.));
#25480=DIRECTION('',(0.,-1.,2.22044604925031E-16));
#25481=DIRECTION('',(1.,0.,0.));
#25482=DIRECTION('',(-1.,0.,2.22044604925031E-16));
#25483=DIRECTION('',(2.22044604925031E-16,0.,1.));
#25484=DIRECTION('',(0.,-1.,2.22044604925031E-16));
#25485=DIRECTION('',(1.,0.,0.));
#25486=DIRECTION('',(0.,0.,1.));
#25487=DIRECTION('',(-1.,1.22464679914735E-16,0.));
#25488=DIRECTION('',(0.,0.,1.));
#25489=DIRECTION('',(-1.,1.22464679914735E-16,0.));
#25490=DIRECTION('',(0.,0.,1.));
#25491=DIRECTION('',(2.22044604925031E-16,-1.,0.));
#25492=DIRECTION('',(0.,1.,2.22044604925031E-16));
#25493=DIRECTION('',(1.,0.,0.));
#25494=DIRECTION('',(0.,1.,2.22044604925031E-16));
#25495=DIRECTION('',(1.,0.,0.));
#25496=DIRECTION('',(0.,-1.,2.22044604925031E-16));
#25497=DIRECTION('',(1.,0.,0.));
#25498=DIRECTION('',(0.,0.,1.));
#25499=DIRECTION('',(-1.,1.22464679914735E-16,0.));
#25500=DIRECTION('',(0.,0.,1.));
#25501=DIRECTION('',(-1.,1.22464679914735E-16,0.));
#25502=DIRECTION('',(0.,0.,1.));
#25503=DIRECTION('',(2.22044604925031E-16,-1.,0.));
#25504=DIRECTION('',(0.,-1.,2.22044604925031E-16));
#25505=DIRECTION('',(1.,0.,0.));
#25506=DIRECTION('',(0.,-1.,2.22044604925031E-16));
#25507=DIRECTION('',(1.,0.,0.));
#25508=DIRECTION('',(0.,-1.,2.22044604925031E-16));
#25509=DIRECTION('',(1.,0.,0.));
#25510=DIRECTION('',(0.,1.,2.22044604925031E-16));
#25511=DIRECTION('',(1.,0.,0.));
#25512=DIRECTION('',(0.,1.,2.22044604925031E-16));
#25513=DIRECTION('',(1.,0.,0.));
#25514=DIRECTION('',(0.,1.,2.22044604925031E-16));
#25515=DIRECTION('',(1.,0.,0.));
#25516=DIRECTION('',(0.,1.,2.22044604925031E-16));
#25517=DIRECTION('',(1.,0.,0.));
#25518=DIRECTION('',(0.,-1.,2.22044604925031E-16));
#25519=DIRECTION('',(1.,0.,0.));
#25520=DIRECTION('',(0.,0.,1.));
#25521=DIRECTION('',(2.22044604925031E-16,1.,0.));
#25522=DIRECTION('',(0.,0.,1.));
#25523=DIRECTION('',(2.22044604925031E-16,1.,0.));
#25524=DIRECTION('',(0.,0.,1.));
#25525=DIRECTION('',(2.22044604925031E-16,-1.,0.));
#25526=DIRECTION('',(0.,0.,1.));
#25527=DIRECTION('',(2.22044604925031E-16,-1.,0.));
#25528=DIRECTION('',(0.,1.,2.22044604925031E-16));
#25529=DIRECTION('',(1.,0.,0.));
#25530=DIRECTION('',(0.,1.,2.22044604925031E-16));
#25531=DIRECTION('',(1.,0.,0.));
#25532=DIRECTION('',(0.,1.,2.22044604925031E-16));
#25533=DIRECTION('',(1.,0.,0.));
#25534=DIRECTION('',(0.,-1.,2.22044604925031E-16));
#25535=DIRECTION('',(1.,0.,0.));
#25536=DIRECTION('',(0.,-1.,2.22044604925031E-16));
#25537=DIRECTION('',(1.,0.,0.));
#25538=DIRECTION('',(0.,-1.,2.22044604925031E-16));
#25539=DIRECTION('',(1.,0.,0.));
#25540=DIRECTION('',(0.,1.,2.22044604925031E-16));
#25541=DIRECTION('',(1.,0.,0.));
#25542=DIRECTION('',(0.,-1.,2.22044604925031E-16));
#25543=DIRECTION('',(1.,0.,0.));
#25544=DIRECTION('',(0.,1.,2.22044604925031E-16));
#25545=DIRECTION('',(1.,0.,0.));
#25546=DIRECTION('',(0.,-1.,2.22044604925031E-16));
#25547=DIRECTION('',(1.,0.,0.));
#25548=DIRECTION('',(0.,-1.,2.22044604925031E-16));
#25549=DIRECTION('',(1.,0.,0.));
#25550=DIRECTION('',(0.,-1.,2.22044604925031E-16));
#25551=DIRECTION('',(1.,0.,0.));
#25552=DIRECTION('',(0.,-1.,2.22044604925031E-16));
#25553=DIRECTION('',(1.,0.,0.));
#25554=DIRECTION('',(0.,-1.,2.22044604925031E-16));
#25555=DIRECTION('',(1.,0.,0.));
#25556=DIRECTION('',(-1.,0.,2.22044604925031E-16));
#25557=DIRECTION('',(2.22044604925031E-16,0.,1.));
#25558=DIRECTION('',(0.,1.,2.22044604925031E-16));
#25559=DIRECTION('',(1.,0.,0.));
#25560=DIRECTION('',(-1.,0.,2.22044604925031E-16));
#25561=DIRECTION('',(2.22044604925031E-16,0.,1.));
#25562=DIRECTION('',(0.,0.,1.));
#25563=DIRECTION('',(2.22044604925031E-16,1.,0.));
#25564=DIRECTION('',(-1.,0.,2.22044604925031E-16));
#25565=DIRECTION('',(2.22044604925031E-16,0.,1.));
#25566=DIRECTION('',(0.,0.,1.));
#25567=DIRECTION('',(2.22044604925031E-16,1.,0.));
#25568=DIRECTION('',(0.,0.,1.));
#25569=DIRECTION('',(1.,0.,0.));
#25570=DIRECTION('',(0.,0.,1.));
#25571=DIRECTION('',(1.,0.,0.));
#25572=DIRECTION('',(0.,0.,1.));
#25573=DIRECTION('',(1.,0.,0.));
#25574=DIRECTION('',(0.,0.,1.));
#25575=DIRECTION('',(1.,0.,0.));
#25576=DIRECTION('',(0.,0.,1.));
#25577=DIRECTION('',(1.,0.,0.));
#25578=DIRECTION('',(0.,0.,1.));
#25579=DIRECTION('',(1.,0.,0.));
#25580=DIRECTION('',(0.,-1.,2.22044604925031E-16));
#25581=DIRECTION('',(1.,0.,0.));
#25582=DIRECTION('',(0.,-1.,2.22044604925031E-16));
#25583=DIRECTION('',(1.,0.,0.));
#25584=DIRECTION('',(0.,-1.,2.22044604925031E-16));
#25585=DIRECTION('',(1.,0.,0.));
#25586=DIRECTION('',(0.,-1.,2.22044604925031E-16));
#25587=DIRECTION('',(1.,0.,0.));
#25588=DIRECTION('',(0.,-1.,2.22044604925031E-16));
#25589=DIRECTION('',(1.,0.,0.));
#25590=DIRECTION('',(0.,-1.,2.22044604925031E-16));
#25591=DIRECTION('',(1.,0.,0.));
#25592=DIRECTION('',(0.,-1.,2.22044604925031E-16));
#25593=DIRECTION('',(1.,0.,0.));
#25594=DIRECTION('',(0.,-1.,2.22044604925031E-16));
#25595=DIRECTION('',(1.,0.,0.));
#25596=DIRECTION('',(0.,-1.,2.22044604925031E-16));
#25597=DIRECTION('',(1.,0.,0.));
#25598=DIRECTION('',(0.,-1.,2.22044604925031E-16));
#25599=DIRECTION('',(1.,0.,0.));
#25600=DIRECTION('',(-1.,0.,2.22044604925031E-16));
#25601=DIRECTION('',(2.22044604925031E-16,0.,1.));
#25602=DIRECTION('',(0.,-1.,2.22044604925031E-16));
#25603=DIRECTION('',(1.,0.,0.));
#25604=DIRECTION('',(0.,-1.,2.22044604925031E-16));
#25605=DIRECTION('',(1.,0.,0.));
#25606=DIRECTION('',(0.,-1.,2.22044604925031E-16));
#25607=DIRECTION('',(1.,0.,0.));
#25608=DIRECTION('',(0.,-1.,2.22044604925031E-16));
#25609=DIRECTION('',(1.,0.,0.));
#25610=DIRECTION('',(0.,-1.,2.22044604925031E-16));
#25611=DIRECTION('',(1.,0.,0.));
#25612=DIRECTION('',(0.,-1.,2.22044604925031E-16));
#25613=DIRECTION('',(1.,0.,0.));
#25614=DIRECTION('',(0.,-1.,2.22044604925031E-16));
#25615=DIRECTION('',(1.,0.,0.));
#25616=DIRECTION('axis',(0.,0.,1.));
#25617=DIRECTION('refdir',(1.,0.,0.));
#25618=DIRECTION('axis',(0.,0.,1.));
#25619=DIRECTION('refdir',(1.,0.,0.));
#25620=DIRECTION('center_axis',(1.,0.,0.));
#25621=DIRECTION('ref_axis',(0.,0.975560628713931,0.219730425074181));
#25622=DIRECTION('',(-1.,0.,0.));
#25623=DIRECTION('center_axis',(-1.,0.,0.));
#25624=DIRECTION('ref_axis',(0.,0.,-1.));
#25625=DIRECTION('center_axis',(1.,0.,0.));
#25626=DIRECTION('ref_axis',(0.,0.,-1.));
#25627=DIRECTION('',(-1.,0.,0.));
#25628=DIRECTION('center_axis',(1.,0.,0.));
#25629=DIRECTION('ref_axis',(0.,0.,-1.));
#25630=DIRECTION('',(-1.,0.,0.));
#25631=DIRECTION('center_axis',(1.,0.,0.));
#25632=DIRECTION('ref_axis',(0.,0.,-1.));
#25633=DIRECTION('',(-1.,0.,0.));
#25634=DIRECTION('center_axis',(1.,0.,0.));
#25635=DIRECTION('ref_axis',(0.,0.,-1.));
#25636=DIRECTION('',(-1.,0.,0.));
#25637=DIRECTION('center_axis',(1.,0.,0.));
#25638=DIRECTION('ref_axis',(0.,0.,-1.));
#25639=DIRECTION('',(-1.,0.,0.));
#25640=DIRECTION('center_axis',(1.,0.,0.));
#25641=DIRECTION('ref_axis',(0.,0.,-1.));
#25642=DIRECTION('',(-1.,0.,0.));
#25643=DIRECTION('center_axis',(1.,0.,0.));
#25644=DIRECTION('ref_axis',(0.,0.,-1.));
#25645=DIRECTION('',(-1.,0.,0.));
#25646=DIRECTION('center_axis',(1.,0.,0.));
#25647=DIRECTION('ref_axis',(0.,0.,-1.));
#25648=DIRECTION('',(-1.,0.,0.));
#25649=DIRECTION('center_axis',(1.,0.,0.));
#25650=DIRECTION('ref_axis',(0.,0.,-1.));
#25651=DIRECTION('',(-1.,0.,0.));
#25652=DIRECTION('center_axis',(1.,0.,0.));
#25653=DIRECTION('ref_axis',(0.,0.,-1.));
#25654=DIRECTION('',(-1.,0.,0.));
#25655=DIRECTION('center_axis',(1.,0.,0.));
#25656=DIRECTION('ref_axis',(0.,0.,-1.));
#25657=DIRECTION('',(-1.,0.,0.));
#25658=DIRECTION('center_axis',(1.,0.,0.));
#25659=DIRECTION('ref_axis',(0.,0.,-1.));
#25660=DIRECTION('',(-1.,0.,0.));
#25661=DIRECTION('center_axis',(1.,0.,0.));
#25662=DIRECTION('ref_axis',(0.,0.,-1.));
#25663=DIRECTION('',(-1.,0.,0.));
#25664=DIRECTION('center_axis',(1.,0.,0.));
#25665=DIRECTION('ref_axis',(0.,0.,-1.));
#25666=DIRECTION('',(-1.,0.,0.));
#25667=DIRECTION('center_axis',(1.,0.,0.));
#25668=DIRECTION('ref_axis',(0.,0.,-1.));
#25669=DIRECTION('',(-1.,0.,0.));
#25670=DIRECTION('center_axis',(1.,0.,0.));
#25671=DIRECTION('ref_axis',(0.,0.,-1.));
#25672=DIRECTION('',(-1.,0.,0.));
#25673=DIRECTION('center_axis',(1.,0.,0.));
#25674=DIRECTION('ref_axis',(0.,0.,-1.));
#25675=DIRECTION('',(-1.,0.,0.));
#25676=DIRECTION('center_axis',(1.,0.,0.));
#25677=DIRECTION('ref_axis',(0.,0.,-1.));
#25678=DIRECTION('',(-1.,0.,0.));
#25679=DIRECTION('center_axis',(1.,0.,0.));
#25680=DIRECTION('ref_axis',(0.,0.,-1.));
#25681=DIRECTION('',(-1.,0.,0.));
#25682=DIRECTION('center_axis',(1.,0.,0.));
#25683=DIRECTION('ref_axis',(0.,0.,-1.));
#25684=DIRECTION('',(-1.,0.,0.));
#25685=DIRECTION('center_axis',(1.,0.,0.));
#25686=DIRECTION('ref_axis',(0.,0.,-1.));
#25687=DIRECTION('',(-1.,0.,0.));
#25688=DIRECTION('center_axis',(1.,0.,0.));
#25689=DIRECTION('ref_axis',(0.,0.,-1.));
#25690=DIRECTION('',(-1.,0.,0.));
#25691=DIRECTION('center_axis',(1.,0.,0.));
#25692=DIRECTION('ref_axis',(0.,0.,-1.));
#25693=DIRECTION('',(-1.,0.,0.));
#25694=DIRECTION('center_axis',(1.,0.,0.));
#25695=DIRECTION('ref_axis',(0.,0.,-1.));
#25696=DIRECTION('',(-1.,0.,0.));
#25697=DIRECTION('center_axis',(1.,0.,0.));
#25698=DIRECTION('ref_axis',(0.,0.,-1.));
#25699=DIRECTION('',(-1.,0.,0.));
#25700=DIRECTION('center_axis',(1.,0.,0.));
#25701=DIRECTION('ref_axis',(0.,0.,-1.));
#25702=DIRECTION('',(-1.,0.,0.));
#25703=DIRECTION('center_axis',(1.,0.,0.));
#25704=DIRECTION('ref_axis',(0.,0.,-1.));
#25705=DIRECTION('',(-1.,0.,0.));
#25706=DIRECTION('center_axis',(1.,0.,0.));
#25707=DIRECTION('ref_axis',(0.,0.,-1.));
#25708=DIRECTION('',(-1.,0.,0.));
#25709=DIRECTION('center_axis',(1.,0.,0.));
#25710=DIRECTION('ref_axis',(0.,0.,-1.));
#25711=DIRECTION('',(-1.,0.,0.));
#25712=DIRECTION('center_axis',(1.,0.,0.));
#25713=DIRECTION('ref_axis',(0.,0.,-1.));
#25714=DIRECTION('',(-1.,0.,0.));
#25715=DIRECTION('center_axis',(1.,0.,0.));
#25716=DIRECTION('ref_axis',(0.,0.,-1.));
#25717=DIRECTION('',(-1.,0.,0.));
#25718=DIRECTION('center_axis',(1.,0.,0.));
#25719=DIRECTION('ref_axis',(0.,0.,-1.));
#25720=DIRECTION('',(-1.,0.,0.));
#25721=DIRECTION('center_axis',(1.,0.,0.));
#25722=DIRECTION('ref_axis',(0.,0.,-1.));
#25723=DIRECTION('',(-1.,0.,0.));
#25724=DIRECTION('center_axis',(1.,0.,0.));
#25725=DIRECTION('ref_axis',(0.,0.,-1.));
#25726=DIRECTION('',(-1.,0.,0.));
#25727=DIRECTION('center_axis',(1.,0.,0.));
#25728=DIRECTION('ref_axis',(0.,0.,-1.));
#25729=DIRECTION('',(-1.,0.,0.));
#25730=DIRECTION('center_axis',(1.,0.,0.));
#25731=DIRECTION('ref_axis',(0.,0.,-1.));
#25732=DIRECTION('',(-1.,0.,0.));
#25733=DIRECTION('center_axis',(1.,0.,0.));
#25734=DIRECTION('ref_axis',(0.,0.,-1.));
#25735=DIRECTION('',(-1.,0.,0.));
#25736=DIRECTION('center_axis',(1.,0.,0.));
#25737=DIRECTION('ref_axis',(0.,0.,-1.));
#25738=DIRECTION('',(-1.,0.,0.));
#25739=DIRECTION('center_axis',(1.,0.,0.));
#25740=DIRECTION('ref_axis',(0.,0.,-1.));
#25741=DIRECTION('',(-1.,0.,0.));
#25742=DIRECTION('center_axis',(1.,0.,0.));
#25743=DIRECTION('ref_axis',(0.,0.,-1.));
#25744=DIRECTION('',(-1.,0.,0.));
#25745=DIRECTION('center_axis',(1.,0.,0.));
#25746=DIRECTION('ref_axis',(0.,0.,-1.));
#25747=DIRECTION('',(-1.,0.,0.));
#25748=DIRECTION('center_axis',(1.,0.,0.));
#25749=DIRECTION('ref_axis',(0.,0.,-1.));
#25750=DIRECTION('',(-1.,0.,0.));
#25751=DIRECTION('center_axis',(1.,0.,0.));
#25752=DIRECTION('ref_axis',(0.,0.,-1.));
#25753=DIRECTION('',(-1.,0.,0.));
#25754=DIRECTION('center_axis',(1.,0.,0.));
#25755=DIRECTION('ref_axis',(0.,0.,-1.));
#25756=DIRECTION('',(-1.,0.,0.));
#25757=DIRECTION('center_axis',(1.,0.,0.));
#25758=DIRECTION('ref_axis',(0.,0.,-1.));
#25759=DIRECTION('',(-1.,0.,0.));
#25760=DIRECTION('center_axis',(1.,0.,0.));
#25761=DIRECTION('ref_axis',(0.,0.,-1.));
#25762=DIRECTION('',(-1.,0.,0.));
#25763=DIRECTION('center_axis',(1.,0.,0.));
#25764=DIRECTION('ref_axis',(0.,0.,-1.));
#25765=DIRECTION('',(-1.,0.,0.));
#25766=DIRECTION('center_axis',(1.,0.,0.));
#25767=DIRECTION('ref_axis',(0.,0.,-1.));
#25768=DIRECTION('',(-1.,0.,0.));
#25769=DIRECTION('center_axis',(1.,0.,0.));
#25770=DIRECTION('ref_axis',(0.,0.,-1.));
#25771=DIRECTION('',(-1.,0.,0.));
#25772=DIRECTION('center_axis',(1.,0.,0.));
#25773=DIRECTION('ref_axis',(0.,0.,-1.));
#25774=DIRECTION('',(-1.,0.,0.));
#25775=DIRECTION('center_axis',(1.,0.,0.));
#25776=DIRECTION('ref_axis',(0.,0.,-1.));
#25777=DIRECTION('',(-1.,0.,0.));
#25778=DIRECTION('center_axis',(1.,0.,0.));
#25779=DIRECTION('ref_axis',(0.,0.,-1.));
#25780=DIRECTION('',(-1.,0.,0.));
#25781=DIRECTION('center_axis',(1.,0.,0.));
#25782=DIRECTION('ref_axis',(0.,0.,-1.));
#25783=DIRECTION('',(-1.,0.,0.));
#25784=DIRECTION('center_axis',(1.,0.,0.));
#25785=DIRECTION('ref_axis',(0.,0.,-1.));
#25786=DIRECTION('',(-1.,0.,0.));
#25787=DIRECTION('center_axis',(1.,0.,0.));
#25788=DIRECTION('ref_axis',(0.,0.,-1.));
#25789=DIRECTION('',(-1.,0.,0.));
#25790=DIRECTION('center_axis',(1.,0.,0.));
#25791=DIRECTION('ref_axis',(0.,0.,-1.));
#25792=DIRECTION('',(-1.,0.,0.));
#25793=DIRECTION('center_axis',(1.,0.,0.));
#25794=DIRECTION('ref_axis',(0.,0.,-1.));
#25795=DIRECTION('',(-1.,0.,0.));
#25796=DIRECTION('center_axis',(1.,0.,0.));
#25797=DIRECTION('ref_axis',(0.,0.,-1.));
#25798=DIRECTION('',(-1.,0.,0.));
#25799=DIRECTION('center_axis',(1.,0.,0.));
#25800=DIRECTION('ref_axis',(0.,0.,-1.));
#25801=DIRECTION('',(-1.,0.,0.));
#25802=DIRECTION('center_axis',(1.,0.,0.));
#25803=DIRECTION('ref_axis',(0.,0.,-1.));
#25804=DIRECTION('',(-1.,0.,0.));
#25805=DIRECTION('center_axis',(1.,0.,0.));
#25806=DIRECTION('ref_axis',(0.,0.,-1.));
#25807=DIRECTION('',(-1.,0.,0.));
#25808=DIRECTION('center_axis',(1.,0.,0.));
#25809=DIRECTION('ref_axis',(0.,0.,-1.));
#25810=DIRECTION('',(-1.,0.,0.));
#25811=DIRECTION('center_axis',(1.,0.,0.));
#25812=DIRECTION('ref_axis',(0.,-1.17203152359781E-12,-1.));
#25813=DIRECTION('',(1.,0.,0.));
#25814=DIRECTION('center_axis',(1.,0.,0.));
#25815=DIRECTION('ref_axis',(0.,-1.17203152359781E-12,-1.));
#25816=DIRECTION('center_axis',(1.,0.,0.));
#25817=DIRECTION('ref_axis',(0.,-1.17203152359781E-12,-1.));
#25818=DIRECTION('',(1.,0.,0.));
#25819=DIRECTION('center_axis',(1.,0.,0.));
#25820=DIRECTION('ref_axis',(0.,-1.17203152359781E-12,-1.));
#25821=DIRECTION('center_axis',(1.,0.,0.));
#25822=DIRECTION('ref_axis',(0.,-1.17203152359781E-12,-1.));
#25823=DIRECTION('',(1.,0.,0.));
#25824=DIRECTION('center_axis',(1.,0.,0.));
#25825=DIRECTION('ref_axis',(0.,-1.17203152359781E-12,-1.));
#25826=DIRECTION('',(1.,0.,0.));
#25827=DIRECTION('center_axis',(1.,0.,0.));
#25828=DIRECTION('ref_axis',(0.,-1.17203152359781E-12,-1.));
#25829=DIRECTION('',(1.,0.,0.));
#25830=DIRECTION('center_axis',(1.,0.,0.));
#25831=DIRECTION('ref_axis',(0.,-1.17203152359781E-12,-1.));
#25832=DIRECTION('',(1.,0.,0.));
#25833=DIRECTION('center_axis',(1.,0.,0.));
#25834=DIRECTION('ref_axis',(0.,-1.17203152359781E-12,-1.));
#25835=DIRECTION('',(1.,0.,0.));
#25836=DIRECTION('center_axis',(1.,0.,0.));
#25837=DIRECTION('ref_axis',(0.,-1.17203152359781E-12,-1.));
#25838=DIRECTION('',(1.,0.,0.));
#25839=DIRECTION('center_axis',(1.,0.,0.));
#25840=DIRECTION('ref_axis',(0.,-1.17203152359781E-12,-1.));
#25841=DIRECTION('',(1.,0.,0.));
#25842=DIRECTION('center_axis',(1.,0.,0.));
#25843=DIRECTION('ref_axis',(0.,-1.17203152359781E-12,-1.));
#25844=DIRECTION('',(1.,0.,0.));
#25845=DIRECTION('center_axis',(1.,0.,0.));
#25846=DIRECTION('ref_axis',(0.,-1.17203152359781E-12,-1.));
#25847=DIRECTION('',(1.,0.,0.));
#25848=DIRECTION('center_axis',(1.,0.,0.));
#25849=DIRECTION('ref_axis',(0.,-1.17203152359781E-12,-1.));
#25850=DIRECTION('',(1.,0.,0.));
#25851=DIRECTION('center_axis',(1.,0.,0.));
#25852=DIRECTION('ref_axis',(0.,-1.17203152359781E-12,-1.));
#25853=DIRECTION('',(1.,0.,0.));
#25854=DIRECTION('center_axis',(1.,0.,0.));
#25855=DIRECTION('ref_axis',(0.,-1.17203152359781E-12,-1.));
#25856=DIRECTION('',(1.,0.,0.));
#25857=DIRECTION('center_axis',(1.,0.,0.));
#25858=DIRECTION('ref_axis',(0.,-1.17203152359781E-12,-1.));
#25859=DIRECTION('',(1.,0.,0.));
#25860=DIRECTION('center_axis',(1.,0.,0.));
#25861=DIRECTION('ref_axis',(0.,-1.17203152359781E-12,-1.));
#25862=DIRECTION('',(1.,0.,0.));
#25863=DIRECTION('center_axis',(1.,0.,0.));
#25864=DIRECTION('ref_axis',(0.,-1.17203152359781E-12,-1.));
#25865=DIRECTION('',(1.,0.,0.));
#25866=DIRECTION('center_axis',(1.,0.,0.));
#25867=DIRECTION('ref_axis',(0.,-1.17203152359781E-12,-1.));
#25868=DIRECTION('',(1.,0.,0.));
#25869=DIRECTION('center_axis',(1.,0.,0.));
#25870=DIRECTION('ref_axis',(0.,-1.17203152359781E-12,-1.));
#25871=DIRECTION('',(1.,0.,0.));
#25872=DIRECTION('center_axis',(1.,0.,0.));
#25873=DIRECTION('ref_axis',(0.,-1.17203152359781E-12,-1.));
#25874=DIRECTION('',(1.,0.,0.));
#25875=DIRECTION('center_axis',(1.,0.,0.));
#25876=DIRECTION('ref_axis',(0.,-1.17203152359781E-12,-1.));
#25877=DIRECTION('',(1.,0.,0.));
#25878=DIRECTION('center_axis',(1.,0.,0.));
#25879=DIRECTION('ref_axis',(0.,-1.17203152359781E-12,-1.));
#25880=DIRECTION('',(1.,0.,0.));
#25881=DIRECTION('center_axis',(1.,0.,0.));
#25882=DIRECTION('ref_axis',(0.,-1.17203152359781E-12,-1.));
#25883=DIRECTION('',(1.,0.,0.));
#25884=DIRECTION('center_axis',(1.,0.,0.));
#25885=DIRECTION('ref_axis',(0.,-1.17203152359781E-12,-1.));
#25886=DIRECTION('',(1.,0.,0.));
#25887=DIRECTION('center_axis',(1.,0.,0.));
#25888=DIRECTION('ref_axis',(0.,-1.17203152359781E-12,-1.));
#25889=DIRECTION('',(1.,0.,0.));
#25890=DIRECTION('center_axis',(1.,0.,0.));
#25891=DIRECTION('ref_axis',(0.,-1.17203152359781E-12,-1.));
#25892=DIRECTION('',(1.,0.,0.));
#25893=DIRECTION('center_axis',(1.,0.,0.));
#25894=DIRECTION('ref_axis',(0.,-1.17203152359781E-12,-1.));
#25895=DIRECTION('',(1.,0.,0.));
#25896=DIRECTION('center_axis',(1.,0.,0.));
#25897=DIRECTION('ref_axis',(0.,-1.17203152359781E-12,-1.));
#25898=DIRECTION('',(1.,0.,0.));
#25899=DIRECTION('center_axis',(1.,0.,0.));
#25900=DIRECTION('ref_axis',(0.,-1.17203152359781E-12,-1.));
#25901=DIRECTION('',(1.,0.,0.));
#25902=DIRECTION('center_axis',(1.,0.,0.));
#25903=DIRECTION('ref_axis',(0.,-1.17203152359781E-12,-1.));
#25904=DIRECTION('',(1.,0.,0.));
#25905=DIRECTION('center_axis',(1.,0.,0.));
#25906=DIRECTION('ref_axis',(0.,-1.17203152359781E-12,-1.));
#25907=DIRECTION('',(1.,0.,0.));
#25908=DIRECTION('center_axis',(1.,0.,0.));
#25909=DIRECTION('ref_axis',(0.,-1.17203152359781E-12,-1.));
#25910=DIRECTION('',(1.,0.,0.));
#25911=DIRECTION('center_axis',(1.,0.,0.));
#25912=DIRECTION('ref_axis',(0.,-1.17203152359781E-12,-1.));
#25913=DIRECTION('',(1.,0.,0.));
#25914=DIRECTION('center_axis',(1.,0.,0.));
#25915=DIRECTION('ref_axis',(0.,-1.17203152359781E-12,-1.));
#25916=DIRECTION('',(1.,0.,0.));
#25917=DIRECTION('center_axis',(1.,0.,0.));
#25918=DIRECTION('ref_axis',(0.,-1.17203152359781E-12,-1.));
#25919=DIRECTION('',(1.,0.,0.));
#25920=DIRECTION('center_axis',(1.,0.,0.));
#25921=DIRECTION('ref_axis',(0.,-1.17203152359781E-12,-1.));
#25922=DIRECTION('',(1.,0.,0.));
#25923=DIRECTION('center_axis',(1.,0.,0.));
#25924=DIRECTION('ref_axis',(0.,-1.17203152359781E-12,-1.));
#25925=DIRECTION('',(1.,0.,0.));
#25926=DIRECTION('center_axis',(1.,0.,0.));
#25927=DIRECTION('ref_axis',(0.,-1.17203152359781E-12,-1.));
#25928=DIRECTION('',(1.,0.,0.));
#25929=DIRECTION('center_axis',(1.,0.,0.));
#25930=DIRECTION('ref_axis',(0.,-1.17203152359781E-12,-1.));
#25931=DIRECTION('',(1.,0.,0.));
#25932=DIRECTION('center_axis',(1.,0.,0.));
#25933=DIRECTION('ref_axis',(0.,-1.17203152359781E-12,-1.));
#25934=DIRECTION('',(1.,0.,0.));
#25935=DIRECTION('center_axis',(1.,0.,0.));
#25936=DIRECTION('ref_axis',(0.,-1.17203152359781E-12,-1.));
#25937=DIRECTION('',(1.,0.,0.));
#25938=DIRECTION('center_axis',(1.,0.,0.));
#25939=DIRECTION('ref_axis',(0.,-1.17203152359781E-12,-1.));
#25940=DIRECTION('',(1.,0.,0.));
#25941=DIRECTION('center_axis',(1.,0.,0.));
#25942=DIRECTION('ref_axis',(0.,-1.17203152359781E-12,-1.));
#25943=DIRECTION('',(1.,0.,0.));
#25944=DIRECTION('center_axis',(1.,0.,0.));
#25945=DIRECTION('ref_axis',(0.,-1.17203152359781E-12,-1.));
#25946=DIRECTION('',(1.,0.,0.));
#25947=DIRECTION('center_axis',(1.,0.,0.));
#25948=DIRECTION('ref_axis',(0.,-1.17203152359781E-12,-1.));
#25949=DIRECTION('',(1.,0.,0.));
#25950=DIRECTION('center_axis',(1.,0.,0.));
#25951=DIRECTION('ref_axis',(0.,-1.17203152359781E-12,-1.));
#25952=DIRECTION('',(1.,0.,0.));
#25953=DIRECTION('center_axis',(1.,0.,0.));
#25954=DIRECTION('ref_axis',(0.,-1.17203152359781E-12,-1.));
#25955=DIRECTION('',(1.,0.,0.));
#25956=DIRECTION('center_axis',(1.,0.,0.));
#25957=DIRECTION('ref_axis',(0.,-1.17203152359781E-12,-1.));
#25958=DIRECTION('',(1.,0.,0.));
#25959=DIRECTION('center_axis',(1.,0.,0.));
#25960=DIRECTION('ref_axis',(0.,-1.17203152359781E-12,-1.));
#25961=DIRECTION('',(1.,0.,0.));
#25962=DIRECTION('center_axis',(1.,0.,0.));
#25963=DIRECTION('ref_axis',(0.,-1.17203152359781E-12,-1.));
#25964=DIRECTION('',(1.,0.,0.));
#25965=DIRECTION('center_axis',(1.,0.,0.));
#25966=DIRECTION('ref_axis',(0.,-1.17203152359781E-12,-1.));
#25967=DIRECTION('',(1.,0.,0.));
#25968=DIRECTION('center_axis',(1.,0.,0.));
#25969=DIRECTION('ref_axis',(0.,-1.17203152359781E-12,-1.));
#25970=DIRECTION('',(1.,0.,0.));
#25971=DIRECTION('center_axis',(1.,0.,0.));
#25972=DIRECTION('ref_axis',(0.,-1.17203152359781E-12,-1.));
#25973=DIRECTION('',(1.,0.,0.));
#25974=DIRECTION('center_axis',(1.,0.,0.));
#25975=DIRECTION('ref_axis',(0.,-1.17203152359781E-12,-1.));
#25976=DIRECTION('',(1.,0.,0.));
#25977=DIRECTION('center_axis',(1.,0.,0.));
#25978=DIRECTION('ref_axis',(0.,-1.17203152359781E-12,-1.));
#25979=DIRECTION('',(1.,0.,0.));
#25980=DIRECTION('center_axis',(1.,0.,0.));
#25981=DIRECTION('ref_axis',(0.,-1.17203152359781E-12,-1.));
#25982=DIRECTION('',(1.,0.,0.));
#25983=DIRECTION('center_axis',(1.,0.,0.));
#25984=DIRECTION('ref_axis',(0.,-1.17203152359781E-12,-1.));
#25985=DIRECTION('',(1.,0.,0.));
#25986=DIRECTION('center_axis',(1.,0.,0.));
#25987=DIRECTION('ref_axis',(0.,-1.17203152359781E-12,-1.));
#25988=DIRECTION('',(1.,0.,0.));
#25989=DIRECTION('center_axis',(1.,0.,0.));
#25990=DIRECTION('ref_axis',(0.,-1.17203152359781E-12,-1.));
#25991=DIRECTION('',(1.,0.,0.));
#25992=DIRECTION('center_axis',(1.,0.,0.));
#25993=DIRECTION('ref_axis',(0.,-1.17203152359781E-12,-1.));
#25994=DIRECTION('',(1.,0.,0.));
#25995=DIRECTION('center_axis',(1.,0.,0.));
#25996=DIRECTION('ref_axis',(0.,-1.17203152359781E-12,-1.));
#25997=DIRECTION('',(1.,0.,0.));
#25998=DIRECTION('center_axis',(1.,0.,0.));
#25999=DIRECTION('ref_axis',(0.,-1.17203152359781E-12,-1.));
#26000=DIRECTION('',(1.,0.,0.));
#26001=DIRECTION('center_axis',(1.,0.,0.));
#26002=DIRECTION('ref_axis',(0.,-1.17203152359781E-12,-1.));
#26003=DIRECTION('',(1.,0.,0.));
#26004=DIRECTION('center_axis',(1.,0.,0.));
#26005=DIRECTION('ref_axis',(0.,0.,-1.));
#26006=DIRECTION('center_axis',(1.,0.,0.));
#26007=DIRECTION('ref_axis',(0.,0.,-1.));
#26008=DIRECTION('center_axis',(-1.,0.,0.));
#26009=DIRECTION('ref_axis',(0.,-1.17203152359781E-12,-1.));
#26010=DIRECTION('center_axis',(1.,0.,0.));
#26011=DIRECTION('ref_axis',(0.,0.,-1.));
#26012=DIRECTION('',(-1.,0.,0.));
#26013=DIRECTION('center_axis',(1.,0.,0.));
#26014=DIRECTION('ref_axis',(0.,0.,-1.));
#26015=DIRECTION('center_axis',(1.,0.,0.));
#26016=DIRECTION('ref_axis',(0.,0.,-1.));
#26017=DIRECTION('center_axis',(1.,0.,0.));
#26018=DIRECTION('ref_axis',(0.,-1.17203152359781E-12,-1.));
#26019=DIRECTION('center_axis',(0.,1.,0.));
#26020=DIRECTION('ref_axis',(0.,0.,1.));
#26021=DIRECTION('',(-1.,0.,0.));
#26022=DIRECTION('',(0.,0.,1.));
#26023=DIRECTION('',(1.,0.,0.));
#26024=DIRECTION('',(0.,0.,1.));
#26025=DIRECTION('center_axis',(1.,0.,0.));
#26026=DIRECTION('ref_axis',(0.,0.,-1.));
#26027=DIRECTION('center_axis',(-1.,0.,0.));
#26028=DIRECTION('ref_axis',(0.,0.,-1.));
#26029=DIRECTION('',(0.,-1.,0.));
#26030=DIRECTION('',(0.,0.,-1.));
#26031=DIRECTION('center_axis',(0.,0.,1.));
#26032=DIRECTION('ref_axis',(0.,-1.,0.));
#26033=DIRECTION('',(0.,-1.,0.));
#26034=DIRECTION('',(1.,0.,0.));
#26035=DIRECTION('center_axis',(0.,-1.,0.));
#26036=DIRECTION('ref_axis',(0.,0.,-1.));
#26037=DIRECTION('',(1.,0.,0.));
#26038=DIRECTION('',(0.,0.,-1.));
#26039=DIRECTION('center_axis',(1.,0.,0.));
#26040=DIRECTION('ref_axis',(0.,0.,-1.));
#26041=DIRECTION('center_axis',(1.,0.,0.));
#26042=DIRECTION('ref_axis',(0.,0.,-1.));
#26043=DIRECTION('center_axis',(1.,0.,0.));
#26044=DIRECTION('ref_axis',(0.,0.,-1.));
#26045=DIRECTION('center_axis',(1.,0.,0.));
#26046=DIRECTION('ref_axis',(0.,0.,-1.));
#26047=DIRECTION('',(-1.,0.,0.));
#26048=DIRECTION('center_axis',(-1.,0.,0.));
#26049=DIRECTION('ref_axis',(0.,0.,-1.));
#26050=DIRECTION('center_axis',(1.,0.,0.));
#26051=DIRECTION('ref_axis',(0.,0.,-1.));
#26052=DIRECTION('center_axis',(1.,0.,0.));
#26053=DIRECTION('ref_axis',(0.,0.,-1.));
#26054=DIRECTION('center_axis',(1.,0.,0.));
#26055=DIRECTION('ref_axis',(0.,0.,-1.));
#26056=DIRECTION('center_axis',(-1.,0.,0.));
#26057=DIRECTION('ref_axis',(0.,0.,-1.));
#26058=DIRECTION('center_axis',(1.,0.,0.));
#26059=DIRECTION('ref_axis',(0.,0.,-1.));
#26060=DIRECTION('center_axis',(1.,0.,0.));
#26061=DIRECTION('ref_axis',(0.,0.,-1.));
#26062=DIRECTION('',(-1.,0.,0.));
#26063=DIRECTION('center_axis',(1.,0.,0.));
#26064=DIRECTION('ref_axis',(0.,0.,-1.));
#26065=DIRECTION('center_axis',(1.,0.,0.));
#26066=DIRECTION('ref_axis',(0.,0.,-1.));
#26067=DIRECTION('axis',(0.,0.,1.));
#26068=DIRECTION('refdir',(1.,0.,0.));
#26069=DIRECTION('center_axis',(1.,0.,0.));
#26070=DIRECTION('ref_axis',(0.,0.,-1.));
#26071=DIRECTION('center_axis',(-1.,0.,0.));
#26072=DIRECTION('ref_axis',(0.,0.,-1.));
#26073=DIRECTION('',(-1.,0.,0.));
#26074=DIRECTION('center_axis',(-1.,0.,0.));
#26075=DIRECTION('ref_axis',(0.,0.,-1.));
#26076=DIRECTION('center_axis',(1.,0.,0.));
#26077=DIRECTION('ref_axis',(0.,0.,-1.));
#26078=DIRECTION('center_axis',(1.,0.,0.));
#26079=DIRECTION('ref_axis',(0.,0.,-1.));
#26080=DIRECTION('',(-1.,0.,0.));
#26081=DIRECTION('center_axis',(1.,0.,0.));
#26082=DIRECTION('ref_axis',(0.,0.,-1.));
#26083=DIRECTION('center_axis',(1.,0.,0.));
#26084=DIRECTION('ref_axis',(0.,0.,-1.));
#26085=DIRECTION('center_axis',(1.,0.,0.));
#26086=DIRECTION('ref_axis',(0.,0.,-1.));
#26087=DIRECTION('axis',(0.,0.,1.));
#26088=DIRECTION('refdir',(1.,0.,0.));
#26089=DIRECTION('center_axis',(0.,1.,0.));
#26090=DIRECTION('ref_axis',(1.,0.,0.));
#26091=DIRECTION('',(1.,0.,0.));
#26092=DIRECTION('center_axis',(0.,1.,0.));
#26093=DIRECTION('ref_axis',(1.,0.,0.));
#26094=DIRECTION('center_axis',(0.,1.,0.));
#26095=DIRECTION('ref_axis',(1.,0.,0.));
#26096=DIRECTION('center_axis',(0.,1.,0.));
#26097=DIRECTION('ref_axis',(1.,0.,0.));
#26098=DIRECTION('',(0.,1.,0.));
#26099=DIRECTION('center_axis',(0.,1.,0.));
#26100=DIRECTION('ref_axis',(1.,0.,0.));
#26101=DIRECTION('',(-1.,0.,0.));
#26102=DIRECTION('center_axis',(1.,0.,0.));
#26103=DIRECTION('ref_axis',(0.,0.,-1.));
#26104=DIRECTION('center_axis',(-1.,0.,0.));
#26105=DIRECTION('ref_axis',(0.,0.,-1.));
#26106=DIRECTION('',(-1.,0.,0.));
#26107=DIRECTION('center_axis',(-1.,0.,0.));
#26108=DIRECTION('ref_axis',(0.,0.,-1.));
#26109=DIRECTION('center_axis',(1.,0.,0.));
#26110=DIRECTION('ref_axis',(0.,0.,-1.));
#26111=DIRECTION('center_axis',(1.,0.,0.));
#26112=DIRECTION('ref_axis',(0.,0.,-1.));
#26113=DIRECTION('',(-1.,0.,0.));
#26114=DIRECTION('center_axis',(1.,0.,0.));
#26115=DIRECTION('ref_axis',(0.,0.,-1.));
#26116=DIRECTION('center_axis',(1.,0.,0.));
#26117=DIRECTION('ref_axis',(0.,0.,-1.));
#26118=DIRECTION('center_axis',(1.,0.,0.));
#26119=DIRECTION('ref_axis',(0.,0.,-1.));
#26120=DIRECTION('axis',(0.,0.,1.));
#26121=DIRECTION('refdir',(1.,0.,0.));
#26122=DIRECTION('center_axis',(1.,0.,0.));
#26123=DIRECTION('ref_axis',(0.,0.,-1.));
#26124=DIRECTION('center_axis',(1.,0.,0.));
#26125=DIRECTION('ref_axis',(0.,0.,-1.));
#26126=DIRECTION('',(1.,0.,0.));
#26127=DIRECTION('center_axis',(-1.,0.,0.));
#26128=DIRECTION('ref_axis',(0.,0.,-1.));
#26129=DIRECTION('center_axis',(0.,1.,0.));
#26130=DIRECTION('ref_axis',(1.,0.,0.));
#26131=DIRECTION('',(1.,0.,0.));
#26132=DIRECTION('center_axis',(0.,1.,0.));
#26133=DIRECTION('ref_axis',(1.,0.,0.));
#26134=DIRECTION('center_axis',(0.,1.,0.));
#26135=DIRECTION('ref_axis',(1.,0.,0.));
#26136=DIRECTION('center_axis',(0.,1.,0.));
#26137=DIRECTION('ref_axis',(1.,0.,0.));
#26138=DIRECTION('',(0.,1.,0.));
#26139=DIRECTION('center_axis',(0.,1.,0.));
#26140=DIRECTION('ref_axis',(1.,0.,0.));
#26141=DIRECTION('',(-1.,0.,0.));
#26142=DIRECTION('center_axis',(0.,-1.,0.));
#26143=DIRECTION('ref_axis',(0.,0.,-1.));
#26144=DIRECTION('',(0.,0.,1.));
#26145=DIRECTION('',(1.,0.,0.));
#26146=DIRECTION('',(0.,0.,-1.));
#26147=DIRECTION('',(1.,0.,0.));
#26148=DIRECTION('',(0.,0.,-1.));
#26149=DIRECTION('',(-1.,0.,0.));
#26150=DIRECTION('center_axis',(0.,0.,-1.));
#26151=DIRECTION('ref_axis',(0.,1.,0.));
#26152=DIRECTION('',(0.,-1.,0.));
#26153=DIRECTION('',(1.,0.,0.));
#26154=DIRECTION('',(0.,1.,0.));
#26155=DIRECTION('center_axis',(0.,1.,0.));
#26156=DIRECTION('ref_axis',(0.,0.,1.));
#26157=DIRECTION('',(0.,0.,-1.));
#26158=DIRECTION('',(1.,0.,0.));
#26159=DIRECTION('',(0.,0.,1.));
#26160=DIRECTION('',(-1.,0.,0.));
#26161=DIRECTION('',(0.,0.,1.));
#26162=DIRECTION('center_axis',(1.,0.,0.));
#26163=DIRECTION('ref_axis',(0.,0.,-1.));
#26164=DIRECTION('center_axis',(1.,0.,0.));
#26165=DIRECTION('ref_axis',(0.,0.,-1.));
#26166=DIRECTION('center_axis',(-1.,0.,0.));
#26167=DIRECTION('ref_axis',(0.,0.,-1.));
#26168=DIRECTION('center_axis',(1.,0.,0.));
#26169=DIRECTION('ref_axis',(0.,0.,-1.));
#26170=DIRECTION('center_axis',(1.,0.,0.));
#26171=DIRECTION('ref_axis',(0.,0.,-1.));
#26172=DIRECTION('center_axis',(1.,0.,0.));
#26173=DIRECTION('ref_axis',(0.,0.,-1.));
#26174=DIRECTION('center_axis',(1.,0.,0.));
#26175=DIRECTION('ref_axis',(0.,0.,-1.));
#26176=DIRECTION('',(-1.,0.,0.));
#26177=DIRECTION('center_axis',(1.,0.,0.));
#26178=DIRECTION('ref_axis',(0.,1.22464679914735E-16,1.));
#26179=DIRECTION('center_axis',(-1.,0.,0.));
#26180=DIRECTION('ref_axis',(0.,0.,-1.));
#26181=DIRECTION('center_axis',(1.,0.,0.));
#26182=DIRECTION('ref_axis',(0.,1.22464679914735E-16,1.));
#26183=DIRECTION('center_axis',(1.,0.,0.));
#26184=DIRECTION('ref_axis',(0.,0.,-1.));
#26185=DIRECTION('center_axis',(1.,0.,0.));
#26186=DIRECTION('ref_axis',(0.,0.,-1.));
#26187=DIRECTION('axis',(0.,0.,1.));
#26188=DIRECTION('refdir',(1.,0.,0.));
#26189=DIRECTION('center_axis',(1.,0.,0.));
#26190=DIRECTION('ref_axis',(0.,0.,-1.));
#26191=DIRECTION('center_axis',(-1.,0.,0.));
#26192=DIRECTION('ref_axis',(0.,0.,-1.));
#26193=DIRECTION('',(-1.,0.,0.));
#26194=DIRECTION('center_axis',(-1.,0.,0.));
#26195=DIRECTION('ref_axis',(0.,0.,-1.));
#26196=DIRECTION('center_axis',(1.,0.,0.));
#26197=DIRECTION('ref_axis',(0.,0.,-1.));
#26198=DIRECTION('center_axis',(1.,0.,0.));
#26199=DIRECTION('ref_axis',(0.,0.,-1.));
#26200=DIRECTION('',(-1.,0.,0.));
#26201=DIRECTION('center_axis',(1.,0.,0.));
#26202=DIRECTION('ref_axis',(0.,0.,-1.));
#26203=DIRECTION('center_axis',(1.,0.,0.));
#26204=DIRECTION('ref_axis',(0.,0.,-1.));
#26205=DIRECTION('center_axis',(1.,0.,0.));
#26206=DIRECTION('ref_axis',(0.,0.,-1.));
#26207=DIRECTION('axis',(0.,0.,1.));
#26208=DIRECTION('refdir',(1.,0.,0.));
#26209=DIRECTION('center_axis',(1.,0.,0.));
#26210=DIRECTION('ref_axis',(0.,0.,-1.));
#26211=DIRECTION('center_axis',(-1.,0.,0.));
#26212=DIRECTION('ref_axis',(0.,0.,-1.));
#26213=DIRECTION('',(-1.,0.,0.));
#26214=DIRECTION('center_axis',(-1.,0.,0.));
#26215=DIRECTION('ref_axis',(0.,0.,-1.));
#26216=DIRECTION('center_axis',(1.,0.,0.));
#26217=DIRECTION('ref_axis',(0.,0.,-1.));
#26218=DIRECTION('center_axis',(1.,0.,0.));
#26219=DIRECTION('ref_axis',(0.,0.,-1.));
#26220=DIRECTION('',(-1.,0.,0.));
#26221=DIRECTION('center_axis',(1.,0.,0.));
#26222=DIRECTION('ref_axis',(0.,0.,-1.));
#26223=DIRECTION('center_axis',(1.,0.,0.));
#26224=DIRECTION('ref_axis',(0.,0.,-1.));
#26225=DIRECTION('center_axis',(1.,0.,0.));
#26226=DIRECTION('ref_axis',(0.,0.,-1.));
#26227=DIRECTION('axis',(0.,0.,1.));
#26228=DIRECTION('refdir',(1.,0.,0.));
#26229=DIRECTION('center_axis',(1.,0.,0.));
#26230=DIRECTION('ref_axis',(0.,0.,-1.));
#26231=DIRECTION('',(0.,-0.707106781186547,-0.707106781186548));
#26232=DIRECTION('',(0.,-1.,0.));
#26233=DIRECTION('',(0.,-0.707106781186547,0.707106781186548));
#26234=DIRECTION('',(0.,0.,1.));
#26235=DIRECTION('',(0.,0.707106781186547,0.707106781186548));
#26236=DIRECTION('',(0.,1.,0.));
#26237=DIRECTION('',(0.,0.707106781186547,-0.707106781186548));
#26238=DIRECTION('',(0.,0.,-1.));
#26239=DIRECTION('center_axis',(0.,0.707106781186548,-0.707106781186547));
#26240=DIRECTION('ref_axis',(-1.,0.,0.));
#26241=DIRECTION('',(1.,0.,0.));
#26242=DIRECTION('',(0.,-0.707106781186547,-0.707106781186548));
#26243=DIRECTION('',(-1.,0.,0.));
#26244=DIRECTION('center_axis',(0.,1.,0.));
#26245=DIRECTION('ref_axis',(-1.,0.,0.));
#26246=DIRECTION('',(-1.,0.,0.));
#26247=DIRECTION('',(0.,0.,-1.));
#26248=DIRECTION('center_axis',(0.,0.707106781186548,0.707106781186547));
#26249=DIRECTION('ref_axis',(1.,0.,0.));
#26250=DIRECTION('',(1.,0.,0.));
#26251=DIRECTION('',(0.,0.707106781186547,-0.707106781186548));
#26252=DIRECTION('center_axis',(0.,0.,1.));
#26253=DIRECTION('ref_axis',(1.,0.,0.));
#26254=DIRECTION('',(-1.,0.,0.));
#26255=DIRECTION('',(0.,1.,0.));
#26256=DIRECTION('center_axis',(1.,0.,0.));
#26257=DIRECTION('ref_axis',(0.,0.,-1.));
#26258=DIRECTION('',(0.,-0.707106781186547,0.707106781186548));
#26259=DIRECTION('',(0.,-1.,0.));
#26260=DIRECTION('',(0.,0.707106781186547,0.707106781186548));
#26261=DIRECTION('',(0.,0.,1.));
#26262=DIRECTION('center_axis',(0.,0.,1.));
#26263=DIRECTION('ref_axis',(1.,0.,0.));
#26264=DIRECTION('',(1.,0.,0.));
#26265=DIRECTION('center_axis',(0.,-0.707106781186548,0.707106781186547));
#26266=DIRECTION('ref_axis',(1.,0.,0.));
#26267=DIRECTION('',(1.,0.,0.));
#26268=DIRECTION('center_axis',(0.,-0.707106781186548,-0.707106781186547));
#26269=DIRECTION('ref_axis',(-1.,0.,0.));
#26270=DIRECTION('',(-1.,0.,0.));
#26271=DIRECTION('center_axis',(0.,-1.,0.));
#26272=DIRECTION('ref_axis',(1.,0.,0.));
#26273=DIRECTION('axis',(0.,0.,1.));
#26274=DIRECTION('refdir',(1.,0.,0.));
#26275=DIRECTION('center_axis',(0.866025403784439,0.,-0.5));
#26276=DIRECTION('ref_axis',(0.5,0.,0.866025403784439));
#26277=DIRECTION('',(0.5,0.,0.866025403784439));
#26278=DIRECTION('',(0.,-1.,0.));
#26279=DIRECTION('',(0.5,0.,0.866025403784439));
#26280=DIRECTION('',(0.,-1.,0.));
#26281=DIRECTION('center_axis',(1.92296268638356E-16,0.,-1.));
#26282=DIRECTION('ref_axis',(1.,0.,1.92296268638356E-16));
#26283=DIRECTION('',(1.,0.,1.92296268638356E-16));
#26284=DIRECTION('',(0.,-1.,0.));
#26285=DIRECTION('',(1.,0.,1.92296268638356E-16));
#26286=DIRECTION('center_axis',(-0.866025403784439,0.,-0.5));
#26287=DIRECTION('ref_axis',(0.5,0.,-0.866025403784439));
#26288=DIRECTION('',(0.5,0.,-0.866025403784439));
#26289=DIRECTION('',(0.,-1.,0.));
#26290=DIRECTION('',(0.5,0.,-0.866025403784438));
#26291=DIRECTION('center_axis',(-0.866025403784439,0.,0.5));
#26292=DIRECTION('ref_axis',(-0.5,0.,-0.866025403784439));
#26293=DIRECTION('',(-0.5,0.,-0.866025403784439));
#26294=DIRECTION('',(0.,-1.,0.));
#26295=DIRECTION('',(-0.5,0.,-0.866025403784439));
#26296=DIRECTION('center_axis',(-1.92296268638356E-16,0.,1.));
#26297=DIRECTION('ref_axis',(-1.,0.,-1.92296268638356E-16));
#26298=DIRECTION('',(-1.,0.,-1.92296268638356E-16));
#26299=DIRECTION('',(0.,-1.,0.));
#26300=DIRECTION('',(-1.,0.,-1.92296268638356E-16));
#26301=DIRECTION('center_axis',(0.866025403784439,0.,0.5));
#26302=DIRECTION('ref_axis',(-0.5,0.,0.866025403784439));
#26303=DIRECTION('',(-0.5,0.,0.866025403784439));
#26304=DIRECTION('',(-0.5,0.,0.866025403784439));
#26305=DIRECTION('center_axis',(0.,-1.,0.));
#26306=DIRECTION('ref_axis',(0.,0.,-1.));
#26307=DIRECTION('center_axis',(0.,1.,0.));
#26308=DIRECTION('ref_axis',(0.,0.,1.));
#26309=DIRECTION('center_axis',(0.,-1.,0.));
#26310=DIRECTION('ref_axis',(1.,0.,0.));
#26311=DIRECTION('center_axis',(0.,-1.,0.));
#26312=DIRECTION('ref_axis',(1.,0.,0.));
#26313=DIRECTION('center_axis',(0.,-1.,0.));
#26314=DIRECTION('ref_axis',(1.,0.,0.));
#26315=DIRECTION('',(0.707106781186547,0.707106781186548,8.65956056235493E-17));
#26316=DIRECTION('center_axis',(0.,-1.,0.));
#26317=DIRECTION('ref_axis',(1.,0.,0.));
#26318=DIRECTION('center_axis',(0.,1.,0.));
#26319=DIRECTION('ref_axis',(1.,0.,0.));
#26320=DIRECTION('',(0.,1.,0.));
#26321=DIRECTION('center_axis',(0.,1.,0.));
#26322=DIRECTION('ref_axis',(1.,0.,0.));
#26323=DIRECTION('center_axis',(0.,-1.,0.));
#26324=DIRECTION('ref_axis',(1.,0.,0.));
#26325=DIRECTION('',(-0.707106781186547,0.707106781186548,-8.65956056235493E-17));
#26326=DIRECTION('center_axis',(0.,-1.,0.));
#26327=DIRECTION('ref_axis',(0.,0.,-1.));
#26328=DIRECTION('axis',(0.,0.,1.));
#26329=DIRECTION('refdir',(1.,0.,0.));
#26330=DIRECTION('center_axis',(0.,1.,0.));
#26331=DIRECTION('ref_axis',(1.,0.,0.));
#26332=DIRECTION('center_axis',(0.,-1.,0.));
#26333=DIRECTION('ref_axis',(1.,0.,0.));
#26334=DIRECTION('',(0.,-1.,0.));
#26335=DIRECTION('center_axis',(0.,-1.,0.));
#26336=DIRECTION('ref_axis',(1.,0.,0.));
#26337=DIRECTION('center_axis',(0.,1.,0.));
#26338=DIRECTION('ref_axis',(1.,0.,0.));
#26339=DIRECTION('center_axis',(0.,1.,0.));
#26340=DIRECTION('ref_axis',(1.,0.,0.));
#26341=DIRECTION('',(0.,-1.,0.));
#26342=DIRECTION('center_axis',(0.,1.,0.));
#26343=DIRECTION('ref_axis',(1.,0.,0.));
#26344=DIRECTION('center_axis',(0.,1.,0.));
#26345=DIRECTION('ref_axis',(1.,0.,0.));
#26346=DIRECTION('center_axis',(0.,1.,0.));
#26347=DIRECTION('ref_axis',(1.,0.,0.));
#26348=DIRECTION('axis',(0.,0.,1.));
#26349=DIRECTION('refdir',(1.,0.,0.));
#26350=DIRECTION('center_axis',(0.,1.,0.));
#26351=DIRECTION('ref_axis',(0.,0.,1.));
#26352=DIRECTION('center_axis',(0.,-1.,0.));
#26353=DIRECTION('ref_axis',(1.,0.,0.));
#26354=DIRECTION('center_axis',(0.,-1.,0.));
#26355=DIRECTION('ref_axis',(1.,0.,0.));
#26356=DIRECTION('center_axis',(0.,-1.,0.));
#26357=DIRECTION('ref_axis',(1.,0.,0.));
#26358=DIRECTION('',(0.707106781186548,0.707106781186547,8.65956056235494E-17));
#26359=DIRECTION('center_axis',(0.,-1.,0.));
#26360=DIRECTION('ref_axis',(1.,0.,0.));
#26361=DIRECTION('center_axis',(0.,-1.,0.));
#26362=DIRECTION('ref_axis',(1.,0.,0.));
#26363=DIRECTION('',(0.,1.,0.));
#26364=DIRECTION('center_axis',(0.,1.,0.));
#26365=DIRECTION('ref_axis',(1.,0.,0.));
#26366=DIRECTION('center_axis',(0.,-1.,0.));
#26367=DIRECTION('ref_axis',(1.,0.,0.));
#26368=DIRECTION('',(-0.707106781186547,0.707106781186548,-8.65956056235493E-17));
#26369=DIRECTION('center_axis',(0.,-1.,0.));
#26370=DIRECTION('ref_axis',(0.,0.,-1.));
#26371=DIRECTION('center_axis',(0.,-1.,0.));
#26372=DIRECTION('ref_axis',(1.,0.,0.));
#26373=DIRECTION('center_axis',(0.,1.,0.));
#26374=DIRECTION('ref_axis',(1.,0.,0.));
#26375=DIRECTION('center_axis',(0.,1.,0.));
#26376=DIRECTION('ref_axis',(1.,0.,0.));
#26377=DIRECTION('',(-0.447213595499958,0.894427190999916,-5.47678698264203E-17));
#26378=DIRECTION('center_axis',(0.,-1.,0.));
#26379=DIRECTION('ref_axis',(1.,0.,0.));
#26380=DIRECTION('center_axis',(0.,1.,0.));
#26381=DIRECTION('ref_axis',(1.,0.,0.));
#26382=DIRECTION('',(0.,1.,0.));
#26383=DIRECTION('center_axis',(0.,1.,0.));
#26384=DIRECTION('ref_axis',(1.,0.,0.));
#26385=DIRECTION('center_axis',(0.,-1.,0.));
#26386=DIRECTION('ref_axis',(1.,0.,0.));
#26387=DIRECTION('',(-0.707106781186547,0.707106781186548,-8.65956056235493E-17));
#26388=DIRECTION('center_axis',(0.,-1.,0.));
#26389=DIRECTION('ref_axis',(0.,0.,-1.));
#26390=DIRECTION('center_axis',(0.866025403784439,0.,-0.5));
#26391=DIRECTION('ref_axis',(0.5,0.,0.866025403784439));
#26392=DIRECTION('',(-0.5,0.,-0.866025403784439));
#26393=DIRECTION('',(0.,-1.,0.));
#26394=DIRECTION('',(0.5,0.,0.866025403784439));
#26395=DIRECTION('',(0.,-1.,0.));
#26396=DIRECTION('center_axis',(1.92296268638356E-16,0.,-1.));
#26397=DIRECTION('ref_axis',(1.,0.,1.92296268638356E-16));
#26398=DIRECTION('',(-1.,0.,-1.92296268638356E-16));
#26399=DIRECTION('',(0.,-1.,0.));
#26400=DIRECTION('',(1.,0.,1.92296268638356E-16));
#26401=DIRECTION('center_axis',(-0.866025403784439,0.,-0.5));
#26402=DIRECTION('ref_axis',(0.5,0.,-0.866025403784439));
#26403=DIRECTION('',(-0.5,0.,0.866025403784438));
#26404=DIRECTION('',(0.,-1.,0.));
#26405=DIRECTION('',(0.5,0.,-0.866025403784438));
#26406=DIRECTION('center_axis',(-0.866025403784439,0.,0.5));
#26407=DIRECTION('ref_axis',(-0.5,0.,-0.866025403784439));
#26408=DIRECTION('',(0.5,0.,0.866025403784439));
#26409=DIRECTION('',(0.,-1.,0.));
#26410=DIRECTION('',(-0.5,0.,-0.866025403784439));
#26411=DIRECTION('center_axis',(-1.92296268638356E-16,0.,1.));
#26412=DIRECTION('ref_axis',(-1.,0.,-1.92296268638356E-16));
#26413=DIRECTION('',(1.,0.,1.92296268638356E-16));
#26414=DIRECTION('',(0.,-1.,0.));
#26415=DIRECTION('',(-1.,0.,-1.92296268638356E-16));
#26416=DIRECTION('center_axis',(0.866025403784439,0.,0.5));
#26417=DIRECTION('ref_axis',(-0.5,0.,0.866025403784439));
#26418=DIRECTION('',(0.5,0.,-0.866025403784439));
#26419=DIRECTION('',(-0.5,0.,0.866025403784439));
#26420=DIRECTION('center_axis',(0.,1.,0.));
#26421=DIRECTION('ref_axis',(1.,0.,0.));
#26422=DIRECTION('center_axis',(0.,-1.,0.));
#26423=DIRECTION('ref_axis',(0.,0.,-1.));
#26424=DIRECTION('',(0.,0.,1.));
#26425=DIRECTION('',(1.,0.,0.));
#26426=DIRECTION('',(0.,0.,1.));
#26427=DIRECTION('',(1.,0.,0.));
#26428=DIRECTION('',(0.,0.,1.));
#26429=DIRECTION('',(1.,0.,0.));
#26430=DIRECTION('',(0.,0.,1.));
#26431=DIRECTION('',(1.,0.,0.));
#26432=DIRECTION('',(0.,0.,1.));
#26433=DIRECTION('',(1.,0.,0.));
#26434=DIRECTION('',(0.,0.,1.));
#26435=DIRECTION('',(1.,0.,0.));
#26436=DIRECTION('',(0.,-1.22464679914735E-16,-1.));
#26437=DIRECTION('',(1.,0.,0.));
#26438=DIRECTION('',(0.,0.,1.));
#26439=DIRECTION('',(1.,0.,0.));
#26440=DIRECTION('',(0.,0.,1.));
#26441=DIRECTION('',(1.,0.,0.));
#26442=DIRECTION('',(0.,0.,1.));
#26443=DIRECTION('',(2.22044604925031E-16,-1.,0.));
#26444=DIRECTION('',(0.,0.,1.));
#26445=DIRECTION('',(2.22044604925031E-16,-1.,0.));
#26446=DIRECTION('',(0.,0.,1.));
#26447=DIRECTION('',(1.,0.,0.));
#26448=DIRECTION('',(0.,0.,1.));
#26449=DIRECTION('',(1.,0.,0.));
#26450=DIRECTION('',(0.5,0.866025403784439,0.));
#26451=DIRECTION('',(0.,0.,1.));
#26452=CARTESIAN_POINT('',(0.,0.,0.));
#26453=CARTESIAN_POINT('',(0.,0.,0.));
#26454=CARTESIAN_POINT('',(0.,0.,0.));
#26455=CARTESIAN_POINT('Origin',(10.,0.,-1.3));
#26456=CARTESIAN_POINT('',(9.725,-3.36777869765523E-17,-1.2));
#26457=CARTESIAN_POINT('Origin',(10.,0.,-1.2));
#26458=CARTESIAN_POINT('',(9.725,3.36777869765523E-17,0.));
#26459=CARTESIAN_POINT('',(9.725,-3.36777869765523E-17,-1.3));
#26460=CARTESIAN_POINT('Origin',(10.,0.,0.));
#26461=CARTESIAN_POINT('Origin',(10.,2.,-0.6));
#26462=CARTESIAN_POINT('',(9.,2.,0.));
#26463=CARTESIAN_POINT('',(9.,2.,-1.2));
#26464=CARTESIAN_POINT('',(9.,2.,-0.9));
#26465=CARTESIAN_POINT('',(12.,2.,0.));
#26466=CARTESIAN_POINT('',(12.,2.,0.));
#26467=CARTESIAN_POINT('',(12.,2.,-1.2));
#26468=CARTESIAN_POINT('',(12.,2.,-1.2));
#26469=CARTESIAN_POINT('',(8.,2.,-1.2));
#26470=CARTESIAN_POINT('Origin',(12.,-2.,0.));
#26471=CARTESIAN_POINT('',(12.,-2.,-1.2));
#26472=CARTESIAN_POINT('',(12.,-2.,0.));
#26473=CARTESIAN_POINT('',(12.,-2.,-1.2));
#26474=CARTESIAN_POINT('',(12.,-2.,-1.2));
#26475=CARTESIAN_POINT('',(12.,-2.,0.));
#26476=CARTESIAN_POINT('Origin',(10.,-2.,-0.6));
#26477=CARTESIAN_POINT('',(9.,-2.,-1.2));
#26478=CARTESIAN_POINT('',(9.,-2.,0.));
#26479=CARTESIAN_POINT('',(9.,-2.,-0.9));
#26480=CARTESIAN_POINT('',(8.,-2.,-1.2));
#26481=CARTESIAN_POINT('',(12.,-2.,0.));
#26482=CARTESIAN_POINT('Origin',(9.,-4.5,-1.2));
#26483=CARTESIAN_POINT('',(9.,12.5,-1.2));
#26484=CARTESIAN_POINT('',(9.,-4.5,-1.2));
#26485=CARTESIAN_POINT('',(9.,12.5,0.));
#26486=CARTESIAN_POINT('',(9.,12.5,-1.2));
#26487=CARTESIAN_POINT('',(9.,-4.5,0.));
#26488=CARTESIAN_POINT('Origin',(9.,-4.5,-1.2));
#26489=CARTESIAN_POINT('',(9.,-4.5,0.));
#26490=CARTESIAN_POINT('',(9.,-4.5,0.));
#26491=CARTESIAN_POINT('',(9.,-4.5,-1.2));
#26492=CARTESIAN_POINT('',(9.,-4.5,-1.2));
#26493=CARTESIAN_POINT('',(9.,-4.5,-1.2));
#26494=CARTESIAN_POINT('Origin',(-2.5,-1.5,-1.1));
#26495=CARTESIAN_POINT('',(-2.665,-1.5,-1.1));
#26496=CARTESIAN_POINT('Origin',(-2.5,-1.5,-1.1));
#26497=CARTESIAN_POINT('',(-2.665,-1.5,0.));
#26498=CARTESIAN_POINT('',(-2.665,-1.5,-1.1));
#26499=CARTESIAN_POINT('Origin',(-2.5,-1.5,0.));
#26500=CARTESIAN_POINT('Origin',(-2.5,-1.5,-1.1));
#26501=CARTESIAN_POINT('Origin',(1.53080849893419E-16,1.,-1.1));
#26502=CARTESIAN_POINT('',(-0.165,1.,-1.1));
#26503=CARTESIAN_POINT('Origin',(1.53080849893419E-16,1.,-1.1));
#26504=CARTESIAN_POINT('',(-0.165,1.,0.));
#26505=CARTESIAN_POINT('',(-0.165,1.,-1.1));
#26506=CARTESIAN_POINT('Origin',(1.53080849893419E-16,1.,0.));
#26507=CARTESIAN_POINT('Origin',(1.66533453693773E-16,1.,-1.1));
#26508=CARTESIAN_POINT('Origin',(2.5,-1.5,-1.1));
#26509=CARTESIAN_POINT('',(2.335,-1.5,-1.1));
#26510=CARTESIAN_POINT('Origin',(2.5,-1.5,-1.1));
#26511=CARTESIAN_POINT('',(2.335,-1.5,0.));
#26512=CARTESIAN_POINT('',(2.335,-1.5,-1.1));
#26513=CARTESIAN_POINT('Origin',(2.5,-1.5,0.));
#26514=CARTESIAN_POINT('Origin',(2.5,-1.5,-1.1));
#26515=CARTESIAN_POINT('Origin',(-4.59242549680257E-16,-4.,-1.1));
#26516=CARTESIAN_POINT('',(-0.165,-4.,-1.1));
#26517=CARTESIAN_POINT('Origin',(-4.59242549680257E-16,-4.,-1.1));
#26518=CARTESIAN_POINT('',(-0.165,-4.,0.));
#26519=CARTESIAN_POINT('',(-0.165,-4.,-1.1));
#26520=CARTESIAN_POINT('Origin',(-4.59242549680257E-16,-4.,0.));
#26521=CARTESIAN_POINT('Origin',(-4.71844785465692E-16,-4.,-1.1));
#26522=CARTESIAN_POINT('Origin',(6.,5.,-1.3));
#26523=CARTESIAN_POINT('',(5.725,5.,-1.2));
#26524=CARTESIAN_POINT('Origin',(6.,5.,-1.2));
#26525=CARTESIAN_POINT('',(5.725,5.,0.));
#26526=CARTESIAN_POINT('',(5.725,5.,-1.3));
#26527=CARTESIAN_POINT('Origin',(6.,5.,0.));
#26528=CARTESIAN_POINT('Origin',(-6.,5.,-1.3));
#26529=CARTESIAN_POINT('',(-6.275,5.,-1.2));
#26530=CARTESIAN_POINT('Origin',(-6.,5.,-1.2));
#26531=CARTESIAN_POINT('',(-6.275,5.,0.));
#26532=CARTESIAN_POINT('',(-6.275,5.,-1.3));
#26533=CARTESIAN_POINT('Origin',(-6.,5.,0.));
#26534=CARTESIAN_POINT('Origin',(2.5,2.5,-1.3));
#26535=CARTESIAN_POINT('',(2.225,2.5,-1.2));
#26536=CARTESIAN_POINT('Origin',(2.5,2.5,-1.2));
#26537=CARTESIAN_POINT('',(2.225,2.5,0.));
#26538=CARTESIAN_POINT('',(2.225,2.5,-1.3));
#26539=CARTESIAN_POINT('Origin',(2.5,2.5,0.));
#26540=CARTESIAN_POINT('Origin',(-2.5,7.5,-1.3));
#26541=CARTESIAN_POINT('',(-2.775,7.5,-1.2));
#26542=CARTESIAN_POINT('Origin',(-2.5,7.5,-1.2));
#26543=CARTESIAN_POINT('',(-2.775,7.5,0.));
#26544=CARTESIAN_POINT('',(-2.775,7.5,-1.3));
#26545=CARTESIAN_POINT('Origin',(-2.5,7.5,0.));
#26546=CARTESIAN_POINT('Origin',(-2.5,2.5,-1.3));
#26547=CARTESIAN_POINT('',(-2.775,2.5,-1.2));
#26548=CARTESIAN_POINT('Origin',(-2.5,2.5,-1.2));
#26549=CARTESIAN_POINT('',(-2.775,2.5,0.));
#26550=CARTESIAN_POINT('',(-2.775,2.5,-1.3));
#26551=CARTESIAN_POINT('Origin',(-2.5,2.5,0.));
#26552=CARTESIAN_POINT('Origin',(2.5,7.5,-1.3));
#26553=CARTESIAN_POINT('',(2.225,7.5,-1.2));
#26554=CARTESIAN_POINT('Origin',(2.5,7.5,-1.2));
#26555=CARTESIAN_POINT('',(2.225,7.5,0.));
#26556=CARTESIAN_POINT('',(2.225,7.5,-1.3));
#26557=CARTESIAN_POINT('Origin',(2.5,7.5,0.));
#26558=CARTESIAN_POINT('Origin',(0.,5.,-1.3));
#26559=CARTESIAN_POINT('',(-2.5,5.,-1.2));
#26560=CARTESIAN_POINT('Origin',(0.,5.,-1.2));
#26561=CARTESIAN_POINT('',(-2.5,5.,0.));
#26562=CARTESIAN_POINT('',(-2.5,5.,-1.3));
#26563=CARTESIAN_POINT('Origin',(0.,5.,0.));
#26564=CARTESIAN_POINT('Origin',(4.4,2.7,-1.3));
#26565=CARTESIAN_POINT('',(4.125,2.7,-1.2));
#26566=CARTESIAN_POINT('Origin',(4.4,2.7,-1.2));
#26567=CARTESIAN_POINT('',(4.125,2.7,0.));
#26568=CARTESIAN_POINT('',(4.125,2.7,-1.3));
#26569=CARTESIAN_POINT('Origin',(4.4,2.7,0.));
#26570=CARTESIAN_POINT('Origin',(7.6,2.7,-1.3));
#26571=CARTESIAN_POINT('',(7.325,2.7,-1.2));
#26572=CARTESIAN_POINT('Origin',(7.6,2.7,-1.2));
#26573=CARTESIAN_POINT('',(7.325,2.7,0.));
#26574=CARTESIAN_POINT('',(7.325,2.7,-1.3));
#26575=CARTESIAN_POINT('Origin',(7.6,2.7,0.));
#26576=CARTESIAN_POINT('Origin',(-7.6,2.7,-1.3));
#26577=CARTESIAN_POINT('',(-7.875,2.7,-1.2));
#26578=CARTESIAN_POINT('Origin',(-7.6,2.7,-1.2));
#26579=CARTESIAN_POINT('',(-7.875,2.7,0.));
#26580=CARTESIAN_POINT('',(-7.875,2.7,-1.3));
#26581=CARTESIAN_POINT('Origin',(-7.6,2.7,0.));
#26582=CARTESIAN_POINT('Origin',(-4.4,2.7,-1.3));
#26583=CARTESIAN_POINT('',(-4.675,2.7,-1.2));
#26584=CARTESIAN_POINT('Origin',(-4.4,2.7,-1.2));
#26585=CARTESIAN_POINT('',(-4.675,2.7,0.));
#26586=CARTESIAN_POINT('',(-4.675,2.7,-1.3));
#26587=CARTESIAN_POINT('Origin',(-4.4,2.7,0.));
#26588=CARTESIAN_POINT('Origin',(7.,9.5,-1.3));
#26589=CARTESIAN_POINT('',(6.725,9.5,-1.2));
#26590=CARTESIAN_POINT('Origin',(7.,9.5,-1.2));
#26591=CARTESIAN_POINT('',(6.725,9.5,0.));
#26592=CARTESIAN_POINT('',(6.725,9.5,-1.3));
#26593=CARTESIAN_POINT('Origin',(7.,9.5,0.));
#26594=CARTESIAN_POINT('Origin',(7.,10.5,-1.3));
#26595=CARTESIAN_POINT('',(6.725,10.5,-1.2));
#26596=CARTESIAN_POINT('Origin',(7.,10.5,-1.2));
#26597=CARTESIAN_POINT('',(6.725,10.5,0.));
#26598=CARTESIAN_POINT('',(6.725,10.5,-1.3));
#26599=CARTESIAN_POINT('Origin',(7.,10.5,0.));
#26600=CARTESIAN_POINT('Origin',(-7.,9.5,-1.3));
#26601=CARTESIAN_POINT('',(-7.275,9.5,-1.2));
#26602=CARTESIAN_POINT('Origin',(-7.,9.5,-1.2));
#26603=CARTESIAN_POINT('',(-7.275,9.5,0.));
#26604=CARTESIAN_POINT('',(-7.275,9.5,-1.3));
#26605=CARTESIAN_POINT('Origin',(-7.,9.5,0.));
#26606=CARTESIAN_POINT('Origin',(-7.,10.5,-1.3));
#26607=CARTESIAN_POINT('',(-7.275,10.5,-1.2));
#26608=CARTESIAN_POINT('Origin',(-7.,10.5,-1.2));
#26609=CARTESIAN_POINT('',(-7.275,10.5,0.));
#26610=CARTESIAN_POINT('',(-7.275,10.5,-1.3));
#26611=CARTESIAN_POINT('Origin',(-7.,10.5,0.));
#26612=CARTESIAN_POINT('Origin',(9.,12.5,-1.2));
#26613=CARTESIAN_POINT('',(-9.,12.5,-1.2));
#26614=CARTESIAN_POINT('',(9.,12.5,-1.2));
#26615=CARTESIAN_POINT('',(-9.,12.5,0.));
#26616=CARTESIAN_POINT('',(-9.,12.5,-1.2));
#26617=CARTESIAN_POINT('',(9.,12.5,0.));
#26618=CARTESIAN_POINT('Origin',(-9.,-4.5,-1.2));
#26619=CARTESIAN_POINT('',(-9.,-4.5,-1.2));
#26620=CARTESIAN_POINT('',(-9.,-4.5,-1.2));
#26621=CARTESIAN_POINT('',(-9.,-4.5,0.));
#26622=CARTESIAN_POINT('',(-9.,-4.5,0.));
#26623=CARTESIAN_POINT('',(-9.,-4.5,-1.2));
#26624=CARTESIAN_POINT('Origin',(-9.,12.5,-1.2));
#26625=CARTESIAN_POINT('',(-9.,12.5,-1.2));
#26626=CARTESIAN_POINT('',(-9.,12.5,0.));
#26627=CARTESIAN_POINT('Origin',(0.,4.,0.));
#26628=CARTESIAN_POINT('Origin',(0.,4.,-1.2));
#26629=CARTESIAN_POINT('',(0.,0.,0.));
#26630=CARTESIAN_POINT('Origin',(9.,-3.,-2.2));
#26631=CARTESIAN_POINT('',(9.,-3.,-2.2));
#26632=CARTESIAN_POINT('',(-9.,-3.,-2.2));
#26633=CARTESIAN_POINT('',(9.,-3.,-2.2));
#26634=CARTESIAN_POINT('',(-9.,-3.,-1.2));
#26635=CARTESIAN_POINT('',(-9.,-3.,-2.2));
#26636=CARTESIAN_POINT('',(9.,-3.,-1.2));
#26637=CARTESIAN_POINT('',(9.,-3.,-1.2));
#26638=CARTESIAN_POINT('',(9.,-3.,-2.2));
#26639=CARTESIAN_POINT('Origin',(9.,-4.5,-2.2));
#26640=CARTESIAN_POINT('',(9.,-4.5,-2.2));
#26641=CARTESIAN_POINT('',(9.,-4.5,-2.2));
#26642=CARTESIAN_POINT('',(9.,-4.5,-1.2));
#26643=CARTESIAN_POINT('',(9.,-4.5,-1.2));
#26644=CARTESIAN_POINT('',(9.,-4.5,-2.2));
#26645=CARTESIAN_POINT('Origin',(-9.,-4.5,-2.2));
#26646=CARTESIAN_POINT('',(-9.,-4.5,-2.2));
#26647=CARTESIAN_POINT('',(-9.,-4.5,-2.2));
#26648=CARTESIAN_POINT('',(-9.,-4.5,-1.2));
#26649=CARTESIAN_POINT('',(-9.,-4.5,-1.2));
#26650=CARTESIAN_POINT('',(-9.,-4.5,-2.2));
#26651=CARTESIAN_POINT('Origin',(-9.,-3.,-2.2));
#26652=CARTESIAN_POINT('',(-9.,-3.,-2.2));
#26653=CARTESIAN_POINT('',(-9.,-3.,-1.2));
#26654=CARTESIAN_POINT('Origin',(0.,-3.75,-1.2));
#26655=CARTESIAN_POINT('Origin',(0.,-3.75,-2.2));
#26656=CARTESIAN_POINT('',(0.,0.,0.));
#26657=CARTESIAN_POINT('Origin',(9.,12.5,-2.2));
#26658=CARTESIAN_POINT('',(9.,12.5,-2.2));
#26659=CARTESIAN_POINT('',(-9.,12.5,-2.2));
#26660=CARTESIAN_POINT('',(9.,12.5,-2.2));
#26661=CARTESIAN_POINT('',(-9.,12.5,-1.2));
#26662=CARTESIAN_POINT('',(-9.,12.5,-2.2));
#26663=CARTESIAN_POINT('',(9.,12.5,-1.2));
#26664=CARTESIAN_POINT('',(9.,12.5,-1.2));
#26665=CARTESIAN_POINT('',(9.,12.5,-2.2));
#26666=CARTESIAN_POINT('Origin',(9.,11.,-2.2));
#26667=CARTESIAN_POINT('',(9.,11.,-2.2));
#26668=CARTESIAN_POINT('',(9.,11.,-2.2));
#26669=CARTESIAN_POINT('',(9.,11.,-1.2));
#26670=CARTESIAN_POINT('',(9.,11.,-1.2));
#26671=CARTESIAN_POINT('',(9.,11.,-2.2));
#26672=CARTESIAN_POINT('Origin',(-9.,11.,-2.2));
#26673=CARTESIAN_POINT('',(-9.,11.,-2.2));
#26674=CARTESIAN_POINT('',(-9.,11.,-2.2));
#26675=CARTESIAN_POINT('',(-9.,11.,-1.2));
#26676=CARTESIAN_POINT('',(-9.,11.,-1.2));
#26677=CARTESIAN_POINT('',(-9.,11.,-2.2));
#26678=CARTESIAN_POINT('Origin',(-9.,12.5,-2.2));
#26679=CARTESIAN_POINT('',(-9.,12.5,-2.2));
#26680=CARTESIAN_POINT('',(-9.,12.5,-1.2));
#26681=CARTESIAN_POINT('Origin',(0.,11.75,-1.2));
#26682=CARTESIAN_POINT('Origin',(0.,11.75,-2.2));
#26683=CARTESIAN_POINT('',(0.,0.,0.));
#26684=CARTESIAN_POINT('Origin',(5.,5.5,30.4));
#26685=CARTESIAN_POINT('',(4.725,5.5,30.5));
#26686=CARTESIAN_POINT('Origin',(5.,5.5,30.5));
#26687=CARTESIAN_POINT('',(4.725,5.5,31.5));
#26688=CARTESIAN_POINT('',(4.725,5.5,30.4));
#26689=CARTESIAN_POINT('Origin',(5.,5.5,31.5));
#26690=CARTESIAN_POINT('Origin',(7.,5.5,30.4));
#26691=CARTESIAN_POINT('',(6.725,5.5,30.5));
#26692=CARTESIAN_POINT('Origin',(7.,5.5,30.5));
#26693=CARTESIAN_POINT('',(6.725,5.5,31.5));
#26694=CARTESIAN_POINT('',(6.725,5.5,30.4));
#26695=CARTESIAN_POINT('Origin',(7.,5.5,31.5));
#26696=CARTESIAN_POINT('Origin',(-7.,5.5,30.4));
#26697=CARTESIAN_POINT('',(-7.275,5.5,30.5));
#26698=CARTESIAN_POINT('Origin',(-7.,5.5,30.5));
#26699=CARTESIAN_POINT('',(-7.275,5.5,31.5));
#26700=CARTESIAN_POINT('',(-7.275,5.5,30.4));
#26701=CARTESIAN_POINT('Origin',(-7.,5.5,31.5));
#26702=CARTESIAN_POINT('Origin',(-5.,5.5,30.4));
#26703=CARTESIAN_POINT('',(-5.275,5.5,30.5));
#26704=CARTESIAN_POINT('Origin',(-5.,5.5,30.5));
#26705=CARTESIAN_POINT('',(-5.275,5.5,31.5));
#26706=CARTESIAN_POINT('',(-5.275,5.5,30.4));
#26707=CARTESIAN_POINT('Origin',(-5.,5.5,31.5));
#26708=CARTESIAN_POINT('Origin',(7.,9.5,30.4));
#26709=CARTESIAN_POINT('',(6.725,9.5,30.5));
#26710=CARTESIAN_POINT('Origin',(7.,9.5,30.5));
#26711=CARTESIAN_POINT('',(6.725,9.5,31.5));
#26712=CARTESIAN_POINT('',(6.725,9.5,30.4));
#26713=CARTESIAN_POINT('Origin',(7.,9.5,31.5));
#26714=CARTESIAN_POINT('Origin',(7.,10.5,30.4));
#26715=CARTESIAN_POINT('',(6.725,10.5,30.5));
#26716=CARTESIAN_POINT('Origin',(7.,10.5,30.5));
#26717=CARTESIAN_POINT('',(6.725,10.5,31.5));
#26718=CARTESIAN_POINT('',(6.725,10.5,30.4));
#26719=CARTESIAN_POINT('Origin',(7.,10.5,31.5));
#26720=CARTESIAN_POINT('Origin',(-7.,9.5,30.4));
#26721=CARTESIAN_POINT('',(-7.275,9.5,30.5));
#26722=CARTESIAN_POINT('Origin',(-7.,9.5,30.5));
#26723=CARTESIAN_POINT('',(-7.275,9.5,31.5));
#26724=CARTESIAN_POINT('',(-7.275,9.5,30.4));
#26725=CARTESIAN_POINT('Origin',(-7.,9.5,31.5));
#26726=CARTESIAN_POINT('Origin',(-7.,10.5,30.4));
#26727=CARTESIAN_POINT('',(-7.275,10.5,30.5));
#26728=CARTESIAN_POINT('Origin',(-7.,10.5,30.5));
#26729=CARTESIAN_POINT('',(-7.275,10.5,31.5));
#26730=CARTESIAN_POINT('',(-7.275,10.5,30.4));
#26731=CARTESIAN_POINT('Origin',(-7.,10.5,31.5));
#26732=CARTESIAN_POINT('Origin',(-3.6,1.4,30.4));
#26733=CARTESIAN_POINT('',(3.6,1.4,31.5));
#26734=CARTESIAN_POINT('',(-3.6,1.4,31.5));
#26735=CARTESIAN_POINT('',(-1.8,1.4,31.5));
#26736=CARTESIAN_POINT('',(3.6,1.4,30.5));
#26737=CARTESIAN_POINT('',(3.6,1.4,30.4));
#26738=CARTESIAN_POINT('',(-3.6,1.4,30.5));
#26739=CARTESIAN_POINT('',(-1.8,1.4,30.5));
#26740=CARTESIAN_POINT('',(-3.6,1.4,30.4));
#26741=CARTESIAN_POINT('Origin',(-3.6,8.6,30.4));
#26742=CARTESIAN_POINT('',(-3.6,8.6,31.5));
#26743=CARTESIAN_POINT('',(-3.6,6.175,31.5));
#26744=CARTESIAN_POINT('',(-3.6,8.6,30.5));
#26745=CARTESIAN_POINT('',(-3.6,6.175,30.5));
#26746=CARTESIAN_POINT('',(-3.6,8.6,30.4));
#26747=CARTESIAN_POINT('Origin',(3.6,8.6,30.4));
#26748=CARTESIAN_POINT('',(3.6,8.6,31.5));
#26749=CARTESIAN_POINT('',(1.8,8.6,31.5));
#26750=CARTESIAN_POINT('',(3.6,8.6,30.5));
#26751=CARTESIAN_POINT('',(1.8,8.6,30.5));
#26752=CARTESIAN_POINT('',(3.6,8.6,30.4));
#26753=CARTESIAN_POINT('Origin',(3.6,1.4,30.4));
#26754=CARTESIAN_POINT('',(3.6,2.575,31.5));
#26755=CARTESIAN_POINT('',(3.6,2.575,30.5));
#26756=CARTESIAN_POINT('Origin',(-6.,0.,30.4));
#26757=CARTESIAN_POINT('',(-6.61,-7.47034547479886E-17,30.5));
#26758=CARTESIAN_POINT('Origin',(-6.,0.,30.5));
#26759=CARTESIAN_POINT('',(-6.61,7.47034547479886E-17,31.5));
#26760=CARTESIAN_POINT('',(-6.61,-7.47034547479886E-17,30.4));
#26761=CARTESIAN_POINT('Origin',(-6.,0.,31.5));
#26762=CARTESIAN_POINT('Origin',(6.,0.,30.4));
#26763=CARTESIAN_POINT('',(5.39,-7.47034547479886E-17,30.5));
#26764=CARTESIAN_POINT('Origin',(6.,0.,30.5));
#26765=CARTESIAN_POINT('',(5.39,7.47034547479886E-17,31.5));
#26766=CARTESIAN_POINT('',(5.39,-7.47034547479886E-17,30.4));
#26767=CARTESIAN_POINT('Origin',(6.,0.,31.5));
#26768=CARTESIAN_POINT('Origin',(7.5,11.,30.5));
#26769=CARTESIAN_POINT('',(7.5,11.,30.5));
#26770=CARTESIAN_POINT('',(-7.5,11.,30.5));
#26771=CARTESIAN_POINT('',(7.5,11.,30.5));
#26772=CARTESIAN_POINT('',(-7.5,11.,31.5));
#26773=CARTESIAN_POINT('',(-7.5,11.,30.5));
#26774=CARTESIAN_POINT('',(7.5,11.,31.5));
#26775=CARTESIAN_POINT('',(7.5,11.,31.5));
#26776=CARTESIAN_POINT('',(7.5,11.,30.5));
#26777=CARTESIAN_POINT('Origin',(7.5,-3.5,30.5));
#26778=CARTESIAN_POINT('',(7.5,-3.5,30.5));
#26779=CARTESIAN_POINT('',(7.5,-3.5,30.5));
#26780=CARTESIAN_POINT('',(7.5,-3.5,31.5));
#26781=CARTESIAN_POINT('',(7.5,-3.5,31.5));
#26782=CARTESIAN_POINT('',(7.5,-3.5,30.5));
#26783=CARTESIAN_POINT('Origin',(-7.5,-3.5,30.5));
#26784=CARTESIAN_POINT('',(-7.5,-3.5,30.5));
#26785=CARTESIAN_POINT('',(-7.5,-3.5,30.5));
#26786=CARTESIAN_POINT('',(-7.5,-3.5,31.5));
#26787=CARTESIAN_POINT('',(-7.5,-3.5,31.5));
#26788=CARTESIAN_POINT('',(-7.5,-3.5,30.5));
#26789=CARTESIAN_POINT('Origin',(-7.5,11.,30.5));
#26790=CARTESIAN_POINT('',(-7.5,11.,30.5));
#26791=CARTESIAN_POINT('',(-7.5,11.,31.5));
#26792=CARTESIAN_POINT('Origin',(0.,3.75,31.5));
#26793=CARTESIAN_POINT('Origin',(0.,3.75,30.5));
#26794=CARTESIAN_POINT('',(0.,0.,0.));
#26795=CARTESIAN_POINT('Origin',(-7.6,9.5,24.));
#26796=CARTESIAN_POINT('',(-7.5,9.5,24.275));
#26797=CARTESIAN_POINT('Origin',(-7.5,9.5,24.));
#26798=CARTESIAN_POINT('',(-6.5,9.5,24.275));
#26799=CARTESIAN_POINT('',(-7.6,9.5,24.275));
#26800=CARTESIAN_POINT('Origin',(-6.5,9.5,24.));
#26801=CARTESIAN_POINT('Origin',(-7.6,10.5,24.));
#26802=CARTESIAN_POINT('',(-7.5,10.5,24.275));
#26803=CARTESIAN_POINT('Origin',(-7.5,10.5,24.));
#26804=CARTESIAN_POINT('',(-6.5,10.5,24.275));
#26805=CARTESIAN_POINT('',(-7.6,10.5,24.275));
#26806=CARTESIAN_POINT('Origin',(-6.5,10.5,24.));
#26807=CARTESIAN_POINT('Origin',(-7.,9.5,29.4));
#26808=CARTESIAN_POINT('',(-7.21,9.5,29.4));
#26809=CARTESIAN_POINT('Origin',(-7.,9.5,29.4));
#26810=CARTESIAN_POINT('',(-7.21,9.5,30.5));
#26811=CARTESIAN_POINT('',(-7.21,9.5,29.4));
#26812=CARTESIAN_POINT('Origin',(-7.,9.5,30.5));
#26813=CARTESIAN_POINT('Origin',(-7.,9.5,29.4));
#26814=CARTESIAN_POINT('Origin',(-7.,10.5,29.4));
#26815=CARTESIAN_POINT('',(-7.21,10.5,29.4));
#26816=CARTESIAN_POINT('Origin',(-7.,10.5,29.4));
#26817=CARTESIAN_POINT('',(-7.21,10.5,30.5));
#26818=CARTESIAN_POINT('',(-7.21,10.5,29.4));
#26819=CARTESIAN_POINT('Origin',(-7.,10.5,30.5));
#26820=CARTESIAN_POINT('Origin',(-7.,10.5,29.4));
#26821=CARTESIAN_POINT('Origin',(-7.,9.5,-0.1));
#26822=CARTESIAN_POINT('',(-7.21,9.5,0.));
#26823=CARTESIAN_POINT('Origin',(-7.,9.5,0.));
#26824=CARTESIAN_POINT('',(-7.21,9.5,1.1));
#26825=CARTESIAN_POINT('',(-7.21,9.5,-0.1));
#26826=CARTESIAN_POINT('Origin',(-7.,9.5,1.1));
#26827=CARTESIAN_POINT('Origin',(-7.,9.5,1.1));
#26828=CARTESIAN_POINT('Origin',(-7.,10.5,-0.1));
#26829=CARTESIAN_POINT('',(-7.21,10.5,0.));
#26830=CARTESIAN_POINT('Origin',(-7.,10.5,0.));
#26831=CARTESIAN_POINT('',(-7.21,10.5,1.1));
#26832=CARTESIAN_POINT('',(-7.21,10.5,-0.1));
#26833=CARTESIAN_POINT('Origin',(-7.,10.5,1.1));
#26834=CARTESIAN_POINT('Origin',(-7.,10.5,1.1));
#26835=CARTESIAN_POINT('Origin',(-6.5,11.,0.));
#26836=CARTESIAN_POINT('',(-6.5,11.,0.));
#26837=CARTESIAN_POINT('',(-7.5,11.,0.));
#26838=CARTESIAN_POINT('',(-6.5,11.,0.));
#26839=CARTESIAN_POINT('',(-7.5,11.,30.5));
#26840=CARTESIAN_POINT('',(-7.5,11.,0.));
#26841=CARTESIAN_POINT('',(-6.5,11.,30.5));
#26842=CARTESIAN_POINT('',(-6.5,11.,30.5));
#26843=CARTESIAN_POINT('',(-6.5,11.,0.));
#26844=CARTESIAN_POINT('Origin',(-6.5,9.,0.));
#26845=CARTESIAN_POINT('',(-6.5,9.,0.));
#26846=CARTESIAN_POINT('',(-6.5,9.,0.));
#26847=CARTESIAN_POINT('',(-6.5,9.,30.5));
#26848=CARTESIAN_POINT('',(-6.5,9.,30.5));
#26849=CARTESIAN_POINT('',(-6.5,9.,0.));
#26850=CARTESIAN_POINT('Origin',(-7.5,9.,0.));
#26851=CARTESIAN_POINT('',(-7.5,9.,0.));
#26852=CARTESIAN_POINT('',(-7.5,9.,0.));
#26853=CARTESIAN_POINT('',(-7.5,9.,30.5));
#26854=CARTESIAN_POINT('',(-7.5,9.,30.5));
#26855=CARTESIAN_POINT('',(-7.5,9.,0.));
#26856=CARTESIAN_POINT('Origin',(-7.5,11.,0.));
#26857=CARTESIAN_POINT('',(-7.5,11.,0.));
#26858=CARTESIAN_POINT('',(-7.5,11.,30.5));
#26859=CARTESIAN_POINT('Origin',(-7.,10.,30.5));
#26860=CARTESIAN_POINT('Origin',(-7.,10.,0.));
#26861=CARTESIAN_POINT('',(0.,0.,0.));
#26862=CARTESIAN_POINT('Origin',(6.4,9.5,24.));
#26863=CARTESIAN_POINT('',(6.5,9.5,24.275));
#26864=CARTESIAN_POINT('Origin',(6.5,9.5,24.));
#26865=CARTESIAN_POINT('',(7.5,9.5,24.275));
#26866=CARTESIAN_POINT('',(6.4,9.5,24.275));
#26867=CARTESIAN_POINT('Origin',(7.5,9.5,24.));
#26868=CARTESIAN_POINT('Origin',(6.4,10.5,24.));
#26869=CARTESIAN_POINT('',(6.5,10.5,24.275));
#26870=CARTESIAN_POINT('Origin',(6.5,10.5,24.));
#26871=CARTESIAN_POINT('',(7.5,10.5,24.275));
#26872=CARTESIAN_POINT('',(6.4,10.5,24.275));
#26873=CARTESIAN_POINT('Origin',(7.5,10.5,24.));
#26874=CARTESIAN_POINT('Origin',(7.,9.5,29.4));
#26875=CARTESIAN_POINT('',(6.79,9.5,29.4));
#26876=CARTESIAN_POINT('Origin',(7.,9.5,29.4));
#26877=CARTESIAN_POINT('',(6.79,9.5,30.5));
#26878=CARTESIAN_POINT('',(6.79,9.5,29.4));
#26879=CARTESIAN_POINT('Origin',(7.,9.5,30.5));
#26880=CARTESIAN_POINT('Origin',(7.,9.5,29.4));
#26881=CARTESIAN_POINT('Origin',(7.,10.5,29.4));
#26882=CARTESIAN_POINT('',(6.79,10.5,29.4));
#26883=CARTESIAN_POINT('Origin',(7.,10.5,29.4));
#26884=CARTESIAN_POINT('',(6.79,10.5,30.5));
#26885=CARTESIAN_POINT('',(6.79,10.5,29.4));
#26886=CARTESIAN_POINT('Origin',(7.,10.5,30.5));
#26887=CARTESIAN_POINT('Origin',(7.,10.5,29.4));
#26888=CARTESIAN_POINT('Origin',(7.,9.5,-0.1));
#26889=CARTESIAN_POINT('',(6.79,9.5,0.));
#26890=CARTESIAN_POINT('Origin',(7.,9.5,0.));
#26891=CARTESIAN_POINT('',(6.79,9.5,1.1));
#26892=CARTESIAN_POINT('',(6.79,9.5,-0.1));
#26893=CARTESIAN_POINT('Origin',(7.,9.5,1.1));
#26894=CARTESIAN_POINT('Origin',(7.,9.5,1.1));
#26895=CARTESIAN_POINT('Origin',(7.,10.5,-0.1));
#26896=CARTESIAN_POINT('',(6.79,10.5,0.));
#26897=CARTESIAN_POINT('Origin',(7.,10.5,0.));
#26898=CARTESIAN_POINT('',(6.79,10.5,1.1));
#26899=CARTESIAN_POINT('',(6.79,10.5,-0.1));
#26900=CARTESIAN_POINT('Origin',(7.,10.5,1.1));
#26901=CARTESIAN_POINT('Origin',(7.,10.5,1.1));
#26902=CARTESIAN_POINT('Origin',(7.5,11.,0.));
#26903=CARTESIAN_POINT('',(7.5,11.,0.));
#26904=CARTESIAN_POINT('',(6.5,11.,0.));
#26905=CARTESIAN_POINT('',(7.5,11.,0.));
#26906=CARTESIAN_POINT('',(6.5,11.,30.5));
#26907=CARTESIAN_POINT('',(6.5,11.,0.));
#26908=CARTESIAN_POINT('',(7.5,11.,30.5));
#26909=CARTESIAN_POINT('',(7.5,11.,30.5));
#26910=CARTESIAN_POINT('',(7.5,11.,0.));
#26911=CARTESIAN_POINT('Origin',(7.5,9.,0.));
#26912=CARTESIAN_POINT('',(7.5,9.,0.));
#26913=CARTESIAN_POINT('',(7.5,9.,0.));
#26914=CARTESIAN_POINT('',(7.5,9.,30.5));
#26915=CARTESIAN_POINT('',(7.5,9.,30.5));
#26916=CARTESIAN_POINT('',(7.5,9.,0.));
#26917=CARTESIAN_POINT('Origin',(6.5,9.,0.));
#26918=CARTESIAN_POINT('',(6.5,9.,0.));
#26919=CARTESIAN_POINT('',(6.5,9.,0.));
#26920=CARTESIAN_POINT('',(6.5,9.,30.5));
#26921=CARTESIAN_POINT('',(6.5,9.,30.5));
#26922=CARTESIAN_POINT('',(6.5,9.,0.));
#26923=CARTESIAN_POINT('Origin',(6.5,11.,0.));
#26924=CARTESIAN_POINT('',(6.5,11.,0.));
#26925=CARTESIAN_POINT('',(6.5,11.,30.5));
#26926=CARTESIAN_POINT('Origin',(7.,10.,30.5));
#26927=CARTESIAN_POINT('Origin',(7.,10.,0.));
#26928=CARTESIAN_POINT('',(0.,0.,0.));
#26929=CARTESIAN_POINT('Origin',(-7.6,2.7,-0.1));
#26930=CARTESIAN_POINT('',(-7.81,2.7,0.));
#26931=CARTESIAN_POINT('Origin',(-7.6,2.7,0.));
#26932=CARTESIAN_POINT('',(-7.81,2.7,0.9));
#26933=CARTESIAN_POINT('',(-7.81,2.7,-0.1));
#26934=CARTESIAN_POINT('Origin',(-7.6,2.7,0.9));
#26935=CARTESIAN_POINT('Origin',(-7.6,2.7,0.9));
#26936=CARTESIAN_POINT('Origin',(-4.4,2.7,-0.1));
#26937=CARTESIAN_POINT('',(-4.61,2.7,0.));
#26938=CARTESIAN_POINT('Origin',(-4.4,2.7,0.));
#26939=CARTESIAN_POINT('',(-4.61,2.7,0.9));
#26940=CARTESIAN_POINT('',(-4.61,2.7,-0.1));
#26941=CARTESIAN_POINT('Origin',(-4.4,2.7,0.9));
#26942=CARTESIAN_POINT('Origin',(-4.4,2.7,0.9));
#26943=CARTESIAN_POINT('Origin',(-7.6,2.2,1.2));
#26944=CARTESIAN_POINT('',(-7.81,2.3,1.2));
#26945=CARTESIAN_POINT('Origin',(-7.6,2.3,1.2));
#26946=CARTESIAN_POINT('',(-7.81,3.1,1.2));
#26947=CARTESIAN_POINT('',(-7.81,2.2,1.2));
#26948=CARTESIAN_POINT('Origin',(-7.6,3.1,1.2));
#26949=CARTESIAN_POINT('Origin',(-4.4,2.2,1.2));
#26950=CARTESIAN_POINT('',(-4.61,2.3,1.2));
#26951=CARTESIAN_POINT('Origin',(-4.4,2.3,1.2));
#26952=CARTESIAN_POINT('',(-4.61,3.1,1.2));
#26953=CARTESIAN_POINT('',(-4.61,2.2,1.2));
#26954=CARTESIAN_POINT('Origin',(-4.4,3.1,1.2));
#26955=CARTESIAN_POINT('Origin',(-3.6,3.1,0.));
#26956=CARTESIAN_POINT('',(-3.6,3.1,0.));
#26957=CARTESIAN_POINT('',(-8.4,3.1,0.));
#26958=CARTESIAN_POINT('',(-3.6,3.1,0.));
#26959=CARTESIAN_POINT('',(-8.4,3.1,3.));
#26960=CARTESIAN_POINT('',(-8.4,3.1,0.));
#26961=CARTESIAN_POINT('',(-3.6,3.1,3.));
#26962=CARTESIAN_POINT('',(-3.6,3.1,3.));
#26963=CARTESIAN_POINT('',(-3.6,3.1,0.));
#26964=CARTESIAN_POINT('Origin',(-3.6,2.3,0.));
#26965=CARTESIAN_POINT('',(-3.6,2.3,0.));
#26966=CARTESIAN_POINT('',(-3.6,2.3,0.));
#26967=CARTESIAN_POINT('',(-3.6,2.3,3.));
#26968=CARTESIAN_POINT('',(-3.6,2.3,3.));
#26969=CARTESIAN_POINT('',(-3.6,2.3,0.));
#26970=CARTESIAN_POINT('Origin',(-8.4,2.3,0.));
#26971=CARTESIAN_POINT('',(-8.4,2.3,0.));
#26972=CARTESIAN_POINT('',(-8.4,2.3,0.));
#26973=CARTESIAN_POINT('',(-8.4,2.3,3.));
#26974=CARTESIAN_POINT('',(-8.4,2.3,3.));
#26975=CARTESIAN_POINT('',(-8.4,2.3,0.));
#26976=CARTESIAN_POINT('Origin',(-8.4,3.1,0.));
#26977=CARTESIAN_POINT('',(-8.4,3.1,0.));
#26978=CARTESIAN_POINT('',(-8.4,3.1,3.));
#26979=CARTESIAN_POINT('Origin',(-6.,2.7,3.));
#26980=CARTESIAN_POINT('Origin',(-6.,2.7,0.));
#26981=CARTESIAN_POINT('',(0.,0.,0.));
#26982=CARTESIAN_POINT('Origin',(-7.,5.5,29.6));
#26983=CARTESIAN_POINT('',(-7.21,5.5,29.7));
#26984=CARTESIAN_POINT('Origin',(-7.,5.5,29.7));
#26985=CARTESIAN_POINT('',(-7.21,5.5,30.5));
#26986=CARTESIAN_POINT('',(-7.21,5.5,29.6));
#26987=CARTESIAN_POINT('Origin',(-7.,5.5,30.5));
#26988=CARTESIAN_POINT('Origin',(-5.,5.5,29.6));
#26989=CARTESIAN_POINT('',(-5.21,5.5,29.7));
#26990=CARTESIAN_POINT('Origin',(-5.,5.5,29.7));
#26991=CARTESIAN_POINT('',(-5.21,5.5,30.5));
#26992=CARTESIAN_POINT('',(-5.21,5.5,29.6));
#26993=CARTESIAN_POINT('Origin',(-5.,5.5,30.5));
#26994=CARTESIAN_POINT('Origin',(-7.6,2.2,29.8));
#26995=CARTESIAN_POINT('',(-7.81,2.3,29.8));
#26996=CARTESIAN_POINT('Origin',(-7.6,2.3,29.8));
#26997=CARTESIAN_POINT('',(-7.81,3.2,29.8));
#26998=CARTESIAN_POINT('',(-7.81,2.2,29.8));
#26999=CARTESIAN_POINT('',(-7.41533814687381,3.2,29.7));
#27000=CARTESIAN_POINT('Origin',(-7.6,3.2,29.8));
#27001=CARTESIAN_POINT('',(-7.4153381468738,3.1,29.7));
#27002=CARTESIAN_POINT('',(-7.41533814687381,2.2,29.7));
#27003=CARTESIAN_POINT('',(-7.78466185312619,3.1,29.7));
#27004=CARTESIAN_POINT('Origin',(-7.6,3.1,29.8));
#27005=CARTESIAN_POINT('',(-7.78466185312619,3.2,29.7));
#27006=CARTESIAN_POINT('',(-7.78466185312619,2.2,29.7));
#27007=CARTESIAN_POINT('Origin',(-7.6,3.2,29.8));
#27008=CARTESIAN_POINT('Origin',(-7.6,3.2,29.8));
#27009=CARTESIAN_POINT('',(-5.6,3.2,29.7));
#27010=CARTESIAN_POINT('Origin',(-4.4,2.2,29.8));
#27011=CARTESIAN_POINT('',(-4.61,2.3,29.8));
#27012=CARTESIAN_POINT('Origin',(-4.4,2.3,29.8));
#27013=CARTESIAN_POINT('',(-4.61,3.2,29.8));
#27014=CARTESIAN_POINT('',(-4.61,2.2,29.8));
#27015=CARTESIAN_POINT('',(-4.21533814687381,3.2,29.7));
#27016=CARTESIAN_POINT('Origin',(-4.4,3.2,29.8));
#27017=CARTESIAN_POINT('',(-4.21533814687381,3.1,29.7));
#27018=CARTESIAN_POINT('',(-4.21533814687381,2.2,29.7));
#27019=CARTESIAN_POINT('',(-4.5846618531262,3.1,29.7));
#27020=CARTESIAN_POINT('Origin',(-4.4,3.1,29.8));
#27021=CARTESIAN_POINT('',(-4.58466185312619,3.2,29.7));
#27022=CARTESIAN_POINT('',(-4.58466185312619,2.2,29.7));
#27023=CARTESIAN_POINT('Origin',(-4.4,3.2,29.8));
#27024=CARTESIAN_POINT('Origin',(-4.4,3.2,29.8));
#27025=CARTESIAN_POINT('',(-4.,3.2,29.7));
#27026=CARTESIAN_POINT('Origin',(-3.6,3.1,28.));
#27027=CARTESIAN_POINT('',(-3.6,3.1,29.7));
#27028=CARTESIAN_POINT('',(-3.6,3.1,29.7));
#27029=CARTESIAN_POINT('',(-3.6,3.1,29.7));
#27030=CARTESIAN_POINT('',(-3.6,3.1,28.));
#27031=CARTESIAN_POINT('',(-3.6,3.1,28.));
#27032=CARTESIAN_POINT('',(-8.4,3.1,28.));
#27033=CARTESIAN_POINT('',(-3.6,3.1,28.));
#27034=CARTESIAN_POINT('',(-8.4,3.1,29.7));
#27035=CARTESIAN_POINT('',(-8.4,3.1,28.));
#27036=CARTESIAN_POINT('',(-3.6,3.1,29.7));
#27037=CARTESIAN_POINT('Origin',(-3.6,2.3,29.7));
#27038=CARTESIAN_POINT('',(-8.4,7.,29.7));
#27039=CARTESIAN_POINT('',(-8.4,2.3,29.7));
#27040=CARTESIAN_POINT('',(-3.6,7.,29.7));
#27041=CARTESIAN_POINT('',(-8.4,7.,29.7));
#27042=CARTESIAN_POINT('',(-3.6,2.3,29.7));
#27043=CARTESIAN_POINT('Origin',(-6.,7.,30.1));
#27044=CARTESIAN_POINT('',(-8.4,7.,30.5));
#27045=CARTESIAN_POINT('',(-3.6,7.,30.5));
#27046=CARTESIAN_POINT('',(-3.6,7.,30.5));
#27047=CARTESIAN_POINT('',(-3.6,7.,29.7));
#27048=CARTESIAN_POINT('',(-8.4,7.,30.5));
#27049=CARTESIAN_POINT('Origin',(-3.6,2.3,28.));
#27050=CARTESIAN_POINT('',(-3.6,2.3,28.));
#27051=CARTESIAN_POINT('',(-3.6,2.3,30.5));
#27052=CARTESIAN_POINT('',(-3.6,2.3,28.));
#27053=CARTESIAN_POINT('',(-3.6,2.3,28.));
#27054=CARTESIAN_POINT('',(-3.6,2.3,30.5));
#27055=CARTESIAN_POINT('Origin',(-8.4,2.3,28.));
#27056=CARTESIAN_POINT('',(-8.4,2.3,28.));
#27057=CARTESIAN_POINT('',(-8.4,2.3,30.5));
#27058=CARTESIAN_POINT('',(-8.4,2.3,28.));
#27059=CARTESIAN_POINT('',(-8.4,2.3,28.));
#27060=CARTESIAN_POINT('',(-8.4,2.3,30.5));
#27061=CARTESIAN_POINT('Origin',(-8.4,3.1,28.));
#27062=CARTESIAN_POINT('',(-8.4,3.1,28.));
#27063=CARTESIAN_POINT('',(-8.4,2.3,30.5));
#27064=CARTESIAN_POINT('Origin',(-6.,2.7,30.5));
#27065=CARTESIAN_POINT('Origin',(-6.,2.7,28.));
#27066=CARTESIAN_POINT('',(0.,0.,0.));
#27067=CARTESIAN_POINT('Origin',(4.4,2.7,-0.1));
#27068=CARTESIAN_POINT('',(4.19,2.7,0.));
#27069=CARTESIAN_POINT('Origin',(4.4,2.7,0.));
#27070=CARTESIAN_POINT('',(4.19,2.7,0.9));
#27071=CARTESIAN_POINT('',(4.19,2.7,-0.1));
#27072=CARTESIAN_POINT('Origin',(4.4,2.7,0.9));
#27073=CARTESIAN_POINT('Origin',(4.4,2.7,0.9));
#27074=CARTESIAN_POINT('Origin',(7.6,2.7,-0.1));
#27075=CARTESIAN_POINT('',(7.39,2.7,0.));
#27076=CARTESIAN_POINT('Origin',(7.6,2.7,0.));
#27077=CARTESIAN_POINT('',(7.39,2.7,0.9));
#27078=CARTESIAN_POINT('',(7.39,2.7,-0.1));
#27079=CARTESIAN_POINT('Origin',(7.6,2.7,0.9));
#27080=CARTESIAN_POINT('Origin',(7.6,2.7,0.9));
#27081=CARTESIAN_POINT('Origin',(4.4,2.2,1.2));
#27082=CARTESIAN_POINT('',(4.19,2.3,1.2));
#27083=CARTESIAN_POINT('Origin',(4.4,2.3,1.2));
#27084=CARTESIAN_POINT('',(4.19,3.1,1.2));
#27085=CARTESIAN_POINT('',(4.19,2.2,1.2));
#27086=CARTESIAN_POINT('Origin',(4.4,3.1,1.2));
#27087=CARTESIAN_POINT('Origin',(7.6,2.2,1.2));
#27088=CARTESIAN_POINT('',(7.39,2.3,1.2));
#27089=CARTESIAN_POINT('Origin',(7.6,2.3,1.2));
#27090=CARTESIAN_POINT('',(7.39,3.1,1.2));
#27091=CARTESIAN_POINT('',(7.39,2.2,1.2));
#27092=CARTESIAN_POINT('Origin',(7.6,3.1,1.2));
#27093=CARTESIAN_POINT('Origin',(8.4,3.1,0.));
#27094=CARTESIAN_POINT('',(8.4,3.1,0.));
#27095=CARTESIAN_POINT('',(3.6,3.1,0.));
#27096=CARTESIAN_POINT('',(8.4,3.1,0.));
#27097=CARTESIAN_POINT('',(3.6,3.1,3.));
#27098=CARTESIAN_POINT('',(3.6,3.1,0.));
#27099=CARTESIAN_POINT('',(8.4,3.1,3.));
#27100=CARTESIAN_POINT('',(8.4,3.1,3.));
#27101=CARTESIAN_POINT('',(8.4,3.1,0.));
#27102=CARTESIAN_POINT('Origin',(8.4,2.3,0.));
#27103=CARTESIAN_POINT('',(8.4,2.3,0.));
#27104=CARTESIAN_POINT('',(8.4,2.3,0.));
#27105=CARTESIAN_POINT('',(8.4,2.3,3.));
#27106=CARTESIAN_POINT('',(8.4,2.3,3.));
#27107=CARTESIAN_POINT('',(8.4,2.3,0.));
#27108=CARTESIAN_POINT('Origin',(3.6,2.3,0.));
#27109=CARTESIAN_POINT('',(3.6,2.3,0.));
#27110=CARTESIAN_POINT('',(3.6,2.3,0.));
#27111=CARTESIAN_POINT('',(3.6,2.3,3.));
#27112=CARTESIAN_POINT('',(3.6,2.3,3.));
#27113=CARTESIAN_POINT('',(3.6,2.3,0.));
#27114=CARTESIAN_POINT('Origin',(3.6,3.1,0.));
#27115=CARTESIAN_POINT('',(3.6,3.1,0.));
#27116=CARTESIAN_POINT('',(3.6,3.1,3.));
#27117=CARTESIAN_POINT('Origin',(6.,2.7,3.));
#27118=CARTESIAN_POINT('Origin',(6.,2.7,0.));
#27119=CARTESIAN_POINT('',(0.,0.,0.));
#27120=CARTESIAN_POINT('Origin',(5.,5.5,29.6));
#27121=CARTESIAN_POINT('',(4.79,5.5,29.7));
#27122=CARTESIAN_POINT('Origin',(5.,5.5,29.7));
#27123=CARTESIAN_POINT('',(4.79,5.5,30.5));
#27124=CARTESIAN_POINT('',(4.79,5.5,29.6));
#27125=CARTESIAN_POINT('Origin',(5.,5.5,30.5));
#27126=CARTESIAN_POINT('Origin',(7.,5.5,29.6));
#27127=CARTESIAN_POINT('',(6.79,5.5,29.7));
#27128=CARTESIAN_POINT('Origin',(7.,5.5,29.7));
#27129=CARTESIAN_POINT('',(6.79,5.5,30.5));
#27130=CARTESIAN_POINT('',(6.79,5.5,29.6));
#27131=CARTESIAN_POINT('Origin',(7.,5.5,30.5));
#27132=CARTESIAN_POINT('Origin',(4.4,2.2,29.8));
#27133=CARTESIAN_POINT('',(4.19,2.3,29.8));
#27134=CARTESIAN_POINT('Origin',(4.4,2.3,29.8));
#27135=CARTESIAN_POINT('',(4.19,3.2,29.8));
#27136=CARTESIAN_POINT('',(4.19,2.2,29.8));
#27137=CARTESIAN_POINT('',(4.58466185312619,3.2,29.7));
#27138=CARTESIAN_POINT('Origin',(4.4,3.2,29.8));
#27139=CARTESIAN_POINT('',(4.5846618531262,3.1,29.7));
#27140=CARTESIAN_POINT('',(4.58466185312619,2.2,29.7));
#27141=CARTESIAN_POINT('',(4.21533814687381,3.1,29.7));
#27142=CARTESIAN_POINT('Origin',(4.4,3.1,29.8));
#27143=CARTESIAN_POINT('',(4.21533814687381,3.2,29.7));
#27144=CARTESIAN_POINT('',(4.21533814687381,2.2,29.7));
#27145=CARTESIAN_POINT('Origin',(4.4,3.2,29.8));
#27146=CARTESIAN_POINT('Origin',(4.4,3.2,29.8));
#27147=CARTESIAN_POINT('',(6.4,3.2,29.7));
#27148=CARTESIAN_POINT('Origin',(7.6,2.2,29.8));
#27149=CARTESIAN_POINT('',(7.39,2.3,29.8));
#27150=CARTESIAN_POINT('Origin',(7.6,2.3,29.8));
#27151=CARTESIAN_POINT('',(7.39,3.2,29.8));
#27152=CARTESIAN_POINT('',(7.39,2.2,29.8));
#27153=CARTESIAN_POINT('',(7.78466185312619,3.2,29.7));
#27154=CARTESIAN_POINT('Origin',(7.6,3.2,29.8));
#27155=CARTESIAN_POINT('',(7.78466185312619,3.1,29.7));
#27156=CARTESIAN_POINT('',(7.78466185312619,2.2,29.7));
#27157=CARTESIAN_POINT('',(7.4153381468738,3.1,29.7));
#27158=CARTESIAN_POINT('Origin',(7.6,3.1,29.8));
#27159=CARTESIAN_POINT('',(7.41533814687381,3.2,29.7));
#27160=CARTESIAN_POINT('',(7.41533814687381,2.2,29.7));
#27161=CARTESIAN_POINT('Origin',(7.6,3.2,29.8));
#27162=CARTESIAN_POINT('Origin',(7.6,3.2,29.8));
#27163=CARTESIAN_POINT('',(8.,3.2,29.7));
#27164=CARTESIAN_POINT('Origin',(8.4,3.1,28.));
#27165=CARTESIAN_POINT('',(8.4,3.1,29.7));
#27166=CARTESIAN_POINT('',(8.4,3.1,29.7));
#27167=CARTESIAN_POINT('',(8.4,3.1,29.7));
#27168=CARTESIAN_POINT('',(8.4,3.1,28.));
#27169=CARTESIAN_POINT('',(8.4,3.1,28.));
#27170=CARTESIAN_POINT('',(3.6,3.1,28.));
#27171=CARTESIAN_POINT('',(8.4,3.1,28.));
#27172=CARTESIAN_POINT('',(3.6,3.1,29.7));
#27173=CARTESIAN_POINT('',(3.6,3.1,28.));
#27174=CARTESIAN_POINT('',(8.4,3.1,29.7));
#27175=CARTESIAN_POINT('Origin',(8.4,2.3,29.7));
#27176=CARTESIAN_POINT('',(3.6,7.,29.7));
#27177=CARTESIAN_POINT('',(3.6,2.3,29.7));
#27178=CARTESIAN_POINT('',(8.4,7.,29.7));
#27179=CARTESIAN_POINT('',(3.6,7.,29.7));
#27180=CARTESIAN_POINT('',(8.4,2.3,29.7));
#27181=CARTESIAN_POINT('Origin',(6.,7.,30.1));
#27182=CARTESIAN_POINT('',(3.6,7.,30.5));
#27183=CARTESIAN_POINT('',(8.4,7.,30.5));
#27184=CARTESIAN_POINT('',(8.4,7.,30.5));
#27185=CARTESIAN_POINT('',(8.4,7.,29.7));
#27186=CARTESIAN_POINT('',(3.6,7.,30.5));
#27187=CARTESIAN_POINT('Origin',(8.4,2.3,28.));
#27188=CARTESIAN_POINT('',(8.4,2.3,28.));
#27189=CARTESIAN_POINT('',(8.4,2.3,30.5));
#27190=CARTESIAN_POINT('',(8.4,2.3,28.));
#27191=CARTESIAN_POINT('',(8.4,2.3,28.));
#27192=CARTESIAN_POINT('',(8.4,2.3,30.5));
#27193=CARTESIAN_POINT('Origin',(3.6,2.3,28.));
#27194=CARTESIAN_POINT('',(3.6,2.3,28.));
#27195=CARTESIAN_POINT('',(3.6,2.3,30.5));
#27196=CARTESIAN_POINT('',(3.6,2.3,28.));
#27197=CARTESIAN_POINT('',(3.6,2.3,28.));
#27198=CARTESIAN_POINT('',(3.6,2.3,30.5));
#27199=CARTESIAN_POINT('Origin',(3.6,3.1,28.));
#27200=CARTESIAN_POINT('',(3.6,3.1,28.));
#27201=CARTESIAN_POINT('',(3.6,2.3,30.5));
#27202=CARTESIAN_POINT('Origin',(6.,2.7,30.5));
#27203=CARTESIAN_POINT('Origin',(6.,2.7,28.));
#27204=CARTESIAN_POINT('',(0.,0.,0.));
#27205=CARTESIAN_POINT('Origin',(2.1,5.,1.9));
#27206=CARTESIAN_POINT('',(1.935,5.,2.));
#27207=CARTESIAN_POINT('Origin',(2.1,5.,2.));
#27208=CARTESIAN_POINT('',(1.935,5.,4.));
#27209=CARTESIAN_POINT('',(1.935,5.,1.9));
#27210=CARTESIAN_POINT('Origin',(2.1,5.,4.));
#27211=CARTESIAN_POINT('Origin',(-1.05,6.81865334794732,1.9));
#27212=CARTESIAN_POINT('',(-1.215,6.81865334794732,2.));
#27213=CARTESIAN_POINT('Origin',(-1.05,6.81865334794732,2.));
#27214=CARTESIAN_POINT('',(-1.215,6.81865334794732,4.));
#27215=CARTESIAN_POINT('',(-1.215,6.81865334794732,1.9));
#27216=CARTESIAN_POINT('Origin',(-1.05,6.81865334794732,4.));
#27217=CARTESIAN_POINT('Origin',(-1.05,3.18134665205268,1.9));
#27218=CARTESIAN_POINT('',(-1.215,3.18134665205268,2.));
#27219=CARTESIAN_POINT('Origin',(-1.05,3.18134665205268,2.));
#27220=CARTESIAN_POINT('',(-1.215,3.18134665205268,4.));
#27221=CARTESIAN_POINT('',(-1.215,3.18134665205268,1.9));
#27222=CARTESIAN_POINT('Origin',(-1.05,3.18134665205268,4.));
#27223=CARTESIAN_POINT('Origin',(2.5,2.5,-0.1));
#27224=CARTESIAN_POINT('',(2.29,2.5,0.));
#27225=CARTESIAN_POINT('Origin',(2.5,2.5,0.));
#27226=CARTESIAN_POINT('',(2.29,2.5,1.1));
#27227=CARTESIAN_POINT('',(2.29,2.5,-0.1));
#27228=CARTESIAN_POINT('Origin',(2.5,2.5,1.1));
#27229=CARTESIAN_POINT('Origin',(2.5,2.5,1.1));
#27230=CARTESIAN_POINT('Origin',(-2.5,7.5,-0.1));
#27231=CARTESIAN_POINT('',(-2.71,7.5,0.));
#27232=CARTESIAN_POINT('Origin',(-2.5,7.5,0.));
#27233=CARTESIAN_POINT('',(-2.71,7.5,1.1));
#27234=CARTESIAN_POINT('',(-2.71,7.5,-0.1));
#27235=CARTESIAN_POINT('Origin',(-2.5,7.5,1.1));
#27236=CARTESIAN_POINT('Origin',(-2.5,7.5,1.1));
#27237=CARTESIAN_POINT('Origin',(-2.5,2.5,-0.1));
#27238=CARTESIAN_POINT('',(-2.71,2.5,0.));
#27239=CARTESIAN_POINT('Origin',(-2.5,2.5,0.));
#27240=CARTESIAN_POINT('',(-2.71,2.5,1.1));
#27241=CARTESIAN_POINT('',(-2.71,2.5,-0.1));
#27242=CARTESIAN_POINT('Origin',(-2.5,2.5,1.1));
#27243=CARTESIAN_POINT('Origin',(-2.5,2.5,1.1));
#27244=CARTESIAN_POINT('Origin',(2.5,7.5,-0.1));
#27245=CARTESIAN_POINT('',(2.29,7.5,0.));
#27246=CARTESIAN_POINT('Origin',(2.5,7.5,0.));
#27247=CARTESIAN_POINT('',(2.29,7.5,1.1));
#27248=CARTESIAN_POINT('',(2.29,7.5,-0.1));
#27249=CARTESIAN_POINT('Origin',(2.5,7.5,1.1));
#27250=CARTESIAN_POINT('Origin',(2.5,7.5,1.1));
#27251=CARTESIAN_POINT('Origin',(0.,5.,1.9));
#27252=CARTESIAN_POINT('',(-1.6,5.,2.));
#27253=CARTESIAN_POINT('Origin',(0.,5.,2.));
#27254=CARTESIAN_POINT('',(-1.6,5.,3.5));
#27255=CARTESIAN_POINT('',(-1.6,5.,1.9));
#27256=CARTESIAN_POINT('Origin',(0.,5.,3.5));
#27257=CARTESIAN_POINT('Origin',(0.,5.,3.5));
#27258=CARTESIAN_POINT('',(-1.4,5.,3.5));
#27259=CARTESIAN_POINT('Origin',(0.,5.,3.5));
#27260=CARTESIAN_POINT('Origin',(0.,5.,1.9));
#27261=CARTESIAN_POINT('',(-1.4,5.,4.));
#27262=CARTESIAN_POINT('',(-1.4,5.,1.9));
#27263=CARTESIAN_POINT('Origin',(0.,5.,4.));
#27264=CARTESIAN_POINT('Origin',(0.,5.,-0.1));
#27265=CARTESIAN_POINT('',(-2.5,5.,0.));
#27266=CARTESIAN_POINT('Origin',(0.,5.,0.));
#27267=CARTESIAN_POINT('',(-2.5,5.,2.));
#27268=CARTESIAN_POINT('',(-2.5,5.,-0.1));
#27269=CARTESIAN_POINT('Origin',(0.,5.,2.));
#27270=CARTESIAN_POINT('Origin',(0.,5.,2.));
#27271=CARTESIAN_POINT('Origin',(3.,8.,0.));
#27272=CARTESIAN_POINT('',(3.,8.,0.));
#27273=CARTESIAN_POINT('',(-3.,8.,0.));
#27274=CARTESIAN_POINT('',(3.,8.,0.));
#27275=CARTESIAN_POINT('',(-3.,8.,4.));
#27276=CARTESIAN_POINT('',(-3.,8.,0.));
#27277=CARTESIAN_POINT('',(3.,8.,4.));
#27278=CARTESIAN_POINT('',(3.,8.,4.));
#27279=CARTESIAN_POINT('',(3.,8.,0.));
#27280=CARTESIAN_POINT('Origin',(3.,2.,0.));
#27281=CARTESIAN_POINT('',(3.,2.,0.));
#27282=CARTESIAN_POINT('',(3.,2.,0.));
#27283=CARTESIAN_POINT('',(3.,2.,4.));
#27284=CARTESIAN_POINT('',(3.,2.,4.));
#27285=CARTESIAN_POINT('',(3.,2.,0.));
#27286=CARTESIAN_POINT('Origin',(-3.,2.,0.));
#27287=CARTESIAN_POINT('',(-3.,2.,0.));
#27288=CARTESIAN_POINT('',(-3.,2.,0.));
#27289=CARTESIAN_POINT('',(-3.,2.,4.));
#27290=CARTESIAN_POINT('',(-3.,2.,4.));
#27291=CARTESIAN_POINT('',(-3.,2.,0.));
#27292=CARTESIAN_POINT('Origin',(-3.,8.,0.));
#27293=CARTESIAN_POINT('',(-3.,8.,0.));
#27294=CARTESIAN_POINT('',(-3.,8.,4.));
#27295=CARTESIAN_POINT('Origin',(0.,5.,4.));
#27296=CARTESIAN_POINT('Origin',(0.,5.,0.));
#27297=CARTESIAN_POINT('',(0.,0.,0.));
#27298=CARTESIAN_POINT('Origin',(6.,5.,22.9));
#27299=CARTESIAN_POINT('',(5.725,5.,23.));
#27300=CARTESIAN_POINT('Origin',(6.,5.,23.));
#27301=CARTESIAN_POINT('',(5.725,5.,25.));
#27302=CARTESIAN_POINT('',(5.725,5.,22.9));
#27303=CARTESIAN_POINT('Origin',(6.,5.,25.));
#27304=CARTESIAN_POINT('Origin',(-6.,5.,22.9));
#27305=CARTESIAN_POINT('',(-6.275,5.,23.));
#27306=CARTESIAN_POINT('Origin',(-6.,5.,23.));
#27307=CARTESIAN_POINT('',(-6.275,5.,25.));
#27308=CARTESIAN_POINT('',(-6.275,5.,22.9));
#27309=CARTESIAN_POINT('Origin',(-6.,5.,25.));
#27310=CARTESIAN_POINT('Origin',(2.6,5.,22.9));
#27311=CARTESIAN_POINT('',(2.435,5.,23.));
#27312=CARTESIAN_POINT('Origin',(2.6,5.,23.));
#27313=CARTESIAN_POINT('',(2.435,5.,25.));
#27314=CARTESIAN_POINT('',(2.435,5.,22.9));
#27315=CARTESIAN_POINT('Origin',(2.6,5.,25.));
#27316=CARTESIAN_POINT('Origin',(-1.3,7.25166604983954,22.9));
#27317=CARTESIAN_POINT('',(-1.465,7.25166604983954,23.));
#27318=CARTESIAN_POINT('Origin',(-1.3,7.25166604983954,23.));
#27319=CARTESIAN_POINT('',(-1.465,7.25166604983954,25.));
#27320=CARTESIAN_POINT('',(-1.465,7.25166604983954,22.9));
#27321=CARTESIAN_POINT('Origin',(-1.3,7.25166604983954,25.));
#27322=CARTESIAN_POINT('Origin',(-1.3,2.74833395016046,22.9));
#27323=CARTESIAN_POINT('',(-1.465,2.74833395016046,23.));
#27324=CARTESIAN_POINT('Origin',(-1.3,2.74833395016046,23.));
#27325=CARTESIAN_POINT('',(-1.465,2.74833395016046,25.));
#27326=CARTESIAN_POINT('',(-1.465,2.74833395016046,22.9));
#27327=CARTESIAN_POINT('Origin',(-1.3,2.74833395016046,25.));
#27328=CARTESIAN_POINT('Origin',(5.4,9.5,24.));
#27329=CARTESIAN_POINT('',(5.4,9.5,24.21));
#27330=CARTESIAN_POINT('Origin',(5.4,9.5,24.));
#27331=CARTESIAN_POINT('',(6.5,9.5,24.21));
#27332=CARTESIAN_POINT('',(5.4,9.5,24.21));
#27333=CARTESIAN_POINT('Origin',(6.5,9.5,24.));
#27334=CARTESIAN_POINT('Origin',(5.4,9.5,24.));
#27335=CARTESIAN_POINT('Origin',(5.4,10.5,24.));
#27336=CARTESIAN_POINT('',(5.4,10.5,24.21));
#27337=CARTESIAN_POINT('Origin',(5.4,10.5,24.));
#27338=CARTESIAN_POINT('',(6.5,10.5,24.21));
#27339=CARTESIAN_POINT('',(5.4,10.5,24.21));
#27340=CARTESIAN_POINT('Origin',(6.5,10.5,24.));
#27341=CARTESIAN_POINT('Origin',(5.4,10.5,24.));
#27342=CARTESIAN_POINT('Origin',(-6.6,9.5,24.));
#27343=CARTESIAN_POINT('',(-6.5,9.5,24.21));
#27344=CARTESIAN_POINT('Origin',(-6.5,9.5,24.));
#27345=CARTESIAN_POINT('',(-5.4,9.5,24.21));
#27346=CARTESIAN_POINT('',(-6.6,9.5,24.21));
#27347=CARTESIAN_POINT('Origin',(-5.4,9.5,24.));
#27348=CARTESIAN_POINT('Origin',(-5.4,9.5,24.));
#27349=CARTESIAN_POINT('Origin',(-6.6,10.5,24.));
#27350=CARTESIAN_POINT('',(-6.5,10.5,24.21));
#27351=CARTESIAN_POINT('Origin',(-6.5,10.5,24.));
#27352=CARTESIAN_POINT('',(-5.4,10.5,24.21));
#27353=CARTESIAN_POINT('',(-6.6,10.5,24.21));
#27354=CARTESIAN_POINT('Origin',(-5.4,10.5,24.));
#27355=CARTESIAN_POINT('Origin',(-5.4,10.5,24.));
#27356=CARTESIAN_POINT('Origin',(0.,5.,23.3));
#27357=CARTESIAN_POINT('',(-2.35,5.,23.3));
#27358=CARTESIAN_POINT('Origin',(0.,5.,23.3));
#27359=CARTESIAN_POINT('',(-2.35,5.,25.));
#27360=CARTESIAN_POINT('',(-2.35,5.,23.3));
#27361=CARTESIAN_POINT('Origin',(0.,5.,25.));
#27362=CARTESIAN_POINT('Origin',(0.,5.,23.3));
#27363=CARTESIAN_POINT('',(-2.15,5.,23.3));
#27364=CARTESIAN_POINT('Origin',(0.,5.,23.3));
#27365=CARTESIAN_POINT('Origin',(0.,5.,22.9));
#27366=CARTESIAN_POINT('',(-2.15,5.,23.));
#27367=CARTESIAN_POINT('Origin',(0.,5.,23.));
#27368=CARTESIAN_POINT('',(-2.15,5.,22.9));
#27369=CARTESIAN_POINT('Origin',(-6.,0.,22.9));
#27370=CARTESIAN_POINT('',(-6.5,0.375,23.));
#27371=CARTESIAN_POINT('',(-6.5,0.375,25.));
#27372=CARTESIAN_POINT('',(-6.5,0.375,22.9));
#27373=CARTESIAN_POINT('',(-5.375,0.,23.));
#27374=CARTESIAN_POINT('Origin',(-6.,0.,23.));
#27375=CARTESIAN_POINT('',(-5.375,0.,25.));
#27376=CARTESIAN_POINT('',(-5.375,0.,22.9));
#27377=CARTESIAN_POINT('Origin',(-6.,0.,25.));
#27378=CARTESIAN_POINT('Origin',(6.,0.,22.9));
#27379=CARTESIAN_POINT('',(5.375,0.,23.));
#27380=CARTESIAN_POINT('',(5.375,0.,25.));
#27381=CARTESIAN_POINT('',(5.375,0.,22.9));
#27382=CARTESIAN_POINT('',(6.5,0.375,23.));
#27383=CARTESIAN_POINT('Origin',(6.,0.,23.));
#27384=CARTESIAN_POINT('',(6.5,0.375,25.));
#27385=CARTESIAN_POINT('',(6.5,0.375,22.9));
#27386=CARTESIAN_POINT('Origin',(6.,0.,25.));
#27387=CARTESIAN_POINT('Origin',(6.5,0.,23.));
#27388=CARTESIAN_POINT('',(6.5,11.,23.));
#27389=CARTESIAN_POINT('',(6.5,0.,23.));
#27390=CARTESIAN_POINT('',(6.5,11.,25.));
#27391=CARTESIAN_POINT('',(6.5,11.,23.));
#27392=CARTESIAN_POINT('',(6.5,0.,25.));
#27393=CARTESIAN_POINT('Origin',(0.,5.5,23.));
#27394=CARTESIAN_POINT('',(-6.5,11.,23.));
#27395=CARTESIAN_POINT('',(-6.5,11.,23.));
#27396=CARTESIAN_POINT('',(6.5,11.,23.));
#27397=CARTESIAN_POINT('',(-6.5,0.,23.));
#27398=CARTESIAN_POINT('Origin',(-6.5,0.,23.));
#27399=CARTESIAN_POINT('',(-6.5,0.,25.));
#27400=CARTESIAN_POINT('Origin',(6.5,11.,23.));
#27401=CARTESIAN_POINT('',(-6.5,11.,25.));
#27402=CARTESIAN_POINT('',(-6.5,11.,23.));
#27403=CARTESIAN_POINT('',(6.5,11.,25.));
#27404=CARTESIAN_POINT('Origin',(-6.5,11.,23.));
#27405=CARTESIAN_POINT('',(-6.5,11.,25.));
#27406=CARTESIAN_POINT('Origin',(0.,5.5,25.));
#27407=CARTESIAN_POINT('',(0.,0.,0.));
#27408=CARTESIAN_POINT('Origin',(2.1,5.,1.5));
#27409=CARTESIAN_POINT('',(1.875,5.,1.6));
#27410=CARTESIAN_POINT('Origin',(2.1,5.,1.6));
#27411=CARTESIAN_POINT('',(1.875,5.,2.));
#27412=CARTESIAN_POINT('',(1.875,5.,1.5));
#27413=CARTESIAN_POINT('Origin',(2.1,5.,2.));
#27414=CARTESIAN_POINT('Origin',(-1.05,6.81865334794732,1.5));
#27415=CARTESIAN_POINT('',(-1.275,6.81865334794732,1.6));
#27416=CARTESIAN_POINT('Origin',(-1.05,6.81865334794732,1.6));
#27417=CARTESIAN_POINT('',(-1.275,6.81865334794732,2.));
#27418=CARTESIAN_POINT('',(-1.275,6.81865334794732,1.5));
#27419=CARTESIAN_POINT('Origin',(-1.05,6.81865334794732,2.));
#27420=CARTESIAN_POINT('Origin',(-1.05,3.18134665205268,1.5));
#27421=CARTESIAN_POINT('',(-1.275,3.18134665205268,1.6));
#27422=CARTESIAN_POINT('Origin',(-1.05,3.18134665205268,1.6));
#27423=CARTESIAN_POINT('',(-1.275,3.18134665205268,2.));
#27424=CARTESIAN_POINT('',(-1.275,3.18134665205268,1.5));
#27425=CARTESIAN_POINT('Origin',(-1.05,3.18134665205268,2.));
#27426=CARTESIAN_POINT('Origin',(0.,5.,2.));
#27427=CARTESIAN_POINT('',(-1.59,5.,2.5));
#27428=CARTESIAN_POINT('Origin',(0.,5.,2.5));
#27429=CARTESIAN_POINT('',(-1.59,5.,2.));
#27430=CARTESIAN_POINT('',(-1.59,5.,2.));
#27431=CARTESIAN_POINT('Origin',(0.,5.,2.));
#27432=CARTESIAN_POINT('Origin',(0.,5.,2.5));
#27433=CARTESIAN_POINT('',(-1.2,5.,2.5));
#27434=CARTESIAN_POINT('Origin',(0.,5.,2.5));
#27435=CARTESIAN_POINT('Origin',(0.,5.,1.6));
#27436=CARTESIAN_POINT('',(-1.2,5.,1.6));
#27437=CARTESIAN_POINT('',(-1.2,5.,1.6));
#27438=CARTESIAN_POINT('Origin',(0.,5.,1.6));
#27439=CARTESIAN_POINT('Origin',(0.,5.,1.6));
#27440=CARTESIAN_POINT('',(-2.4,5.,2.));
#27441=CARTESIAN_POINT('Origin',(0.,5.,2.));
#27442=CARTESIAN_POINT('',(-2.4,5.,1.6));
#27443=CARTESIAN_POINT('',(-2.4,5.,1.6));
#27444=CARTESIAN_POINT('Origin',(0.,5.,1.6));
#27445=CARTESIAN_POINT('Origin',(0.,5.,2.));
#27446=CARTESIAN_POINT('Origin',(0.,5.,1.6));
#27447=CARTESIAN_POINT('',(0.,0.,0.));
#27448=CARTESIAN_POINT('Origin',(2.6,5.,24.9));
#27449=CARTESIAN_POINT('',(2.375,5.,25.));
#27450=CARTESIAN_POINT('Origin',(2.6,5.,25.));
#27451=CARTESIAN_POINT('',(2.375,5.,25.4));
#27452=CARTESIAN_POINT('',(2.375,5.,24.9));
#27453=CARTESIAN_POINT('Origin',(2.6,5.,25.4));
#27454=CARTESIAN_POINT('Origin',(-1.3,7.25166604983954,24.9));
#27455=CARTESIAN_POINT('',(-1.525,7.25166604983954,25.));
#27456=CARTESIAN_POINT('Origin',(-1.3,7.25166604983954,25.));
#27457=CARTESIAN_POINT('',(-1.525,7.25166604983954,25.4));
#27458=CARTESIAN_POINT('',(-1.525,7.25166604983954,24.9));
#27459=CARTESIAN_POINT('Origin',(-1.3,7.25166604983954,25.4));
#27460=CARTESIAN_POINT('Origin',(-1.3,2.74833395016046,24.9));
#27461=CARTESIAN_POINT('',(-1.525,2.74833395016046,25.));
#27462=CARTESIAN_POINT('Origin',(-1.3,2.74833395016046,25.));
#27463=CARTESIAN_POINT('',(-1.525,2.74833395016046,25.4));
#27464=CARTESIAN_POINT('',(-1.525,2.74833395016046,24.9));
#27465=CARTESIAN_POINT('Origin',(-1.3,2.74833395016046,25.4));
#27466=CARTESIAN_POINT('Origin',(0.,5.,24.7));
#27467=CARTESIAN_POINT('',(-2.34,5.,25.));
#27468=CARTESIAN_POINT('Origin',(0.,5.,25.));
#27469=CARTESIAN_POINT('',(-2.34,5.,24.7));
#27470=CARTESIAN_POINT('',(-2.34,5.,24.7));
#27471=CARTESIAN_POINT('Origin',(0.,5.,24.7));
#27472=CARTESIAN_POINT('Origin',(0.,5.,24.7));
#27473=CARTESIAN_POINT('',(-1.8,5.,24.7));
#27474=CARTESIAN_POINT('Origin',(0.,5.,24.7));
#27475=CARTESIAN_POINT('Origin',(0.,5.,25.));
#27476=CARTESIAN_POINT('',(-1.8,5.,25.4));
#27477=CARTESIAN_POINT('Origin',(0.,5.,25.4));
#27478=CARTESIAN_POINT('',(-1.8,5.,25.));
#27479=CARTESIAN_POINT('Origin',(0.,5.,25.));
#27480=CARTESIAN_POINT('',(-3.,5.,25.4));
#27481=CARTESIAN_POINT('Origin',(0.,5.,25.4));
#27482=CARTESIAN_POINT('',(-3.,5.,25.));
#27483=CARTESIAN_POINT('',(-3.,5.,25.));
#27484=CARTESIAN_POINT('Origin',(0.,5.,25.));
#27485=CARTESIAN_POINT('Origin',(0.,5.,25.4));
#27486=CARTESIAN_POINT('Origin',(0.,5.,25.));
#27487=CARTESIAN_POINT('',(0.,0.,0.));
#27488=CARTESIAN_POINT('Origin',(-6.,5.,-0.1));
#27489=CARTESIAN_POINT('',(-6.21,5.,0.));
#27490=CARTESIAN_POINT('Origin',(-6.,5.,0.));
#27491=CARTESIAN_POINT('',(-6.21,5.,1.1));
#27492=CARTESIAN_POINT('',(-6.21,5.,-0.1));
#27493=CARTESIAN_POINT('Origin',(-6.,5.,1.1));
#27494=CARTESIAN_POINT('Origin',(-6.,5.,1.1));
#27495=CARTESIAN_POINT('Origin',(-6.,5.,0.));
#27496=CARTESIAN_POINT('',(-6.5,5.,9.1));
#27497=CARTESIAN_POINT('Origin',(-6.,5.,9.1));
#27498=CARTESIAN_POINT('',(-6.5,5.,0.));
#27499=CARTESIAN_POINT('',(-6.5,5.,0.));
#27500=CARTESIAN_POINT('Origin',(-6.,5.,0.));
#27501=CARTESIAN_POINT('Origin',(-6.,5.,9.1));
#27502=CARTESIAN_POINT('Origin',(-6.,5.,0.));
#27503=CARTESIAN_POINT('',(0.,0.,0.));
#27504=CARTESIAN_POINT('Origin',(-6.,5.,22.4));
#27505=CARTESIAN_POINT('',(-6.21,5.,22.4));
#27506=CARTESIAN_POINT('Origin',(-6.,5.,22.4));
#27507=CARTESIAN_POINT('',(-6.21,5.,23.));
#27508=CARTESIAN_POINT('',(-6.21,5.,22.4));
#27509=CARTESIAN_POINT('Origin',(-6.,5.,23.));
#27510=CARTESIAN_POINT('Origin',(-6.,5.,22.4));
#27511=CARTESIAN_POINT('Origin',(-6.,5.,22.3));
#27512=CARTESIAN_POINT('',(-6.5,5.,23.));
#27513=CARTESIAN_POINT('Origin',(-6.,5.,23.));
#27514=CARTESIAN_POINT('',(-6.5,5.,22.3));
#27515=CARTESIAN_POINT('',(-6.5,5.,22.3));
#27516=CARTESIAN_POINT('Origin',(-6.,5.,22.3));
#27517=CARTESIAN_POINT('Origin',(-6.,5.,23.));
#27518=CARTESIAN_POINT('Origin',(-6.,5.,22.3));
#27519=CARTESIAN_POINT('',(0.,0.,0.));
#27520=CARTESIAN_POINT('Origin',(6.,5.,-0.1));
#27521=CARTESIAN_POINT('',(5.79,5.,0.));
#27522=CARTESIAN_POINT('Origin',(6.,5.,0.));
#27523=CARTESIAN_POINT('',(5.79,5.,1.1));
#27524=CARTESIAN_POINT('',(5.79,5.,-0.1));
#27525=CARTESIAN_POINT('Origin',(6.,5.,1.1));
#27526=CARTESIAN_POINT('Origin',(6.,5.,1.1));
#27527=CARTESIAN_POINT('Origin',(6.,5.,0.));
#27528=CARTESIAN_POINT('',(5.5,5.,9.1));
#27529=CARTESIAN_POINT('Origin',(6.,5.,9.1));
#27530=CARTESIAN_POINT('',(5.5,5.,0.));
#27531=CARTESIAN_POINT('',(5.5,5.,0.));
#27532=CARTESIAN_POINT('Origin',(6.,5.,0.));
#27533=CARTESIAN_POINT('Origin',(6.,5.,9.1));
#27534=CARTESIAN_POINT('Origin',(6.,5.,0.));
#27535=CARTESIAN_POINT('',(0.,0.,0.));
#27536=CARTESIAN_POINT('Origin',(6.,5.,22.4));
#27537=CARTESIAN_POINT('',(5.79,5.,22.4));
#27538=CARTESIAN_POINT('Origin',(6.,5.,22.4));
#27539=CARTESIAN_POINT('',(5.79,5.,23.));
#27540=CARTESIAN_POINT('',(5.79,5.,22.4));
#27541=CARTESIAN_POINT('Origin',(6.,5.,23.));
#27542=CARTESIAN_POINT('Origin',(6.,5.,22.4));
#27543=CARTESIAN_POINT('Origin',(6.,5.,22.3));
#27544=CARTESIAN_POINT('',(5.5,5.,23.));
#27545=CARTESIAN_POINT('Origin',(6.,5.,23.));
#27546=CARTESIAN_POINT('',(5.5,5.,22.3));
#27547=CARTESIAN_POINT('',(5.5,5.,22.3));
#27548=CARTESIAN_POINT('Origin',(6.,5.,22.3));
#27549=CARTESIAN_POINT('Origin',(6.,5.,23.));
#27550=CARTESIAN_POINT('Origin',(6.,5.,22.3));
#27551=CARTESIAN_POINT('',(0.,0.,0.));
#27552=CARTESIAN_POINT('Origin',(-2.5,-1.5,0.4));
#27553=CARTESIAN_POINT('',(-2.875,-1.5,0.4));
#27554=CARTESIAN_POINT('Origin',(-2.5,-1.5,0.4));
#27555=CARTESIAN_POINT('',(-2.875,-1.5,0.8));
#27556=CARTESIAN_POINT('',(-2.875,-1.5,0.4));
#27557=CARTESIAN_POINT('Origin',(-2.5,-1.5,0.8));
#27558=CARTESIAN_POINT('Origin',(-2.5,-1.5,0.4));
#27559=CARTESIAN_POINT('',(-2.725,-1.5,0.4));
#27560=CARTESIAN_POINT('Origin',(-2.5,-1.5,0.4));
#27561=CARTESIAN_POINT('Origin',(1.53080849893419E-16,1.,0.4));
#27562=CARTESIAN_POINT('',(-0.375,1.,0.4));
#27563=CARTESIAN_POINT('Origin',(1.53080849893419E-16,1.,0.4));
#27564=CARTESIAN_POINT('',(-0.375,1.,0.8));
#27565=CARTESIAN_POINT('',(-0.375,1.,0.4));
#27566=CARTESIAN_POINT('Origin',(1.53080849893419E-16,1.,0.8));
#27567=CARTESIAN_POINT('Origin',(1.66533453693773E-16,1.,0.4));
#27568=CARTESIAN_POINT('',(-0.225,1.,0.4));
#27569=CARTESIAN_POINT('Origin',(1.53080849893419E-16,1.,0.4));
#27570=CARTESIAN_POINT('Origin',(2.5,-1.5,0.4));
#27571=CARTESIAN_POINT('',(2.125,-1.5,0.4));
#27572=CARTESIAN_POINT('Origin',(2.5,-1.5,0.4));
#27573=CARTESIAN_POINT('',(2.125,-1.5,0.8));
#27574=CARTESIAN_POINT('',(2.125,-1.5,0.4));
#27575=CARTESIAN_POINT('Origin',(2.5,-1.5,0.8));
#27576=CARTESIAN_POINT('Origin',(2.5,-1.5,0.4));
#27577=CARTESIAN_POINT('',(2.275,-1.5,0.4));
#27578=CARTESIAN_POINT('Origin',(2.5,-1.5,0.4));
#27579=CARTESIAN_POINT('Origin',(-4.59242549680257E-16,-4.,0.4));
#27580=CARTESIAN_POINT('',(-0.375,-4.,0.4));
#27581=CARTESIAN_POINT('Origin',(-4.59242549680257E-16,-4.,0.4));
#27582=CARTESIAN_POINT('',(-0.375,-4.,0.8));
#27583=CARTESIAN_POINT('',(-0.375,-4.,0.4));
#27584=CARTESIAN_POINT('Origin',(-4.59242549680257E-16,-4.,0.8));
#27585=CARTESIAN_POINT('Origin',(-4.44089209850063E-16,-4.,0.4));
#27586=CARTESIAN_POINT('',(-0.225,-4.,0.4));
#27587=CARTESIAN_POINT('Origin',(-4.59242549680257E-16,-4.,0.4));
#27588=CARTESIAN_POINT('Origin',(-2.5,-1.5,-0.1));
#27589=CARTESIAN_POINT('',(-2.725,-1.5,0.));
#27590=CARTESIAN_POINT('Origin',(-2.5,-1.5,0.));
#27591=CARTESIAN_POINT('',(-2.725,-1.5,-0.1));
#27592=CARTESIAN_POINT('Origin',(1.53080849893419E-16,1.,-0.1));
#27593=CARTESIAN_POINT('',(-0.225,1.,0.));
#27594=CARTESIAN_POINT('Origin',(1.53080849893419E-16,1.,0.));
#27595=CARTESIAN_POINT('',(-0.225,1.,-0.1));
#27596=CARTESIAN_POINT('Origin',(2.5,-1.5,-0.1));
#27597=CARTESIAN_POINT('',(2.275,-1.5,0.));
#27598=CARTESIAN_POINT('Origin',(2.5,-1.5,0.));
#27599=CARTESIAN_POINT('',(2.275,-1.5,-0.1));
#27600=CARTESIAN_POINT('Origin',(-4.59242549680257E-16,-4.,-0.1));
#27601=CARTESIAN_POINT('',(-0.225,-4.,0.));
#27602=CARTESIAN_POINT('Origin',(-4.59242549680257E-16,-4.,0.));
#27603=CARTESIAN_POINT('',(-0.225,-4.,-0.1));
#27604=CARTESIAN_POINT('Origin',(0.,-1.5,0.));
#27605=CARTESIAN_POINT('',(-3.,-1.5,0.8));
#27606=CARTESIAN_POINT('Origin',(0.,-1.5,0.8));
#27607=CARTESIAN_POINT('',(-3.,-1.5,0.));
#27608=CARTESIAN_POINT('',(-3.,-1.5,0.));
#27609=CARTESIAN_POINT('Origin',(0.,-1.5,0.));
#27610=CARTESIAN_POINT('Origin',(0.,-1.5,0.8));
#27611=CARTESIAN_POINT('Origin',(0.,-1.5,0.));
#27612=CARTESIAN_POINT('',(0.,0.,0.));
#27613=CARTESIAN_POINT('Origin',(8.69,-0.7,21.29));
#27614=CARTESIAN_POINT('',(8.7,-0.7,21.29));
#27615=CARTESIAN_POINT('',(8.7,0.4,21.29));
#27616=CARTESIAN_POINT('',(8.7,0.05,21.29));
#27617=CARTESIAN_POINT('',(8.75,-0.7,21.29));
#27618=CARTESIAN_POINT('',(8.69,-0.7,21.29));
#27619=CARTESIAN_POINT('',(8.75,0.4,21.29));
#27620=CARTESIAN_POINT('',(8.75,-0.7,21.29));
#27621=CARTESIAN_POINT('',(8.69,0.4,21.29));
#27622=CARTESIAN_POINT('Origin',(8.69,0.4,21.29));
#27623=CARTESIAN_POINT('',(8.7,0.4,21.31));
#27624=CARTESIAN_POINT('',(8.7,0.4,11.645));
#27625=CARTESIAN_POINT('',(8.75,0.4,21.31));
#27626=CARTESIAN_POINT('',(8.75,0.4,21.29));
#27627=CARTESIAN_POINT('',(8.69,0.4,21.31));
#27628=CARTESIAN_POINT('Origin',(8.69,0.4,21.31));
#27629=CARTESIAN_POINT('',(8.7,-0.7,21.31));
#27630=CARTESIAN_POINT('',(8.7,0.6,21.31));
#27631=CARTESIAN_POINT('',(8.75,-0.7,21.31));
#27632=CARTESIAN_POINT('',(8.75,0.4,21.31));
#27633=CARTESIAN_POINT('',(8.69,-0.7,21.31));
#27634=CARTESIAN_POINT('Origin',(8.69,-0.7,21.31));
#27635=CARTESIAN_POINT('',(8.7,-0.7,11.655));
#27636=CARTESIAN_POINT('',(8.75,-0.7,21.31));
#27637=CARTESIAN_POINT('Origin',(8.75,-0.15,21.3));
#27638=CARTESIAN_POINT('Origin',(8.69,-0.7,20.79));
#27639=CARTESIAN_POINT('',(8.7,-0.7,20.79));
#27640=CARTESIAN_POINT('',(8.7,-0.1,20.79));
#27641=CARTESIAN_POINT('',(8.7,0.05,20.79));
#27642=CARTESIAN_POINT('',(8.75,-0.7,20.79));
#27643=CARTESIAN_POINT('',(8.69,-0.7,20.79));
#27644=CARTESIAN_POINT('',(8.75,-0.1,20.79));
#27645=CARTESIAN_POINT('',(8.75,-0.7,20.79));
#27646=CARTESIAN_POINT('',(8.69,-0.1,20.79));
#27647=CARTESIAN_POINT('Origin',(8.69,-0.1,20.79));
#27648=CARTESIAN_POINT('',(8.7,-0.1,20.81));
#27649=CARTESIAN_POINT('',(8.7,-0.1,11.395));
#27650=CARTESIAN_POINT('',(8.75,-0.1,20.81));
#27651=CARTESIAN_POINT('',(8.75,-0.1,20.79));
#27652=CARTESIAN_POINT('',(8.69,-0.1,20.81));
#27653=CARTESIAN_POINT('Origin',(8.69,-0.1,20.81));
#27654=CARTESIAN_POINT('',(8.7,-0.7,20.81));
#27655=CARTESIAN_POINT('',(8.7,0.35,20.81));
#27656=CARTESIAN_POINT('',(8.75,-0.7,20.81));
#27657=CARTESIAN_POINT('',(8.75,-0.1,20.81));
#27658=CARTESIAN_POINT('',(8.69,-0.7,20.81));
#27659=CARTESIAN_POINT('Origin',(8.69,-0.7,20.81));
#27660=CARTESIAN_POINT('',(8.7,-0.7,11.405));
#27661=CARTESIAN_POINT('',(8.75,-0.7,20.81));
#27662=CARTESIAN_POINT('Origin',(8.75,-0.4,20.8));
#27663=CARTESIAN_POINT('Origin',(8.69,-0.7,20.29));
#27664=CARTESIAN_POINT('',(8.7,-0.7,20.29));
#27665=CARTESIAN_POINT('',(8.7,0.4,20.29));
#27666=CARTESIAN_POINT('',(8.7,0.05,20.29));
#27667=CARTESIAN_POINT('',(8.75,-0.7,20.29));
#27668=CARTESIAN_POINT('',(8.69,-0.7,20.29));
#27669=CARTESIAN_POINT('',(8.75,0.4,20.29));
#27670=CARTESIAN_POINT('',(8.75,-0.7,20.29));
#27671=CARTESIAN_POINT('',(8.69,0.4,20.29));
#27672=CARTESIAN_POINT('Origin',(8.69,0.4,20.29));
#27673=CARTESIAN_POINT('',(8.7,0.4,20.31));
#27674=CARTESIAN_POINT('',(8.7,0.4,11.145));
#27675=CARTESIAN_POINT('',(8.75,0.4,20.31));
#27676=CARTESIAN_POINT('',(8.75,0.4,20.29));
#27677=CARTESIAN_POINT('',(8.69,0.4,20.31));
#27678=CARTESIAN_POINT('Origin',(8.69,0.4,20.31));
#27679=CARTESIAN_POINT('',(8.7,-0.7,20.31));
#27680=CARTESIAN_POINT('',(8.7,0.6,20.31));
#27681=CARTESIAN_POINT('',(8.75,-0.7,20.31));
#27682=CARTESIAN_POINT('',(8.75,0.4,20.31));
#27683=CARTESIAN_POINT('',(8.69,-0.7,20.31));
#27684=CARTESIAN_POINT('Origin',(8.69,-0.7,20.31));
#27685=CARTESIAN_POINT('',(8.7,-0.7,11.155));
#27686=CARTESIAN_POINT('',(8.75,-0.7,20.31));
#27687=CARTESIAN_POINT('Origin',(8.75,-0.15,20.3));
#27688=CARTESIAN_POINT('Origin',(8.69,-0.7,19.79));
#27689=CARTESIAN_POINT('',(8.7,-0.7,19.79));
#27690=CARTESIAN_POINT('',(8.7,-0.1,19.79));
#27691=CARTESIAN_POINT('',(8.7,0.05,19.79));
#27692=CARTESIAN_POINT('',(8.75,-0.7,19.79));
#27693=CARTESIAN_POINT('',(8.69,-0.7,19.79));
#27694=CARTESIAN_POINT('',(8.75,-0.1,19.79));
#27695=CARTESIAN_POINT('',(8.75,-0.7,19.79));
#27696=CARTESIAN_POINT('',(8.69,-0.1,19.79));
#27697=CARTESIAN_POINT('Origin',(8.69,-0.1,19.79));
#27698=CARTESIAN_POINT('',(8.7,-0.1,19.81));
#27699=CARTESIAN_POINT('',(8.7,-0.1,10.895));
#27700=CARTESIAN_POINT('',(8.75,-0.1,19.81));
#27701=CARTESIAN_POINT('',(8.75,-0.1,19.79));
#27702=CARTESIAN_POINT('',(8.69,-0.1,19.81));
#27703=CARTESIAN_POINT('Origin',(8.69,-0.1,19.81));
#27704=CARTESIAN_POINT('',(8.7,-0.7,19.81));
#27705=CARTESIAN_POINT('',(8.7,0.35,19.81));
#27706=CARTESIAN_POINT('',(8.75,-0.7,19.81));
#27707=CARTESIAN_POINT('',(8.75,-0.1,19.81));
#27708=CARTESIAN_POINT('',(8.69,-0.7,19.81));
#27709=CARTESIAN_POINT('Origin',(8.69,-0.7,19.81));
#27710=CARTESIAN_POINT('',(8.7,-0.7,10.905));
#27711=CARTESIAN_POINT('',(8.75,-0.7,19.81));
#27712=CARTESIAN_POINT('Origin',(8.75,-0.4,19.8));
#27713=CARTESIAN_POINT('Origin',(8.69,-0.7,19.29));
#27714=CARTESIAN_POINT('',(8.7,-0.7,19.29));
#27715=CARTESIAN_POINT('',(8.7,0.4,19.29));
#27716=CARTESIAN_POINT('',(8.7,0.05,19.29));
#27717=CARTESIAN_POINT('',(8.75,-0.7,19.29));
#27718=CARTESIAN_POINT('',(8.69,-0.7,19.29));
#27719=CARTESIAN_POINT('',(8.75,0.4,19.29));
#27720=CARTESIAN_POINT('',(8.75,-0.7,19.29));
#27721=CARTESIAN_POINT('',(8.69,0.4,19.29));
#27722=CARTESIAN_POINT('Origin',(8.69,0.4,19.29));
#27723=CARTESIAN_POINT('',(8.7,0.4,19.31));
#27724=CARTESIAN_POINT('',(8.7,0.4,10.645));
#27725=CARTESIAN_POINT('',(8.75,0.4,19.31));
#27726=CARTESIAN_POINT('',(8.75,0.4,19.29));
#27727=CARTESIAN_POINT('',(8.69,0.4,19.31));
#27728=CARTESIAN_POINT('Origin',(8.69,0.4,19.31));
#27729=CARTESIAN_POINT('',(8.7,-0.7,19.31));
#27730=CARTESIAN_POINT('',(8.7,0.6,19.31));
#27731=CARTESIAN_POINT('',(8.75,-0.7,19.31));
#27732=CARTESIAN_POINT('',(8.75,0.4,19.31));
#27733=CARTESIAN_POINT('',(8.69,-0.7,19.31));
#27734=CARTESIAN_POINT('Origin',(8.69,-0.7,19.31));
#27735=CARTESIAN_POINT('',(8.7,-0.7,10.655));
#27736=CARTESIAN_POINT('',(8.75,-0.7,19.31));
#27737=CARTESIAN_POINT('Origin',(8.75,-0.15,19.3));
#27738=CARTESIAN_POINT('Origin',(8.69,-0.7,18.79));
#27739=CARTESIAN_POINT('',(8.7,-0.7,18.79));
#27740=CARTESIAN_POINT('',(8.7,-0.1,18.79));
#27741=CARTESIAN_POINT('',(8.7,0.05,18.79));
#27742=CARTESIAN_POINT('',(8.75,-0.7,18.79));
#27743=CARTESIAN_POINT('',(8.69,-0.7,18.79));
#27744=CARTESIAN_POINT('',(8.75,-0.1,18.79));
#27745=CARTESIAN_POINT('',(8.75,-0.7,18.79));
#27746=CARTESIAN_POINT('',(8.69,-0.1,18.79));
#27747=CARTESIAN_POINT('Origin',(8.69,-0.1,18.79));
#27748=CARTESIAN_POINT('',(8.7,-0.1,18.81));
#27749=CARTESIAN_POINT('',(8.7,-0.1,10.395));
#27750=CARTESIAN_POINT('',(8.75,-0.1,18.81));
#27751=CARTESIAN_POINT('',(8.75,-0.1,18.79));
#27752=CARTESIAN_POINT('',(8.69,-0.1,18.81));
#27753=CARTESIAN_POINT('Origin',(8.69,-0.1,18.81));
#27754=CARTESIAN_POINT('',(8.7,-0.7,18.81));
#27755=CARTESIAN_POINT('',(8.7,0.35,18.81));
#27756=CARTESIAN_POINT('',(8.75,-0.7,18.81));
#27757=CARTESIAN_POINT('',(8.75,-0.1,18.81));
#27758=CARTESIAN_POINT('',(8.69,-0.7,18.81));
#27759=CARTESIAN_POINT('Origin',(8.69,-0.7,18.81));
#27760=CARTESIAN_POINT('',(8.7,-0.7,10.405));
#27761=CARTESIAN_POINT('',(8.75,-0.7,18.81));
#27762=CARTESIAN_POINT('Origin',(8.75,-0.4,18.8));
#27763=CARTESIAN_POINT('Origin',(8.69,-0.7,18.29));
#27764=CARTESIAN_POINT('',(8.7,-0.7,18.29));
#27765=CARTESIAN_POINT('',(8.7,0.4,18.29));
#27766=CARTESIAN_POINT('',(8.7,0.05,18.29));
#27767=CARTESIAN_POINT('',(8.75,-0.7,18.29));
#27768=CARTESIAN_POINT('',(8.69,-0.7,18.29));
#27769=CARTESIAN_POINT('',(8.75,0.4,18.29));
#27770=CARTESIAN_POINT('',(8.75,-0.7,18.29));
#27771=CARTESIAN_POINT('',(8.69,0.4,18.29));
#27772=CARTESIAN_POINT('Origin',(8.69,0.4,18.29));
#27773=CARTESIAN_POINT('',(8.7,0.4,18.31));
#27774=CARTESIAN_POINT('',(8.7,0.4,10.145));
#27775=CARTESIAN_POINT('',(8.75,0.4,18.31));
#27776=CARTESIAN_POINT('',(8.75,0.4,18.29));
#27777=CARTESIAN_POINT('',(8.69,0.4,18.31));
#27778=CARTESIAN_POINT('Origin',(8.69,0.4,18.31));
#27779=CARTESIAN_POINT('',(8.7,-0.7,18.31));
#27780=CARTESIAN_POINT('',(8.7,0.6,18.31));
#27781=CARTESIAN_POINT('',(8.75,-0.7,18.31));
#27782=CARTESIAN_POINT('',(8.75,0.4,18.31));
#27783=CARTESIAN_POINT('',(8.69,-0.7,18.31));
#27784=CARTESIAN_POINT('Origin',(8.69,-0.7,18.31));
#27785=CARTESIAN_POINT('',(8.7,-0.7,10.155));
#27786=CARTESIAN_POINT('',(8.75,-0.7,18.31));
#27787=CARTESIAN_POINT('Origin',(8.75,-0.15,18.3));
#27788=CARTESIAN_POINT('Origin',(8.69,-0.7,17.79));
#27789=CARTESIAN_POINT('',(8.7,-0.7,17.79));
#27790=CARTESIAN_POINT('',(8.7,-0.1,17.79));
#27791=CARTESIAN_POINT('',(8.7,0.05,17.79));
#27792=CARTESIAN_POINT('',(8.75,-0.7,17.79));
#27793=CARTESIAN_POINT('',(8.69,-0.7,17.79));
#27794=CARTESIAN_POINT('',(8.75,-0.1,17.79));
#27795=CARTESIAN_POINT('',(8.75,-0.7,17.79));
#27796=CARTESIAN_POINT('',(8.69,-0.1,17.79));
#27797=CARTESIAN_POINT('Origin',(8.69,-0.1,17.79));
#27798=CARTESIAN_POINT('',(8.7,-0.1,17.81));
#27799=CARTESIAN_POINT('',(8.7,-0.1,9.895));
#27800=CARTESIAN_POINT('',(8.75,-0.1,17.81));
#27801=CARTESIAN_POINT('',(8.75,-0.1,17.79));
#27802=CARTESIAN_POINT('',(8.69,-0.1,17.81));
#27803=CARTESIAN_POINT('Origin',(8.69,-0.1,17.81));
#27804=CARTESIAN_POINT('',(8.7,-0.7,17.81));
#27805=CARTESIAN_POINT('',(8.7,0.35,17.81));
#27806=CARTESIAN_POINT('',(8.75,-0.7,17.81));
#27807=CARTESIAN_POINT('',(8.75,-0.1,17.81));
#27808=CARTESIAN_POINT('',(8.69,-0.7,17.81));
#27809=CARTESIAN_POINT('Origin',(8.69,-0.7,17.81));
#27810=CARTESIAN_POINT('',(8.7,-0.7,9.905));
#27811=CARTESIAN_POINT('',(8.75,-0.7,17.81));
#27812=CARTESIAN_POINT('Origin',(8.75,-0.4,17.8));
#27813=CARTESIAN_POINT('Origin',(8.69,-0.7,17.29));
#27814=CARTESIAN_POINT('',(8.7,-0.7,17.29));
#27815=CARTESIAN_POINT('',(8.7,0.4,17.29));
#27816=CARTESIAN_POINT('',(8.7,0.05,17.29));
#27817=CARTESIAN_POINT('',(8.75,-0.7,17.29));
#27818=CARTESIAN_POINT('',(8.69,-0.7,17.29));
#27819=CARTESIAN_POINT('',(8.75,0.4,17.29));
#27820=CARTESIAN_POINT('',(8.75,-0.7,17.29));
#27821=CARTESIAN_POINT('',(8.69,0.4,17.29));
#27822=CARTESIAN_POINT('Origin',(8.69,0.4,17.29));
#27823=CARTESIAN_POINT('',(8.7,0.4,17.31));
#27824=CARTESIAN_POINT('',(8.7,0.4,9.645));
#27825=CARTESIAN_POINT('',(8.75,0.4,17.31));
#27826=CARTESIAN_POINT('',(8.75,0.4,17.29));
#27827=CARTESIAN_POINT('',(8.69,0.4,17.31));
#27828=CARTESIAN_POINT('Origin',(8.69,0.4,17.31));
#27829=CARTESIAN_POINT('',(8.7,-0.7,17.31));
#27830=CARTESIAN_POINT('',(8.7,0.6,17.31));
#27831=CARTESIAN_POINT('',(8.75,-0.7,17.31));
#27832=CARTESIAN_POINT('',(8.75,0.4,17.31));
#27833=CARTESIAN_POINT('',(8.69,-0.7,17.31));
#27834=CARTESIAN_POINT('Origin',(8.69,-0.7,17.31));
#27835=CARTESIAN_POINT('',(8.7,-0.7,9.655));
#27836=CARTESIAN_POINT('',(8.75,-0.7,17.31));
#27837=CARTESIAN_POINT('Origin',(8.75,-0.15,17.3));
#27838=CARTESIAN_POINT('Origin',(8.69,-0.7,16.79));
#27839=CARTESIAN_POINT('',(8.7,-0.7,16.79));
#27840=CARTESIAN_POINT('',(8.7,-0.1,16.79));
#27841=CARTESIAN_POINT('',(8.7,0.05,16.79));
#27842=CARTESIAN_POINT('',(8.75,-0.7,16.79));
#27843=CARTESIAN_POINT('',(8.69,-0.7,16.79));
#27844=CARTESIAN_POINT('',(8.75,-0.1,16.79));
#27845=CARTESIAN_POINT('',(8.75,-0.7,16.79));
#27846=CARTESIAN_POINT('',(8.69,-0.1,16.79));
#27847=CARTESIAN_POINT('Origin',(8.69,-0.1,16.79));
#27848=CARTESIAN_POINT('',(8.7,-0.1,16.81));
#27849=CARTESIAN_POINT('',(8.7,-0.1,9.395));
#27850=CARTESIAN_POINT('',(8.75,-0.1,16.81));
#27851=CARTESIAN_POINT('',(8.75,-0.1,16.79));
#27852=CARTESIAN_POINT('',(8.69,-0.1,16.81));
#27853=CARTESIAN_POINT('Origin',(8.69,-0.1,16.81));
#27854=CARTESIAN_POINT('',(8.7,-0.7,16.81));
#27855=CARTESIAN_POINT('',(8.7,0.35,16.81));
#27856=CARTESIAN_POINT('',(8.75,-0.7,16.81));
#27857=CARTESIAN_POINT('',(8.75,-0.1,16.81));
#27858=CARTESIAN_POINT('',(8.69,-0.7,16.81));
#27859=CARTESIAN_POINT('Origin',(8.69,-0.7,16.81));
#27860=CARTESIAN_POINT('',(8.7,-0.7,9.405));
#27861=CARTESIAN_POINT('',(8.75,-0.7,16.81));
#27862=CARTESIAN_POINT('Origin',(8.75,-0.4,16.8));
#27863=CARTESIAN_POINT('Origin',(8.69,-0.7,16.29));
#27864=CARTESIAN_POINT('',(8.7,-0.7,16.29));
#27865=CARTESIAN_POINT('',(8.7,0.4,16.29));
#27866=CARTESIAN_POINT('',(8.7,0.05,16.29));
#27867=CARTESIAN_POINT('',(8.75,-0.7,16.29));
#27868=CARTESIAN_POINT('',(8.69,-0.7,16.29));
#27869=CARTESIAN_POINT('',(8.75,0.4,16.29));
#27870=CARTESIAN_POINT('',(8.75,-0.7,16.29));
#27871=CARTESIAN_POINT('',(8.69,0.4,16.29));
#27872=CARTESIAN_POINT('Origin',(8.69,0.4,16.29));
#27873=CARTESIAN_POINT('',(8.7,0.4,16.31));
#27874=CARTESIAN_POINT('',(8.7,0.4,9.145));
#27875=CARTESIAN_POINT('',(8.75,0.4,16.31));
#27876=CARTESIAN_POINT('',(8.75,0.4,16.29));
#27877=CARTESIAN_POINT('',(8.69,0.4,16.31));
#27878=CARTESIAN_POINT('Origin',(8.69,0.4,16.31));
#27879=CARTESIAN_POINT('',(8.7,-0.7,16.31));
#27880=CARTESIAN_POINT('',(8.7,0.6,16.31));
#27881=CARTESIAN_POINT('',(8.75,-0.7,16.31));
#27882=CARTESIAN_POINT('',(8.75,0.4,16.31));
#27883=CARTESIAN_POINT('',(8.69,-0.7,16.31));
#27884=CARTESIAN_POINT('Origin',(8.69,-0.7,16.31));
#27885=CARTESIAN_POINT('',(8.7,-0.7,9.155));
#27886=CARTESIAN_POINT('',(8.75,-0.7,16.31));
#27887=CARTESIAN_POINT('Origin',(8.75,-0.15,16.3));
#27888=CARTESIAN_POINT('Origin',(8.69,-0.7,15.79));
#27889=CARTESIAN_POINT('',(8.7,-0.7,15.79));
#27890=CARTESIAN_POINT('',(8.7,-0.1,15.79));
#27891=CARTESIAN_POINT('',(8.7,0.05,15.79));
#27892=CARTESIAN_POINT('',(8.75,-0.7,15.79));
#27893=CARTESIAN_POINT('',(8.69,-0.7,15.79));
#27894=CARTESIAN_POINT('',(8.75,-0.1,15.79));
#27895=CARTESIAN_POINT('',(8.75,-0.7,15.79));
#27896=CARTESIAN_POINT('',(8.69,-0.1,15.79));
#27897=CARTESIAN_POINT('Origin',(8.69,-0.1,15.79));
#27898=CARTESIAN_POINT('',(8.7,-0.1,15.81));
#27899=CARTESIAN_POINT('',(8.7,-0.1,8.895));
#27900=CARTESIAN_POINT('',(8.75,-0.1,15.81));
#27901=CARTESIAN_POINT('',(8.75,-0.1,15.79));
#27902=CARTESIAN_POINT('',(8.69,-0.1,15.81));
#27903=CARTESIAN_POINT('Origin',(8.69,-0.1,15.81));
#27904=CARTESIAN_POINT('',(8.7,-0.7,15.81));
#27905=CARTESIAN_POINT('',(8.7,0.35,15.81));
#27906=CARTESIAN_POINT('',(8.75,-0.7,15.81));
#27907=CARTESIAN_POINT('',(8.75,-0.1,15.81));
#27908=CARTESIAN_POINT('',(8.69,-0.7,15.81));
#27909=CARTESIAN_POINT('Origin',(8.69,-0.7,15.81));
#27910=CARTESIAN_POINT('',(8.7,-0.7,8.905));
#27911=CARTESIAN_POINT('',(8.75,-0.7,15.81));
#27912=CARTESIAN_POINT('Origin',(8.75,-0.4,15.8));
#27913=CARTESIAN_POINT('Origin',(8.69,-0.7,15.29));
#27914=CARTESIAN_POINT('',(8.7,-0.7,15.29));
#27915=CARTESIAN_POINT('',(8.7,0.4,15.29));
#27916=CARTESIAN_POINT('',(8.7,0.05,15.29));
#27917=CARTESIAN_POINT('',(8.75,-0.7,15.29));
#27918=CARTESIAN_POINT('',(8.69,-0.7,15.29));
#27919=CARTESIAN_POINT('',(8.75,0.4,15.29));
#27920=CARTESIAN_POINT('',(8.75,-0.7,15.29));
#27921=CARTESIAN_POINT('',(8.69,0.4,15.29));
#27922=CARTESIAN_POINT('Origin',(8.69,0.4,15.29));
#27923=CARTESIAN_POINT('',(8.7,0.4,15.31));
#27924=CARTESIAN_POINT('',(8.7,0.4,8.645));
#27925=CARTESIAN_POINT('',(8.75,0.4,15.31));
#27926=CARTESIAN_POINT('',(8.75,0.4,15.29));
#27927=CARTESIAN_POINT('',(8.69,0.4,15.31));
#27928=CARTESIAN_POINT('Origin',(8.69,0.4,15.31));
#27929=CARTESIAN_POINT('',(8.7,-0.7,15.31));
#27930=CARTESIAN_POINT('',(8.7,0.6,15.31));
#27931=CARTESIAN_POINT('',(8.75,-0.7,15.31));
#27932=CARTESIAN_POINT('',(8.75,0.4,15.31));
#27933=CARTESIAN_POINT('',(8.69,-0.7,15.31));
#27934=CARTESIAN_POINT('Origin',(8.69,-0.7,15.31));
#27935=CARTESIAN_POINT('',(8.7,-0.7,8.655));
#27936=CARTESIAN_POINT('',(8.75,-0.7,15.31));
#27937=CARTESIAN_POINT('Origin',(8.75,-0.15,15.3));
#27938=CARTESIAN_POINT('Origin',(8.69,-0.7,14.79));
#27939=CARTESIAN_POINT('',(8.7,-0.7,14.79));
#27940=CARTESIAN_POINT('',(8.7,-0.1,14.79));
#27941=CARTESIAN_POINT('',(8.7,0.05,14.79));
#27942=CARTESIAN_POINT('',(8.75,-0.7,14.79));
#27943=CARTESIAN_POINT('',(8.69,-0.7,14.79));
#27944=CARTESIAN_POINT('',(8.75,-0.1,14.79));
#27945=CARTESIAN_POINT('',(8.75,-0.7,14.79));
#27946=CARTESIAN_POINT('',(8.69,-0.1,14.79));
#27947=CARTESIAN_POINT('Origin',(8.69,-0.1,14.79));
#27948=CARTESIAN_POINT('',(8.7,-0.1,14.81));
#27949=CARTESIAN_POINT('',(8.7,-0.1,8.395));
#27950=CARTESIAN_POINT('',(8.75,-0.1,14.81));
#27951=CARTESIAN_POINT('',(8.75,-0.1,14.79));
#27952=CARTESIAN_POINT('',(8.69,-0.1,14.81));
#27953=CARTESIAN_POINT('Origin',(8.69,-0.1,14.81));
#27954=CARTESIAN_POINT('',(8.7,-0.7,14.81));
#27955=CARTESIAN_POINT('',(8.7,0.35,14.81));
#27956=CARTESIAN_POINT('',(8.75,-0.7,14.81));
#27957=CARTESIAN_POINT('',(8.75,-0.1,14.81));
#27958=CARTESIAN_POINT('',(8.69,-0.7,14.81));
#27959=CARTESIAN_POINT('Origin',(8.69,-0.7,14.81));
#27960=CARTESIAN_POINT('',(8.7,-0.7,8.405));
#27961=CARTESIAN_POINT('',(8.75,-0.7,14.81));
#27962=CARTESIAN_POINT('Origin',(8.75,-0.4,14.8));
#27963=CARTESIAN_POINT('Origin',(8.69,-0.7,14.29));
#27964=CARTESIAN_POINT('',(8.7,-0.7,14.29));
#27965=CARTESIAN_POINT('',(8.7,0.4,14.29));
#27966=CARTESIAN_POINT('',(8.7,0.05,14.29));
#27967=CARTESIAN_POINT('',(8.75,-0.7,14.29));
#27968=CARTESIAN_POINT('',(8.69,-0.7,14.29));
#27969=CARTESIAN_POINT('',(8.75,0.4,14.29));
#27970=CARTESIAN_POINT('',(8.75,-0.7,14.29));
#27971=CARTESIAN_POINT('',(8.69,0.4,14.29));
#27972=CARTESIAN_POINT('Origin',(8.69,0.4,14.29));
#27973=CARTESIAN_POINT('',(8.7,0.4,14.31));
#27974=CARTESIAN_POINT('',(8.7,0.4,8.145));
#27975=CARTESIAN_POINT('',(8.75,0.4,14.31));
#27976=CARTESIAN_POINT('',(8.75,0.4,14.29));
#27977=CARTESIAN_POINT('',(8.69,0.4,14.31));
#27978=CARTESIAN_POINT('Origin',(8.69,0.4,14.31));
#27979=CARTESIAN_POINT('',(8.7,-0.7,14.31));
#27980=CARTESIAN_POINT('',(8.7,0.6,14.31));
#27981=CARTESIAN_POINT('',(8.75,-0.7,14.31));
#27982=CARTESIAN_POINT('',(8.75,0.4,14.31));
#27983=CARTESIAN_POINT('',(8.69,-0.7,14.31));
#27984=CARTESIAN_POINT('Origin',(8.69,-0.7,14.31));
#27985=CARTESIAN_POINT('',(8.7,-0.7,8.155));
#27986=CARTESIAN_POINT('',(8.75,-0.7,14.31));
#27987=CARTESIAN_POINT('Origin',(8.75,-0.15,14.3));
#27988=CARTESIAN_POINT('Origin',(8.69,-0.7,13.79));
#27989=CARTESIAN_POINT('',(8.7,-0.7,13.79));
#27990=CARTESIAN_POINT('',(8.7,-0.1,13.79));
#27991=CARTESIAN_POINT('',(8.7,0.05,13.79));
#27992=CARTESIAN_POINT('',(8.75,-0.7,13.79));
#27993=CARTESIAN_POINT('',(8.69,-0.7,13.79));
#27994=CARTESIAN_POINT('',(8.75,-0.1,13.79));
#27995=CARTESIAN_POINT('',(8.75,-0.7,13.79));
#27996=CARTESIAN_POINT('',(8.69,-0.1,13.79));
#27997=CARTESIAN_POINT('Origin',(8.69,-0.1,13.79));
#27998=CARTESIAN_POINT('',(8.7,-0.1,13.81));
#27999=CARTESIAN_POINT('',(8.7,-0.1,7.895));
#28000=CARTESIAN_POINT('',(8.75,-0.1,13.81));
#28001=CARTESIAN_POINT('',(8.75,-0.1,13.79));
#28002=CARTESIAN_POINT('',(8.69,-0.1,13.81));
#28003=CARTESIAN_POINT('Origin',(8.69,-0.1,13.81));
#28004=CARTESIAN_POINT('',(8.7,-0.7,13.81));
#28005=CARTESIAN_POINT('',(8.7,0.35,13.81));
#28006=CARTESIAN_POINT('',(8.75,-0.7,13.81));
#28007=CARTESIAN_POINT('',(8.75,-0.1,13.81));
#28008=CARTESIAN_POINT('',(8.69,-0.7,13.81));
#28009=CARTESIAN_POINT('Origin',(8.69,-0.7,13.81));
#28010=CARTESIAN_POINT('',(8.7,-0.7,7.905));
#28011=CARTESIAN_POINT('',(8.75,-0.7,13.81));
#28012=CARTESIAN_POINT('Origin',(8.75,-0.4,13.8));
#28013=CARTESIAN_POINT('Origin',(8.69,-0.7,13.29));
#28014=CARTESIAN_POINT('',(8.7,-0.7,13.29));
#28015=CARTESIAN_POINT('',(8.7,0.4,13.29));
#28016=CARTESIAN_POINT('',(8.7,0.05,13.29));
#28017=CARTESIAN_POINT('',(8.75,-0.7,13.29));
#28018=CARTESIAN_POINT('',(8.69,-0.7,13.29));
#28019=CARTESIAN_POINT('',(8.75,0.4,13.29));
#28020=CARTESIAN_POINT('',(8.75,-0.7,13.29));
#28021=CARTESIAN_POINT('',(8.69,0.4,13.29));
#28022=CARTESIAN_POINT('Origin',(8.69,0.4,13.29));
#28023=CARTESIAN_POINT('',(8.7,0.4,13.31));
#28024=CARTESIAN_POINT('',(8.7,0.4,7.645));
#28025=CARTESIAN_POINT('',(8.75,0.4,13.31));
#28026=CARTESIAN_POINT('',(8.75,0.4,13.29));
#28027=CARTESIAN_POINT('',(8.69,0.4,13.31));
#28028=CARTESIAN_POINT('Origin',(8.69,0.4,13.31));
#28029=CARTESIAN_POINT('',(8.7,-0.7,13.31));
#28030=CARTESIAN_POINT('',(8.7,0.6,13.31));
#28031=CARTESIAN_POINT('',(8.75,-0.7,13.31));
#28032=CARTESIAN_POINT('',(8.75,0.4,13.31));
#28033=CARTESIAN_POINT('',(8.69,-0.7,13.31));
#28034=CARTESIAN_POINT('Origin',(8.69,-0.7,13.31));
#28035=CARTESIAN_POINT('',(8.7,-0.7,7.655));
#28036=CARTESIAN_POINT('',(8.75,-0.7,13.31));
#28037=CARTESIAN_POINT('Origin',(8.75,-0.15,13.3));
#28038=CARTESIAN_POINT('Origin',(8.69,-0.7,12.79));
#28039=CARTESIAN_POINT('',(8.7,-0.7,12.79));
#28040=CARTESIAN_POINT('',(8.7,-0.1,12.79));
#28041=CARTESIAN_POINT('',(8.7,0.05,12.79));
#28042=CARTESIAN_POINT('',(8.75,-0.7,12.79));
#28043=CARTESIAN_POINT('',(8.69,-0.7,12.79));
#28044=CARTESIAN_POINT('',(8.75,-0.1,12.79));
#28045=CARTESIAN_POINT('',(8.75,-0.7,12.79));
#28046=CARTESIAN_POINT('',(8.69,-0.1,12.79));
#28047=CARTESIAN_POINT('Origin',(8.69,-0.1,12.79));
#28048=CARTESIAN_POINT('',(8.7,-0.1,12.81));
#28049=CARTESIAN_POINT('',(8.7,-0.1,7.395));
#28050=CARTESIAN_POINT('',(8.75,-0.1,12.81));
#28051=CARTESIAN_POINT('',(8.75,-0.1,12.79));
#28052=CARTESIAN_POINT('',(8.69,-0.1,12.81));
#28053=CARTESIAN_POINT('Origin',(8.69,-0.1,12.81));
#28054=CARTESIAN_POINT('',(8.7,-0.7,12.81));
#28055=CARTESIAN_POINT('',(8.7,0.35,12.81));
#28056=CARTESIAN_POINT('',(8.75,-0.7,12.81));
#28057=CARTESIAN_POINT('',(8.75,-0.1,12.81));
#28058=CARTESIAN_POINT('',(8.69,-0.7,12.81));
#28059=CARTESIAN_POINT('Origin',(8.69,-0.7,12.81));
#28060=CARTESIAN_POINT('',(8.7,-0.7,7.405));
#28061=CARTESIAN_POINT('',(8.75,-0.7,12.81));
#28062=CARTESIAN_POINT('Origin',(8.75,-0.4,12.8));
#28063=CARTESIAN_POINT('Origin',(8.69,-0.7,12.29));
#28064=CARTESIAN_POINT('',(8.7,-0.7,12.29));
#28065=CARTESIAN_POINT('',(8.7,0.4,12.29));
#28066=CARTESIAN_POINT('',(8.7,0.05,12.29));
#28067=CARTESIAN_POINT('',(8.75,-0.7,12.29));
#28068=CARTESIAN_POINT('',(8.69,-0.7,12.29));
#28069=CARTESIAN_POINT('',(8.75,0.4,12.29));
#28070=CARTESIAN_POINT('',(8.75,-0.7,12.29));
#28071=CARTESIAN_POINT('',(8.69,0.4,12.29));
#28072=CARTESIAN_POINT('Origin',(8.69,0.4,12.29));
#28073=CARTESIAN_POINT('',(8.7,0.4,12.31));
#28074=CARTESIAN_POINT('',(8.7,0.4,7.145));
#28075=CARTESIAN_POINT('',(8.75,0.4,12.31));
#28076=CARTESIAN_POINT('',(8.75,0.4,12.29));
#28077=CARTESIAN_POINT('',(8.69,0.4,12.31));
#28078=CARTESIAN_POINT('Origin',(8.69,0.4,12.31));
#28079=CARTESIAN_POINT('',(8.7,-0.7,12.31));
#28080=CARTESIAN_POINT('',(8.7,0.6,12.31));
#28081=CARTESIAN_POINT('',(8.75,-0.7,12.31));
#28082=CARTESIAN_POINT('',(8.75,0.4,12.31));
#28083=CARTESIAN_POINT('',(8.69,-0.7,12.31));
#28084=CARTESIAN_POINT('Origin',(8.69,-0.7,12.31));
#28085=CARTESIAN_POINT('',(8.7,-0.7,7.155));
#28086=CARTESIAN_POINT('',(8.75,-0.7,12.31));
#28087=CARTESIAN_POINT('Origin',(8.75,-0.15,12.3));
#28088=CARTESIAN_POINT('Origin',(8.69,-0.7,11.79));
#28089=CARTESIAN_POINT('',(8.7,-0.7,11.79));
#28090=CARTESIAN_POINT('',(8.7,-0.1,11.79));
#28091=CARTESIAN_POINT('',(8.7,0.05,11.79));
#28092=CARTESIAN_POINT('',(8.75,-0.7,11.79));
#28093=CARTESIAN_POINT('',(8.69,-0.7,11.79));
#28094=CARTESIAN_POINT('',(8.75,-0.1,11.79));
#28095=CARTESIAN_POINT('',(8.75,-0.7,11.79));
#28096=CARTESIAN_POINT('',(8.69,-0.1,11.79));
#28097=CARTESIAN_POINT('Origin',(8.69,-0.1,11.79));
#28098=CARTESIAN_POINT('',(8.7,-0.1,11.81));
#28099=CARTESIAN_POINT('',(8.7,-0.1,6.895));
#28100=CARTESIAN_POINT('',(8.75,-0.1,11.81));
#28101=CARTESIAN_POINT('',(8.75,-0.1,11.79));
#28102=CARTESIAN_POINT('',(8.69,-0.1,11.81));
#28103=CARTESIAN_POINT('Origin',(8.69,-0.1,11.81));
#28104=CARTESIAN_POINT('',(8.7,-0.7,11.81));
#28105=CARTESIAN_POINT('',(8.7,0.35,11.81));
#28106=CARTESIAN_POINT('',(8.75,-0.7,11.81));
#28107=CARTESIAN_POINT('',(8.75,-0.1,11.81));
#28108=CARTESIAN_POINT('',(8.69,-0.7,11.81));
#28109=CARTESIAN_POINT('Origin',(8.69,-0.7,11.81));
#28110=CARTESIAN_POINT('',(8.7,-0.7,6.905));
#28111=CARTESIAN_POINT('',(8.75,-0.7,11.81));
#28112=CARTESIAN_POINT('Origin',(8.75,-0.4,11.8));
#28113=CARTESIAN_POINT('Origin',(8.69,-0.7,11.29));
#28114=CARTESIAN_POINT('',(8.7,-0.7,11.29));
#28115=CARTESIAN_POINT('',(8.7,0.4,11.29));
#28116=CARTESIAN_POINT('',(8.7,0.05,11.29));
#28117=CARTESIAN_POINT('',(8.75,-0.7,11.29));
#28118=CARTESIAN_POINT('',(8.69,-0.7,11.29));
#28119=CARTESIAN_POINT('',(8.75,0.4,11.29));
#28120=CARTESIAN_POINT('',(8.75,-0.7,11.29));
#28121=CARTESIAN_POINT('',(8.69,0.4,11.29));
#28122=CARTESIAN_POINT('Origin',(8.69,0.4,11.29));
#28123=CARTESIAN_POINT('',(8.7,0.4,11.31));
#28124=CARTESIAN_POINT('',(8.7,0.4,6.645));
#28125=CARTESIAN_POINT('',(8.75,0.4,11.31));
#28126=CARTESIAN_POINT('',(8.75,0.4,11.29));
#28127=CARTESIAN_POINT('',(8.69,0.4,11.31));
#28128=CARTESIAN_POINT('Origin',(8.69,0.4,11.31));
#28129=CARTESIAN_POINT('',(8.7,-0.7,11.31));
#28130=CARTESIAN_POINT('',(8.7,0.6,11.31));
#28131=CARTESIAN_POINT('',(8.75,-0.7,11.31));
#28132=CARTESIAN_POINT('',(8.75,0.4,11.31));
#28133=CARTESIAN_POINT('',(8.69,-0.7,11.31));
#28134=CARTESIAN_POINT('Origin',(8.69,-0.7,11.31));
#28135=CARTESIAN_POINT('',(8.7,-0.7,6.655));
#28136=CARTESIAN_POINT('',(8.75,-0.7,11.31));
#28137=CARTESIAN_POINT('Origin',(8.75,-0.15,11.3));
#28138=CARTESIAN_POINT('Origin',(8.69,-0.7,10.79));
#28139=CARTESIAN_POINT('',(8.7,-0.7,10.79));
#28140=CARTESIAN_POINT('',(8.7,-0.1,10.79));
#28141=CARTESIAN_POINT('',(8.7,0.05,10.79));
#28142=CARTESIAN_POINT('',(8.75,-0.7,10.79));
#28143=CARTESIAN_POINT('',(8.69,-0.7,10.79));
#28144=CARTESIAN_POINT('',(8.75,-0.1,10.79));
#28145=CARTESIAN_POINT('',(8.75,-0.7,10.79));
#28146=CARTESIAN_POINT('',(8.69,-0.1,10.79));
#28147=CARTESIAN_POINT('Origin',(8.69,-0.1,10.79));
#28148=CARTESIAN_POINT('',(8.7,-0.1,10.81));
#28149=CARTESIAN_POINT('',(8.7,-0.1,6.395));
#28150=CARTESIAN_POINT('',(8.75,-0.1,10.81));
#28151=CARTESIAN_POINT('',(8.75,-0.1,10.79));
#28152=CARTESIAN_POINT('',(8.69,-0.1,10.81));
#28153=CARTESIAN_POINT('Origin',(8.69,-0.1,10.81));
#28154=CARTESIAN_POINT('',(8.7,-0.7,10.81));
#28155=CARTESIAN_POINT('',(8.7,0.35,10.81));
#28156=CARTESIAN_POINT('',(8.75,-0.7,10.81));
#28157=CARTESIAN_POINT('',(8.75,-0.1,10.81));
#28158=CARTESIAN_POINT('',(8.69,-0.7,10.81));
#28159=CARTESIAN_POINT('Origin',(8.69,-0.7,10.81));
#28160=CARTESIAN_POINT('',(8.7,-0.7,6.405));
#28161=CARTESIAN_POINT('',(8.75,-0.7,10.81));
#28162=CARTESIAN_POINT('Origin',(8.75,-0.4,10.8));
#28163=CARTESIAN_POINT('Origin',(8.69,-0.7,10.29));
#28164=CARTESIAN_POINT('',(8.7,-0.7,10.29));
#28165=CARTESIAN_POINT('',(8.7,0.4,10.29));
#28166=CARTESIAN_POINT('',(8.7,0.05,10.29));
#28167=CARTESIAN_POINT('',(8.75,-0.7,10.29));
#28168=CARTESIAN_POINT('',(8.69,-0.7,10.29));
#28169=CARTESIAN_POINT('',(8.75,0.4,10.29));
#28170=CARTESIAN_POINT('',(8.75,-0.7,10.29));
#28171=CARTESIAN_POINT('',(8.69,0.4,10.29));
#28172=CARTESIAN_POINT('Origin',(8.69,0.4,10.29));
#28173=CARTESIAN_POINT('',(8.7,0.4,10.31));
#28174=CARTESIAN_POINT('',(8.7,0.4,6.145));
#28175=CARTESIAN_POINT('',(8.75,0.4,10.31));
#28176=CARTESIAN_POINT('',(8.75,0.4,10.29));
#28177=CARTESIAN_POINT('',(8.69,0.4,10.31));
#28178=CARTESIAN_POINT('Origin',(8.69,0.4,10.31));
#28179=CARTESIAN_POINT('',(8.7,-0.7,10.31));
#28180=CARTESIAN_POINT('',(8.7,0.6,10.31));
#28181=CARTESIAN_POINT('',(8.75,-0.7,10.31));
#28182=CARTESIAN_POINT('',(8.75,0.4,10.31));
#28183=CARTESIAN_POINT('',(8.69,-0.7,10.31));
#28184=CARTESIAN_POINT('Origin',(8.69,-0.7,10.31));
#28185=CARTESIAN_POINT('',(8.7,-0.7,6.155));
#28186=CARTESIAN_POINT('',(8.75,-0.7,10.31));
#28187=CARTESIAN_POINT('Origin',(8.75,-0.15,10.3));
#28188=CARTESIAN_POINT('Origin',(8.69,-0.7,9.79));
#28189=CARTESIAN_POINT('',(8.7,-0.7,9.79));
#28190=CARTESIAN_POINT('',(8.7,-0.1,9.79));
#28191=CARTESIAN_POINT('',(8.7,0.05,9.79));
#28192=CARTESIAN_POINT('',(8.75,-0.7,9.79));
#28193=CARTESIAN_POINT('',(8.69,-0.7,9.79));
#28194=CARTESIAN_POINT('',(8.75,-0.1,9.79));
#28195=CARTESIAN_POINT('',(8.75,-0.7,9.79));
#28196=CARTESIAN_POINT('',(8.69,-0.1,9.79));
#28197=CARTESIAN_POINT('Origin',(8.69,-0.1,9.79));
#28198=CARTESIAN_POINT('',(8.7,-0.1,9.81));
#28199=CARTESIAN_POINT('',(8.7,-0.1,5.895));
#28200=CARTESIAN_POINT('',(8.75,-0.1,9.81));
#28201=CARTESIAN_POINT('',(8.75,-0.1,9.79));
#28202=CARTESIAN_POINT('',(8.69,-0.1,9.81));
#28203=CARTESIAN_POINT('Origin',(8.69,-0.1,9.81));
#28204=CARTESIAN_POINT('',(8.7,-0.7,9.81));
#28205=CARTESIAN_POINT('',(8.7,0.35,9.81));
#28206=CARTESIAN_POINT('',(8.75,-0.7,9.81));
#28207=CARTESIAN_POINT('',(8.75,-0.1,9.81));
#28208=CARTESIAN_POINT('',(8.69,-0.7,9.81));
#28209=CARTESIAN_POINT('Origin',(8.69,-0.7,9.81));
#28210=CARTESIAN_POINT('',(8.7,-0.7,5.905));
#28211=CARTESIAN_POINT('',(8.75,-0.7,9.81));
#28212=CARTESIAN_POINT('Origin',(8.75,-0.4,9.8));
#28213=CARTESIAN_POINT('Origin',(8.69,-0.7,9.29));
#28214=CARTESIAN_POINT('',(8.7,-0.7,9.29));
#28215=CARTESIAN_POINT('',(8.7,0.4,9.29));
#28216=CARTESIAN_POINT('',(8.7,0.05,9.29));
#28217=CARTESIAN_POINT('',(8.75,-0.7,9.29));
#28218=CARTESIAN_POINT('',(8.69,-0.7,9.29));
#28219=CARTESIAN_POINT('',(8.75,0.4,9.29));
#28220=CARTESIAN_POINT('',(8.75,-0.7,9.29));
#28221=CARTESIAN_POINT('',(8.69,0.4,9.29));
#28222=CARTESIAN_POINT('Origin',(8.69,0.4,9.29));
#28223=CARTESIAN_POINT('',(8.7,0.4,9.31));
#28224=CARTESIAN_POINT('',(8.7,0.4,5.645));
#28225=CARTESIAN_POINT('',(8.75,0.4,9.31));
#28226=CARTESIAN_POINT('',(8.75,0.4,9.29));
#28227=CARTESIAN_POINT('',(8.69,0.4,9.31));
#28228=CARTESIAN_POINT('Origin',(8.69,0.4,9.31));
#28229=CARTESIAN_POINT('',(8.7,-0.7,9.31));
#28230=CARTESIAN_POINT('',(8.7,0.6,9.31));
#28231=CARTESIAN_POINT('',(8.75,-0.7,9.31));
#28232=CARTESIAN_POINT('',(8.75,0.4,9.31));
#28233=CARTESIAN_POINT('',(8.69,-0.7,9.31));
#28234=CARTESIAN_POINT('Origin',(8.69,-0.7,9.31));
#28235=CARTESIAN_POINT('',(8.7,-0.7,5.655));
#28236=CARTESIAN_POINT('',(8.75,-0.7,9.31));
#28237=CARTESIAN_POINT('Origin',(8.75,-0.15,9.3));
#28238=CARTESIAN_POINT('Origin',(8.6,0.,28.));
#28239=CARTESIAN_POINT('',(8.7,-3.3677786976552E-17,28.275));
#28240=CARTESIAN_POINT('Origin',(8.7,0.,28.));
#28241=CARTESIAN_POINT('',(9.,3.3677786976552E-17,28.275));
#28242=CARTESIAN_POINT('',(8.6,-3.3677786976552E-17,28.275));
#28243=CARTESIAN_POINT('Origin',(9.,0.,28.));
#28244=CARTESIAN_POINT('Origin',(8.6,0.,3.));
#28245=CARTESIAN_POINT('',(8.7,-3.36777869765522E-17,3.275));
#28246=CARTESIAN_POINT('Origin',(8.7,0.,3.));
#28247=CARTESIAN_POINT('',(9.,3.36777869765522E-17,3.275));
#28248=CARTESIAN_POINT('',(8.6,-3.36777869765522E-17,3.275));
#28249=CARTESIAN_POINT('Origin',(9.,0.,3.));
#28250=CARTESIAN_POINT('Origin',(9.,0.8,2.));
#28251=CARTESIAN_POINT('',(9.,0.8,2.));
#28252=CARTESIAN_POINT('',(8.7,0.8,2.));
#28253=CARTESIAN_POINT('',(9.,0.8,2.));
#28254=CARTESIAN_POINT('',(8.7,0.8,30.));
#28255=CARTESIAN_POINT('',(8.7,0.8,2.));
#28256=CARTESIAN_POINT('',(9.,0.8,30.));
#28257=CARTESIAN_POINT('',(9.,0.8,30.));
#28258=CARTESIAN_POINT('',(9.,0.8,2.));
#28259=CARTESIAN_POINT('Origin',(9.,-0.8,2.));
#28260=CARTESIAN_POINT('',(9.,-0.8,2.));
#28261=CARTESIAN_POINT('',(9.,-0.8,2.));
#28262=CARTESIAN_POINT('',(9.,-0.8,30.));
#28263=CARTESIAN_POINT('',(9.,-0.8,30.));
#28264=CARTESIAN_POINT('',(9.,-0.8,2.));
#28265=CARTESIAN_POINT('Origin',(8.7,-0.8,2.));
#28266=CARTESIAN_POINT('',(8.7,-0.8,2.));
#28267=CARTESIAN_POINT('',(8.7,-0.8,2.));
#28268=CARTESIAN_POINT('',(8.7,-0.8,30.));
#28269=CARTESIAN_POINT('',(8.7,-0.8,30.));
#28270=CARTESIAN_POINT('',(8.7,-0.8,2.));
#28271=CARTESIAN_POINT('Origin',(8.7,0.8,2.));
#28272=CARTESIAN_POINT('',(8.7,0.8,2.));
#28273=CARTESIAN_POINT('',(8.7,0.8,30.));
#28274=CARTESIAN_POINT('Origin',(8.85,0.,30.));
#28275=CARTESIAN_POINT('Origin',(8.85,0.,2.));
#28276=CARTESIAN_POINT('',(0.,0.,0.));
#28277=CARTESIAN_POINT('Origin',(0.05,0.,0.));
#28278=CARTESIAN_POINT('',(0.1,7.34788079488412E-17,0.6));
#28279=CARTESIAN_POINT('Origin',(0.1,0.,0.));
#28280=CARTESIAN_POINT('',(0.,-6.12323399573677E-17,0.5));
#28281=CARTESIAN_POINT('',(0.05,-6.73555739531044E-17,0.55));
#28282=CARTESIAN_POINT('Origin',(0.,0.,0.));
#28283=CARTESIAN_POINT('Origin',(0.,0.,0.));
#28284=CARTESIAN_POINT('',(29.9,-7.34788079488412E-17,0.6));
#28285=CARTESIAN_POINT('Origin',(29.9,0.,0.));
#28286=CARTESIAN_POINT('',(0.,-7.34788079488412E-17,0.6));
#28287=CARTESIAN_POINT('Origin',(0.,0.,0.));
#28288=CARTESIAN_POINT('Origin',(29.95,0.,0.));
#28289=CARTESIAN_POINT('',(30.,6.12323399573677E-17,0.5));
#28290=CARTESIAN_POINT('Origin',(30.,0.,0.));
#28291=CARTESIAN_POINT('',(29.95,-6.73555739531044E-17,0.55));
#28292=CARTESIAN_POINT('Origin',(30.,0.,0.));
#28293=CARTESIAN_POINT('',(0.,0.,0.));
#28294=CARTESIAN_POINT('Origin',(-1.6,0.,1.3));
#28295=CARTESIAN_POINT('',(-1.2,0.340036762718386,1.3));
#28296=CARTESIAN_POINT('',(-1.2,-0.340036762718386,1.3));
#28297=CARTESIAN_POINT('',(-1.2,0.,1.3));
#28298=CARTESIAN_POINT('Origin',(-1.6,0.,1.3));
#28299=CARTESIAN_POINT('Origin',(-1.6,0.,0.6));
#28300=CARTESIAN_POINT('',(-1.2,0.340036762718386,0.6));
#28301=CARTESIAN_POINT('',(-1.2,0.340036762718386,0.6));
#28302=CARTESIAN_POINT('',(-1.2,-0.340036762718386,0.6));
#28303=CARTESIAN_POINT('Origin',(-1.6,0.,0.6));
#28304=CARTESIAN_POINT('',(-1.2,-0.340036762718386,0.6));
#28305=CARTESIAN_POINT('Origin',(1.6,0.,0.6));
#28306=CARTESIAN_POINT('',(1.2,0.340036762718386,1.3));
#28307=CARTESIAN_POINT('',(1.2,0.340036762718386,0.6));
#28308=CARTESIAN_POINT('',(1.2,0.340036762718386,0.6));
#28309=CARTESIAN_POINT('',(1.2,-0.340036762718386,1.3));
#28310=CARTESIAN_POINT('Origin',(1.6,0.,1.3));
#28311=CARTESIAN_POINT('',(1.2,-0.340036762718386,0.6));
#28312=CARTESIAN_POINT('',(1.2,-0.340036762718386,0.6));
#28313=CARTESIAN_POINT('Origin',(1.6,0.,0.6));
#28314=CARTESIAN_POINT('Origin',(1.6,0.,1.3));
#28315=CARTESIAN_POINT('',(1.2,0.,1.3));
#28316=CARTESIAN_POINT('Origin',(-2.1,0.,0.6));
#28317=CARTESIAN_POINT('',(-1.2,0.7,0.6));
#28318=CARTESIAN_POINT('',(-1.2,0.,0.6));
#28319=CARTESIAN_POINT('',(-2.1,0.7,0.6));
#28320=CARTESIAN_POINT('',(-1.2,0.7,0.6));
#28321=CARTESIAN_POINT('',(-2.1,-0.7,0.6));
#28322=CARTESIAN_POINT('',(-2.1,0.,0.6));
#28323=CARTESIAN_POINT('',(-1.2,-0.7,0.6));
#28324=CARTESIAN_POINT('',(-1.2,-0.7,0.6));
#28325=CARTESIAN_POINT('',(-1.2,0.,0.6));
#28326=CARTESIAN_POINT('',(-1.875,3.36777869765522E-17,0.6));
#28327=CARTESIAN_POINT('Origin',(-1.6,0.,0.6));
#28328=CARTESIAN_POINT('Origin',(-1.2,0.,0.6));
#28329=CARTESIAN_POINT('',(-1.2,-0.7,3.75));
#28330=CARTESIAN_POINT('',(-1.2,-0.7,3.75));
#28331=CARTESIAN_POINT('',(-1.2,0.7,3.75));
#28332=CARTESIAN_POINT('',(-1.2,0.,3.75));
#28333=CARTESIAN_POINT('',(-1.2,0.7,3.75));
#28334=CARTESIAN_POINT('',(-1.2,-2.02066721859313E-17,3.515));
#28335=CARTESIAN_POINT('Origin',(-1.2,0.,3.35));
#28336=CARTESIAN_POINT('Origin',(1.2,0.,0.6));
#28337=CARTESIAN_POINT('',(2.1,-0.7,0.6));
#28338=CARTESIAN_POINT('',(2.1,0.7,0.6));
#28339=CARTESIAN_POINT('',(2.1,0.,0.6));
#28340=CARTESIAN_POINT('',(1.2,0.7,0.6));
#28341=CARTESIAN_POINT('',(2.1,0.7,0.6));
#28342=CARTESIAN_POINT('',(1.2,0.,0.6));
#28343=CARTESIAN_POINT('',(1.2,-0.7,0.6));
#28344=CARTESIAN_POINT('',(1.2,0.,0.6));
#28345=CARTESIAN_POINT('',(2.1,-0.7,0.6));
#28346=CARTESIAN_POINT('',(1.325,3.36777869765522E-17,0.6));
#28347=CARTESIAN_POINT('Origin',(1.6,0.,0.6));
#28348=CARTESIAN_POINT('Origin',(0.1,0.,3.35));
#28349=CARTESIAN_POINT('',(0.1,-2.75545529808155E-17,3.575));
#28350=CARTESIAN_POINT('Origin',(0.1,0.,3.35));
#28351=CARTESIAN_POINT('',(1.2,2.75545529808155E-17,3.575));
#28352=CARTESIAN_POINT('',(0.1,-2.75545529808155E-17,3.575));
#28353=CARTESIAN_POINT('Origin',(1.2,0.,3.35));
#28354=CARTESIAN_POINT('Origin',(0.,0.,3.35));
#28355=CARTESIAN_POINT('',(-0.1,2.02066721859313E-17,3.515));
#28356=CARTESIAN_POINT('',(0.,-2.02066721859313E-17,3.515));
#28357=CARTESIAN_POINT('Origin',(-0.1,0.,3.35));
#28358=CARTESIAN_POINT('Origin',(-1.6,0.,-0.05));
#28359=CARTESIAN_POINT('',(-1.875,-3.36777869765522E-17,0.));
#28360=CARTESIAN_POINT('Origin',(-1.6,0.,0.));
#28361=CARTESIAN_POINT('',(-1.875,-3.36777869765522E-17,-0.05));
#28362=CARTESIAN_POINT('Origin',(1.6,0.,-0.05));
#28363=CARTESIAN_POINT('',(1.325,-3.36777869765522E-17,0.));
#28364=CARTESIAN_POINT('Origin',(1.6,0.,0.));
#28365=CARTESIAN_POINT('',(1.325,-3.36777869765522E-17,-0.05));
#28366=CARTESIAN_POINT('Origin',(0.,0.,2.3));
#28367=CARTESIAN_POINT('',(-0.6,-0.7,2.3));
#28368=CARTESIAN_POINT('Origin',(0.,-0.7,2.3));
#28369=CARTESIAN_POINT('',(-0.6,0.7,2.3));
#28370=CARTESIAN_POINT('',(-0.6,0.,2.3));
#28371=CARTESIAN_POINT('Origin',(0.,0.7,2.3));
#28372=CARTESIAN_POINT('Origin',(0.,-0.7,1.875));
#28373=CARTESIAN_POINT('',(-2.1,-0.7,0.));
#28374=CARTESIAN_POINT('',(-2.1,-0.7,0.6));
#28375=CARTESIAN_POINT('',(2.1,-0.7,0.));
#28376=CARTESIAN_POINT('',(-2.1,-0.7,0.));
#28377=CARTESIAN_POINT('',(2.1,-0.7,0.));
#28378=CARTESIAN_POINT('',(1.2,-0.7,3.75));
#28379=CARTESIAN_POINT('',(1.2,-0.7,0.6));
#28380=CARTESIAN_POINT('',(0.1,-0.7,3.75));
#28381=CARTESIAN_POINT('',(1.2,-0.7,3.75));
#28382=CARTESIAN_POINT('',(0.1,-0.7,2.95));
#28383=CARTESIAN_POINT('',(0.1,-0.7,3.75));
#28384=CARTESIAN_POINT('',(-0.1,-0.7,2.95));
#28385=CARTESIAN_POINT('',(0.1,-0.7,2.95));
#28386=CARTESIAN_POINT('',(-0.1,-0.7,3.75));
#28387=CARTESIAN_POINT('',(-0.1,-0.7,2.95));
#28388=CARTESIAN_POINT('',(-0.1,-0.7,3.75));
#28389=CARTESIAN_POINT('Origin',(-2.1,0.,0.));
#28390=CARTESIAN_POINT('',(-2.1,0.7,0.));
#28391=CARTESIAN_POINT('',(-2.1,0.7,0.6));
#28392=CARTESIAN_POINT('',(-2.1,0.,0.));
#28393=CARTESIAN_POINT('Origin',(2.1,0.,0.));
#28394=CARTESIAN_POINT('',(2.1,0.7,0.));
#28395=CARTESIAN_POINT('',(-2.1,0.7,0.));
#28396=CARTESIAN_POINT('',(2.1,0.,0.));
#28397=CARTESIAN_POINT('Origin',(2.1,0.,0.6));
#28398=CARTESIAN_POINT('',(2.1,0.7,0.));
#28399=CARTESIAN_POINT('Origin',(1.2,0.,3.75));
#28400=CARTESIAN_POINT('',(1.2,0.7,3.75));
#28401=CARTESIAN_POINT('',(1.2,0.7,0.6));
#28402=CARTESIAN_POINT('',(1.2,0.,3.75));
#28403=CARTESIAN_POINT('Origin',(0.1,0.,3.75));
#28404=CARTESIAN_POINT('',(0.1,0.7,3.75));
#28405=CARTESIAN_POINT('',(1.2,0.7,3.75));
#28406=CARTESIAN_POINT('',(0.1,0.,3.75));
#28407=CARTESIAN_POINT('Origin',(0.1,0.,2.95));
#28408=CARTESIAN_POINT('',(0.1,0.7,2.95));
#28409=CARTESIAN_POINT('',(0.1,0.7,3.75));
#28410=CARTESIAN_POINT('',(0.1,0.,2.95));
#28411=CARTESIAN_POINT('Origin',(-0.1,0.,2.95));
#28412=CARTESIAN_POINT('',(-0.1,0.7,2.95));
#28413=CARTESIAN_POINT('',(0.1,0.7,2.95));
#28414=CARTESIAN_POINT('',(-0.1,0.,2.95));
#28415=CARTESIAN_POINT('Origin',(-0.1,0.,3.75));
#28416=CARTESIAN_POINT('',(-0.1,0.7,3.75));
#28417=CARTESIAN_POINT('',(-0.1,0.7,2.95));
#28418=CARTESIAN_POINT('',(-0.1,0.,3.75));
#28419=CARTESIAN_POINT('Origin',(-1.2,0.,3.75));
#28420=CARTESIAN_POINT('',(-0.1,0.7,3.75));
#28421=CARTESIAN_POINT('Origin',(0.,0.7,1.875));
#28422=CARTESIAN_POINT('',(0.,0.,0.));
#28423=CARTESIAN_POINT('Origin',(0.115470053837925,-0.5,-0.2));
#28424=CARTESIAN_POINT('',(0.23094010767585,-0.5,0.));
#28425=CARTESIAN_POINT('',(0.115470053837925,-0.5,-0.2));
#28426=CARTESIAN_POINT('',(0.23094010767585,-0.5,0.));
#28427=CARTESIAN_POINT('',(0.115470053837925,-0.8,-0.2));
#28428=CARTESIAN_POINT('',(0.115470053837925,-0.5,-0.2));
#28429=CARTESIAN_POINT('',(0.23094010767585,-0.8,0.));
#28430=CARTESIAN_POINT('',(0.23094010767585,-0.8,0.));
#28431=CARTESIAN_POINT('',(0.23094010767585,-0.5,0.));
#28432=CARTESIAN_POINT('Origin',(-0.115470053837925,-0.5,-0.2));
#28433=CARTESIAN_POINT('',(-0.115470053837925,-0.5,-0.2));
#28434=CARTESIAN_POINT('',(0.115470053837925,-0.5,-0.2));
#28435=CARTESIAN_POINT('',(-0.115470053837925,-0.8,-0.2));
#28436=CARTESIAN_POINT('',(-0.115470053837925,-0.5,-0.2));
#28437=CARTESIAN_POINT('',(0.115470053837925,-0.8,-0.2));
#28438=CARTESIAN_POINT('Origin',(-0.23094010767585,-0.5,-2.77555756156289E-17));
#28439=CARTESIAN_POINT('',(-0.23094010767585,-0.5,-2.82820063659975E-17));
#28440=CARTESIAN_POINT('',(-0.115470053837925,-0.5,-0.2));
#28441=CARTESIAN_POINT('',(-0.23094010767585,-0.8,-2.77555756156289E-17));
#28442=CARTESIAN_POINT('',(-0.23094010767585,-0.5,-2.82820063659975E-17));
#28443=CARTESIAN_POINT('',(-0.115470053837925,-0.8,-0.2));
#28444=CARTESIAN_POINT('Origin',(-0.115470053837925,-0.5,0.2));
#28445=CARTESIAN_POINT('',(-0.115470053837925,-0.5,0.2));
#28446=CARTESIAN_POINT('',(-0.23094010767585,-0.5,-2.82820063659975E-17));
#28447=CARTESIAN_POINT('',(-0.115470053837925,-0.8,0.2));
#28448=CARTESIAN_POINT('',(-0.115470053837925,-0.5,0.2));
#28449=CARTESIAN_POINT('',(-0.23094010767585,-0.8,-2.82820063659975E-17));
#28450=CARTESIAN_POINT('Origin',(0.115470053837925,-0.5,0.2));
#28451=CARTESIAN_POINT('',(0.115470053837925,-0.5,0.2));
#28452=CARTESIAN_POINT('',(-0.115470053837925,-0.5,0.2));
#28453=CARTESIAN_POINT('',(0.115470053837925,-0.8,0.2));
#28454=CARTESIAN_POINT('',(0.115470053837925,-0.5,0.2));
#28455=CARTESIAN_POINT('',(-0.115470053837925,-0.8,0.2));
#28456=CARTESIAN_POINT('Origin',(0.23094010767585,-0.5,0.));
#28457=CARTESIAN_POINT('',(0.115470053837925,-0.5,0.2));
#28458=CARTESIAN_POINT('',(0.115470053837925,-0.8,0.2));
#28459=CARTESIAN_POINT('Origin',(0.,-0.5,0.));
#28460=CARTESIAN_POINT('Origin',(0.,-0.8,0.));
#28461=CARTESIAN_POINT('Origin',(0.,-1.4,0.));
#28462=CARTESIAN_POINT('',(-0.24505,-1.4,3.00099698131059E-17));
#28463=CARTESIAN_POINT('Origin',(0.,-1.4,0.));
#28464=CARTESIAN_POINT('Origin',(0.375,0.5,0.));
#28465=CARTESIAN_POINT('',(-0.375,0.5,-4.59242549680257E-17));
#28466=CARTESIAN_POINT('Origin',(0.,0.5,0.));
#28467=CARTESIAN_POINT('Origin',(0.,0.475,0.));
#28468=CARTESIAN_POINT('',(-0.425,0.45,-5.20474889637625E-17));
#28469=CARTESIAN_POINT('Origin',(0.,0.45,0.));
#28470=CARTESIAN_POINT('',(-0.4,0.475,-4.89858719658941E-17));
#28471=CARTESIAN_POINT('Origin',(0.,0.24,0.));
#28472=CARTESIAN_POINT('',(-0.425,0.0299999999999998,-5.20474889637625E-17));
#28473=CARTESIAN_POINT('Origin',(0.,0.0299999999999998,0.));
#28474=CARTESIAN_POINT('',(-0.425,0.24,-5.20474889637625E-17));
#28475=CARTESIAN_POINT('Origin',(0.,0.0150000000000001,0.));
#28476=CARTESIAN_POINT('',(-0.395,4.85722573273506E-17,-4.83735485663204E-17));
#28477=CARTESIAN_POINT('Origin',(0.,0.,0.));
#28478=CARTESIAN_POINT('',(-0.41,0.0150000000000001,-5.02105187650415E-17));
#28479=CARTESIAN_POINT('Origin',(0.27,0.,0.));
#28480=CARTESIAN_POINT('',(-0.27,0.,-3.30654635769785E-17));
#28481=CARTESIAN_POINT('Origin',(0.,0.,0.));
#28482=CARTESIAN_POINT('Origin',(0.,-0.02,0.));
#28483=CARTESIAN_POINT('',(-0.24505,-0.0498999999999999,3.00099698131059E-17));
#28484=CARTESIAN_POINT('Origin',(0.,-0.0498999999999999,0.));
#28485=CARTESIAN_POINT('',(-0.26,-0.02,-3.18408167778312E-17));
#28486=CARTESIAN_POINT('Origin',(0.,-0.995,0.));
#28487=CARTESIAN_POINT('',(-0.24505,-0.995,-3.00099698131059E-17));
#28488=CARTESIAN_POINT('',(0.,0.,0.));
#28489=CARTESIAN_POINT('',(0.,0.,0.));
#28490=CARTESIAN_POINT('Origin',(0.,0.,0.));
#28491=CARTESIAN_POINT('',(-1.070235,-0.308121667383195,-1.31065986708547E-16));
#28492=CARTESIAN_POINT('',(-1.31065986708547E-16,-0.308121667383195,1.070235));
#28493=CARTESIAN_POINT('Origin',(0.,-0.308121667383195,0.));
#28494=CARTESIAN_POINT('Origin',(0.,-0.308121667383195,0.));
#28495=CARTESIAN_POINT('',(-1.31065986708547E-16,0.308121667383195,1.070235));
#28496=CARTESIAN_POINT('Origin',(-1.34711147906209E-16,0.,1.1));
#28497=CARTESIAN_POINT('',(-1.070235,0.308121667383195,1.31065986708547E-16));
#28498=CARTESIAN_POINT('Origin',(0.,0.308121667383195,0.));
#28499=CARTESIAN_POINT('Origin',(0.,0.308121667383195,0.));
#28500=CARTESIAN_POINT('Origin',(0.,0.,0.));
#28501=CARTESIAN_POINT('',(-1.070235,0.5,-1.31065986708547E-16));
#28502=CARTESIAN_POINT('',(-1.070235,0.,-1.31065986708547E-16));
#28503=CARTESIAN_POINT('Origin',(0.,0.5,0.));
#28504=CARTESIAN_POINT('Origin',(0.,0.,0.));
#28505=CARTESIAN_POINT('',(-0.6,-0.44,-7.34788079488412E-17));
#28506=CARTESIAN_POINT('Origin',(0.,-0.44,0.));
#28507=CARTESIAN_POINT('',(-0.6,0.44,-7.34788079488412E-17));
#28508=CARTESIAN_POINT('',(-0.6,0.,-7.34788079488412E-17));
#28509=CARTESIAN_POINT('Origin',(0.,0.44,0.));
#28510=CARTESIAN_POINT('Origin',(0.,0.47,0.));
#28511=CARTESIAN_POINT('',(-0.66,0.5,-8.08266887437253E-17));
#28512=CARTESIAN_POINT('',(-0.63,0.47,-7.71527483462832E-17));
#28513=CARTESIAN_POINT('Origin',(0.,0.5,0.));
#28514=CARTESIAN_POINT('Origin',(1.070235,0.5,0.));
#28515=CARTESIAN_POINT('Origin',(0.,0.,0.));
#28516=CARTESIAN_POINT('',(-1.070235,-0.5,-1.31065986708547E-16));
#28517=CARTESIAN_POINT('Origin',(0.,-0.5,0.));
#28518=CARTESIAN_POINT('',(-1.070235,0.,-1.31065986708547E-16));
#28519=CARTESIAN_POINT('Origin',(0.66,-0.5,0.));
#28520=CARTESIAN_POINT('',(-0.66,-0.5,-8.08266887437253E-17));
#28521=CARTESIAN_POINT('Origin',(0.,-0.5,0.));
#28522=CARTESIAN_POINT('Origin',(0.,-0.47,0.));
#28523=CARTESIAN_POINT('',(-0.63,-0.47,-7.71527483462832E-17));
#28524=CARTESIAN_POINT('',(0.,0.,0.));
#28525=CARTESIAN_POINT('Origin',(0.,0.,0.));
#28526=CARTESIAN_POINT('',(-1.129765,0.308121667383195,-1.38356309103871E-16));
#28527=CARTESIAN_POINT('',(-1.38356309103871E-16,0.308121667383195,1.129765));
#28528=CARTESIAN_POINT('Origin',(0.,0.308121667383195,0.));
#28529=CARTESIAN_POINT('Origin',(0.,0.308121667383195,0.));
#28530=CARTESIAN_POINT('',(-1.38356309103871E-16,-0.308121667383195,1.129765));
#28531=CARTESIAN_POINT('Origin',(-1.34711147906209E-16,0.,1.1));
#28532=CARTESIAN_POINT('',(-1.129765,-0.308121667383195,1.38356309103871E-16));
#28533=CARTESIAN_POINT('Origin',(0.,-0.308121667383195,0.));
#28534=CARTESIAN_POINT('Origin',(0.,-0.308121667383195,0.));
#28535=CARTESIAN_POINT('Origin',(0.,0.,0.));
#28536=CARTESIAN_POINT('',(-1.129765,-0.5,-1.38356309103871E-16));
#28537=CARTESIAN_POINT('Origin',(0.,-0.5,0.));
#28538=CARTESIAN_POINT('',(-1.129765,0.,-1.38356309103871E-16));
#28539=CARTESIAN_POINT('Origin',(1.54,0.5,0.));
#28540=CARTESIAN_POINT('',(-1.54,0.5,-1.88595607068692E-16));
#28541=CARTESIAN_POINT('Origin',(0.,0.5,0.));
#28542=CARTESIAN_POINT('',(-1.129765,0.5,-1.38356309103871E-16));
#28543=CARTESIAN_POINT('Origin',(0.,0.5,0.));
#28544=CARTESIAN_POINT('Origin',(0.,0.47,0.));
#28545=CARTESIAN_POINT('',(-1.6,0.44,-1.95943487863577E-16));
#28546=CARTESIAN_POINT('Origin',(0.,0.44,0.));
#28547=CARTESIAN_POINT('',(-1.57,0.47,-1.92269547466134E-16));
#28548=CARTESIAN_POINT('Origin',(0.,0.,0.));
#28549=CARTESIAN_POINT('',(-1.6,-0.44,-1.95943487863577E-16));
#28550=CARTESIAN_POINT('Origin',(0.,-0.44,0.));
#28551=CARTESIAN_POINT('',(-1.6,0.,-1.95943487863577E-16));
#28552=CARTESIAN_POINT('Origin',(0.,-0.47,0.));
#28553=CARTESIAN_POINT('',(-1.54,-0.5,-1.88595607068692E-16));
#28554=CARTESIAN_POINT('Origin',(0.,-0.5,0.));
#28555=CARTESIAN_POINT('',(-1.57,-0.47,-1.92269547466134E-16));
#28556=CARTESIAN_POINT('Origin',(1.129765,-0.5,0.));
#28557=CARTESIAN_POINT('Origin',(0.,0.,0.));
#28558=CARTESIAN_POINT('',(-1.129765,0.,-1.38356309103871E-16));
#28559=CARTESIAN_POINT('',(0.,0.,0.));
#28560=CARTESIAN_POINT('Origin',(1.1,0.,0.));
#28561=CARTESIAN_POINT('',(1.1,-2.23201749654651E-33,0.29765));
#28562=CARTESIAN_POINT('',(1.1,-2.23201749654651E-33,-0.29765));
#28563=CARTESIAN_POINT('Origin',(1.1,0.,0.));
#28564=CARTESIAN_POINT('Origin',(0.685838782044607,0.,-0.860014630714833));
#28565=CARTESIAN_POINT('',(0.918550922801216,-5.31350540756609E-33,-0.674432891191581));
#28566=CARTESIAN_POINT('',(0.453126641287998,8.49470414473068E-34,-1.04559637023808));
#28567=CARTESIAN_POINT('Origin',(0.685838782044607,0.,-0.860014630714833));
#28568=CARTESIAN_POINT('Origin',(-0.244773027351946,0.,-1.07242070340001));
#28569=CARTESIAN_POINT('',(0.0454142657089739,-2.23201749654651E-33,-1.1386540593921));
#28570=CARTESIAN_POINT('',(-0.534960320412865,-2.23201749654651E-33,-1.00618734740791));
#28571=CARTESIAN_POINT('Origin',(-0.244773027351946,0.,-1.07242070340001));
#28572=CARTESIAN_POINT('Origin',(-0.991065754692661,0.,-0.477272113029314));
#28573=CARTESIAN_POINT('',(-0.86192025974432,8.49470414473067E-34,-0.745445496560469));
#28574=CARTESIAN_POINT('',(-1.120211249641,-5.31350540756609E-33,-0.209098729498159));
#28575=CARTESIAN_POINT('Origin',(-0.991065754692661,0.,-0.477272113029314));
#28576=CARTESIAN_POINT('Origin',(-0.991065754692661,0.,0.477272113029314));
#28577=CARTESIAN_POINT('',(-1.120211249641,-2.23201749654651E-33,0.209098729498159));
#28578=CARTESIAN_POINT('',(-0.86192025974432,-2.23201749654651E-33,0.745445496560469));
#28579=CARTESIAN_POINT('Origin',(-0.991065754692661,0.,0.477272113029314));
#28580=CARTESIAN_POINT('Origin',(-0.244773027351946,0.,1.07242070340001));
#28581=CARTESIAN_POINT('',(-0.534960320412866,-2.23201749654651E-33,1.00618734740791));
#28582=CARTESIAN_POINT('',(0.0454142657089737,-2.23201749654651E-33,1.1386540593921));
#28583=CARTESIAN_POINT('Origin',(-0.244773027351946,0.,1.07242070340001));
#28584=CARTESIAN_POINT('Origin',(0.685838782044607,0.,0.860014630714833));
#28585=CARTESIAN_POINT('',(0.453126641287998,-2.23201749654651E-33,1.04559637023808));
#28586=CARTESIAN_POINT('',(0.918550922801216,-2.23201749654651E-33,0.674432891191581));
#28587=CARTESIAN_POINT('Origin',(0.685838782044607,0.,0.860014630714833));
#28588=CARTESIAN_POINT('',(0.,0.,0.));
#28589=CARTESIAN_POINT('Origin',(0.685838782044607,0.,0.860014630714833));
#28590=CARTESIAN_POINT('',(0.413083465285518,-0.05953,0.993751811093549));
#28591=CARTESIAN_POINT('',(0.876916659919095,-0.05953,0.623857181492959));
#28592=CARTESIAN_POINT('Ctrl Pts',(0.413083465285518,-0.05953,0.993751811093549));
#28593=CARTESIAN_POINT('Ctrl Pts',(0.419070565453383,-0.0925528133349865,
0.991263089003441));
#28594=CARTESIAN_POINT('Ctrl Pts',(0.430199341854858,-0.124911173756694,
0.986608710139579));
#28595=CARTESIAN_POINT('Ctrl Pts',(0.457978755888596,-0.177924977804098,
0.973971221090534));
#28596=CARTESIAN_POINT('Ctrl Pts',(0.473077587363685,-0.199697230012983,
0.966820759530997));
#28597=CARTESIAN_POINT('Ctrl Pts',(0.507057380724533,-0.237895043532788,
0.949440676105255));
#28598=CARTESIAN_POINT('Ctrl Pts',(0.525933334162555,-0.254319232363049,
0.939198248544428));
#28599=CARTESIAN_POINT('Ctrl Pts',(0.564362943424238,-0.28018331644634,
0.916597376014514));
#28600=CARTESIAN_POINT('Ctrl Pts',(0.585840553788742,-0.29104845371857,
0.903141581680914));
#28601=CARTESIAN_POINT('Ctrl Pts',(0.629305439856167,-0.30527573347708,
0.873412008702649));
#28602=CARTESIAN_POINT('Ctrl Pts',(0.651278921914856,-0.308638795020976,
0.857118508332695));
#28603=CARTESIAN_POINT('Ctrl Pts',(0.690705563850638,-0.308638795020976,
0.825676810575914));
#28604=CARTESIAN_POINT('Ctrl Pts',(0.711480111898423,-0.30527573347708,
0.807879894508811));
#28605=CARTESIAN_POINT('Ctrl Pts',(0.750136149454208,-0.29104845371857,
0.772120216227122));
#28606=CARTESIAN_POINT('Ctrl Pts',(0.768033796848072,-0.28018331644634,
0.754175290318038));
#28607=CARTESIAN_POINT('Ctrl Pts',(0.798619410861634,-0.254319232363049,
0.721738358858166));
#28608=CARTESIAN_POINT('Ctrl Pts',(0.812805334167529,-0.237895043532788,
0.705614819529209));
#28609=CARTESIAN_POINT('Ctrl Pts',(0.837310877969633,-0.199697230012983,
0.676354402927683));
#28610=CARTESIAN_POINT('Ctrl Pts',(0.847641868610495,-0.177924977804098,
0.663225258065736));
#28611=CARTESIAN_POINT('Ctrl Pts',(0.866144010579847,-0.124911173756694,
0.638954437806245));
#28612=CARTESIAN_POINT('Ctrl Pts',(0.873158080166742,-0.0925528133349865,
0.62914037979579));
#28613=CARTESIAN_POINT('Ctrl Pts',(0.876916659919095,-0.05953,0.623857181492959));
#28614=CARTESIAN_POINT('',(0.437601487681057,-0.05953,1.03511272300331));
#28615=CARTESIAN_POINT('Origin',(0.685838782044607,-0.05953,0.860014630714833));
#28616=CARTESIAN_POINT('',(0.911784794170997,-0.05953,0.656964154625313));
#28617=CARTESIAN_POINT('Ctrl Pts',(0.911784794170998,-0.0595300000000001,
0.656964154625312));
#28618=CARTESIAN_POINT('Ctrl Pts',(0.909827729890942,-0.0762225747374255,
0.659680317203144));
#28619=CARTESIAN_POINT('Ctrl Pts',(0.907004864562642,-0.0928409665394228,
0.663576540841106));
#28620=CARTESIAN_POINT('Ctrl Pts',(0.895234408667242,-0.144299303100741,
0.679480524217551));
#28621=CARTESIAN_POINT('Ctrl Pts',(0.882797231409153,-0.177024326825049,
0.695831250979106));
#28622=CARTESIAN_POINT('Ctrl Pts',(0.854332839576145,-0.227269801620064,
0.73042219438957));
#28623=CARTESIAN_POINT('Ctrl Pts',(0.834863020612702,-0.251265615809407,
0.752807465209441));
#28624=CARTESIAN_POINT('Ctrl Pts',(0.800439809856111,-0.279889827963178,
0.789147407129766));
#28625=CARTESIAN_POINT('Ctrl Pts',(0.781998747691871,-0.290879136862659,
0.80756613568454));
#28626=CARTESIAN_POINT('Ctrl Pts',(0.742239891936898,-0.305251990234487,
0.844254137480382));
#28627=CARTESIAN_POINT('Ctrl Pts',(0.720906778729541,-0.308638795020976,
0.862505527716294));
#28628=CARTESIAN_POINT('Ctrl Pts',(0.680463863683392,-0.308638795020976,
0.894757676234429));
#28629=CARTESIAN_POINT('Ctrl Pts',(0.657923009631182,-0.305251990234488,
0.91149460735272));
#28630=CARTESIAN_POINT('Ctrl Pts',(0.613307674922609,-0.290879136862659,
0.942092777160053));
#28631=CARTESIAN_POINT('Ctrl Pts',(0.591247219971725,-0.279889827963178,
0.955972930713954));
#28632=CARTESIAN_POINT('Ctrl Pts',(0.548158511259202,-0.251265615809407,
0.981446681891443));
#28633=CARTESIAN_POINT('Ctrl Pts',(0.522002043615455,-0.227269801620063,
0.995447160474328));
#28634=CARTESIAN_POINT('Ctrl Pts',(0.481944444320713,-0.177024326825049,
1.01550068154148));
#28635=CARTESIAN_POINT('Ctrl Pts',(0.463236132117164,-0.14429930310074,
1.0239876538093));
#28636=CARTESIAN_POINT('Ctrl Pts',(0.445111721969657,-0.0928409665394226,
1.03192403056628));
#28637=CARTESIAN_POINT('Ctrl Pts',(0.440685038163619,-0.0762225747374254,
1.03380912944435));
#28638=CARTESIAN_POINT('Ctrl Pts',(0.437601487681056,-0.05953,1.03511272300331));
#28639=CARTESIAN_POINT('Origin',(0.685838782044607,-0.05953,0.860014630714833));
#28640=CARTESIAN_POINT('Origin',(0.,-0.208355,0.));
#28641=CARTESIAN_POINT('',(0.0548532617164168,-0.05953,1.12247250791415));
#28642=CARTESIAN_POINT('Origin',(0.,-0.05953,0.));
#28643=CARTESIAN_POINT('',(-0.536443649899848,-0.05953,0.987512846410683));
#28644=CARTESIAN_POINT('Ctrl Pts',(0.0548532617164173,-0.0595300000000001,
1.12247250791414));
#28645=CARTESIAN_POINT('Ctrl Pts',(0.05150947068137,-0.0762225747374254,
1.12263591311425));
#28646=CARTESIAN_POINT('Ctrl Pts',(0.0467032526342597,-0.0928409665394227,
1.12285816383385));
#28647=CARTESIAN_POINT('Ctrl Pts',(0.0269302585198975,-0.144299303100741,
1.12357162229597));
#28648=CARTESIAN_POINT('Ctrl Pts',(0.006392292392153,-0.177024326825049,
1.12404235695137));
#28649=CARTESIAN_POINT('Ctrl Pts',(-0.0383992541984087,-0.227269801620063,
1.12335509974011));
#28650=CARTESIAN_POINT('Ctrl Pts',(-0.0680399972366993,-0.251265615809407,
1.12208997038458));
#28651=CARTESIAN_POINT('Ctrl Pts',(-0.117914228755037,-0.279889827963178,
1.1178344036749));
#28652=CARTESIAN_POINT('Ctrl Pts',(-0.14381238480104,-0.290879136862659,
1.11490049012186));
#28653=CARTESIAN_POINT('Ctrl Pts',(-0.19728546073067,-0.305251990234488,
1.10669035995599));
#28654=CARTESIAN_POINT('Ctrl Pts',(-0.224855950742601,-0.308638795020976,
1.10139101611326));
#28655=CARTESIAN_POINT('Ctrl Pts',(-0.275287440920027,-0.308638795020976,
1.0898803575765));
#28656=CARTESIAN_POINT('Ctrl Pts',(-0.302426893214945,-0.305251990234488,
1.08269251410343));
#28657=CARTESIAN_POINT('Ctrl Pts',(-0.35416671187353,-0.290879136862659,
1.06688848765783));
#28658=CARTESIAN_POINT('Ctrl Pts',(-0.3787731215897,-0.279889827963178,
1.05829506364875));
#28659=CARTESIAN_POINT('Ctrl Pts',(-0.425554672694338,-0.251265615809407,
1.04048957871266));
#28660=CARTESIAN_POINT('Ctrl Pts',(-0.452808978448581,-0.227269801620063,
1.02876878445619));
#28661=CARTESIAN_POINT('Ctrl Pts',(-0.493462957200432,-0.177024326825049,
1.0099536580922));
#28662=CARTESIAN_POINT('Ctrl Pts',(-0.511762781179148,-0.14429930310074,
1.00061845128527));
#28663=CARTESIAN_POINT('Ctrl Pts',(-0.529268075276157,-0.0928409665394226,
0.991396466802468));
#28664=CARTESIAN_POINT('Ctrl Pts',(-0.533501897135713,-0.0762225747374254,
0.989110885965947));
#28665=CARTESIAN_POINT('Ctrl Pts',(-0.536443649899848,-0.0595300000000001,
0.987512846410683));
#28666=CARTESIAN_POINT('',(-0.843383895613249,-0.05953,0.742736168477219));
#28667=CARTESIAN_POINT('Origin',(0.,-0.05953,0.));
#28668=CARTESIAN_POINT('',(-1.10653577764992,-0.05953,0.196295654879792));
#28669=CARTESIAN_POINT('Ctrl Pts',(-0.843383895613249,-0.0595300000000001,
0.742736168477219));
#28670=CARTESIAN_POINT('Ctrl Pts',(-0.84559647055299,-0.0762225747374255,
0.740223768851062));
#28671=CARTESIAN_POINT('Ctrl Pts',(-0.848766861100456,-0.0928409665394227,
0.736604687327351));
#28672=CARTESIAN_POINT('Ctrl Pts',(-0.861652925570091,-0.144299303100741,
0.721590372101268));
#28673=CARTESIAN_POINT('Ctrl Pts',(-0.87482617317514,-0.177024326825049,
0.705826641853758));
#28674=CARTESIAN_POINT('Ctrl Pts',(-0.902215926359523,-0.227269801620063,
0.670378702718353));
#28675=CARTESIAN_POINT('Ctrl Pts',(-0.919707509403859,-0.251265615809407,
0.646415841396062));
#28676=CARTESIAN_POINT('Ctrl Pts',(-0.947476448101718,-0.279889827963178,
0.604769294586516));
#28677=CARTESIAN_POINT('Ctrl Pts',(-0.961329858300736,-0.290879136862659,
0.582692035672022));
#28678=CARTESIAN_POINT('Ctrl Pts',(-0.988250837578047,-0.305251990234488,
0.535766169015486));
#28679=CARTESIAN_POINT('Ctrl Pts',(-1.00129756308006,-0.308638795020976,
0.510906605094603));
#28680=CARTESIAN_POINT('Ctrl Pts',(-1.02374168767024,-0.308638795020976,
0.46430090015576));
#28681=CARTESIAN_POINT('Ctrl Pts',(-1.03504317708586,-0.305251990234488,
0.438600874831839));
#28682=CARTESIAN_POINT('Ctrl Pts',(-1.05494634094458,-0.290879136862659,
0.388295406390235));
#28683=CARTESIAN_POINT('Ctrl Pts',(-1.06356957703048,-0.279889827963178,
0.363699428370917));
#28684=CARTESIAN_POINT('Ctrl Pts',(-1.0788165083757,-0.251265615809407,
0.316022600643821));
#28685=CARTESIAN_POINT('Ctrl Pts',(-1.08664560412098,-0.227269801620063,
0.287406530683752));
#28686=CARTESIAN_POINT('Ctrl Pts',(-1.09728268713976,-0.177024326825049,
0.243890930799337));
#28687=CARTESIAN_POINT('Ctrl Pts',(-1.10139388218929,-0.144299303100741,
0.22376314604679));
#28688=CARTESIAN_POINT('Ctrl Pts',(-1.10509821673782,-0.0928409665394227,
0.204327142733961));
#28689=CARTESIAN_POINT('Ctrl Pts',(-1.10595102243643,-0.0762225747374254,
0.199591971170104));
#28690=CARTESIAN_POINT('Ctrl Pts',(-1.10653577764992,-0.0595300000000001,
0.196295654879792));
#28691=CARTESIAN_POINT('',(-1.123812,-0.05953,1.37627276864339E-16));
#28692=CARTESIAN_POINT('Origin',(0.,-0.05953,0.));
#28693=CARTESIAN_POINT('',(-1.123812,-0.35718,1.37627276864339E-16));
#28694=CARTESIAN_POINT('',(-1.123812,-0.208355,1.37627276864339E-16));
#28695=CARTESIAN_POINT('Origin',(0.,-0.35718,0.));
#28696=CARTESIAN_POINT('',(-1.10653577764992,-0.05953,-0.196295654879793));
#28697=CARTESIAN_POINT('Origin',(0.,-0.05953,0.));
#28698=CARTESIAN_POINT('',(-0.843383895613249,-0.05953,-0.742736168477219));
#28699=CARTESIAN_POINT('Ctrl Pts',(-1.10653577764992,-0.0595300000000001,
-0.196295654879792));
#28700=CARTESIAN_POINT('Ctrl Pts',(-1.10595102243643,-0.0762225747374255,
-0.199591971170104));
#28701=CARTESIAN_POINT('Ctrl Pts',(-1.10509821673782,-0.0928409665394228,
-0.204327142733962));
#28702=CARTESIAN_POINT('Ctrl Pts',(-1.10139388218929,-0.144299303100741,
-0.22376314604679));
#28703=CARTESIAN_POINT('Ctrl Pts',(-1.09728268713976,-0.177024326825049,
-0.243890930799338));
#28704=CARTESIAN_POINT('Ctrl Pts',(-1.08664560412098,-0.227269801620063,
-0.287406530683753));
#28705=CARTESIAN_POINT('Ctrl Pts',(-1.0788165083757,-0.251265615809407,
-0.316022600643821));
#28706=CARTESIAN_POINT('Ctrl Pts',(-1.06356957703048,-0.279889827963178,
-0.363699428370918));
#28707=CARTESIAN_POINT('Ctrl Pts',(-1.05494634094458,-0.290879136862659,
-0.388295406390235));
#28708=CARTESIAN_POINT('Ctrl Pts',(-1.03504317708586,-0.305251990234488,
-0.438600874831839));
#28709=CARTESIAN_POINT('Ctrl Pts',(-1.02374168767024,-0.308638795020976,
-0.46430090015576));
#28710=CARTESIAN_POINT('Ctrl Pts',(-1.00129756308006,-0.308638795020976,
-0.510906605094603));
#28711=CARTESIAN_POINT('Ctrl Pts',(-0.988250837578047,-0.305251990234488,
-0.535766169015486));
#28712=CARTESIAN_POINT('Ctrl Pts',(-0.961329858300736,-0.290879136862659,
-0.582692035672022));
#28713=CARTESIAN_POINT('Ctrl Pts',(-0.947476448101718,-0.279889827963178,
-0.604769294586516));
#28714=CARTESIAN_POINT('Ctrl Pts',(-0.919707509403859,-0.251265615809407,
-0.646415841396062));
#28715=CARTESIAN_POINT('Ctrl Pts',(-0.902215926359523,-0.227269801620064,
-0.670378702718353));
#28716=CARTESIAN_POINT('Ctrl Pts',(-0.87482617317514,-0.177024326825049,
-0.705826641853758));
#28717=CARTESIAN_POINT('Ctrl Pts',(-0.861652925570091,-0.144299303100741,
-0.721590372101268));
#28718=CARTESIAN_POINT('Ctrl Pts',(-0.848766861100456,-0.0928409665394229,
-0.736604687327351));
#28719=CARTESIAN_POINT('Ctrl Pts',(-0.84559647055299,-0.0762225747374255,
-0.740223768851063));
#28720=CARTESIAN_POINT('Ctrl Pts',(-0.843383895613249,-0.0595300000000001,
-0.742736168477219));
#28721=CARTESIAN_POINT('',(-0.536443649899847,-0.05953,-0.987512846410683));
#28722=CARTESIAN_POINT('Origin',(0.,-0.05953,0.));
#28723=CARTESIAN_POINT('',(0.0548532617164172,-0.05953,-1.12247250791415));
#28724=CARTESIAN_POINT('Ctrl Pts',(-0.536443649899848,-0.0595300000000001,
-0.987512846410683));
#28725=CARTESIAN_POINT('Ctrl Pts',(-0.533501897135712,-0.0762225747374254,
-0.989110885965947));
#28726=CARTESIAN_POINT('Ctrl Pts',(-0.529268075276156,-0.0928409665394227,
-0.991396466802469));
#28727=CARTESIAN_POINT('Ctrl Pts',(-0.511762781179147,-0.144299303100741,
-1.00061845128527));
#28728=CARTESIAN_POINT('Ctrl Pts',(-0.493462957200432,-0.177024326825049,
-1.0099536580922));
#28729=CARTESIAN_POINT('Ctrl Pts',(-0.45280897844858,-0.227269801620063,
-1.02876878445619));
#28730=CARTESIAN_POINT('Ctrl Pts',(-0.425554672694337,-0.251265615809407,
-1.04048957871266));
#28731=CARTESIAN_POINT('Ctrl Pts',(-0.3787731215897,-0.279889827963178,
-1.05829506364875));
#28732=CARTESIAN_POINT('Ctrl Pts',(-0.354166711873529,-0.290879136862659,
-1.06688848765783));
#28733=CARTESIAN_POINT('Ctrl Pts',(-0.302426893214944,-0.305251990234488,
-1.08269251410343));
#28734=CARTESIAN_POINT('Ctrl Pts',(-0.275287440920027,-0.308638795020976,
-1.0898803575765));
#28735=CARTESIAN_POINT('Ctrl Pts',(-0.224855950742601,-0.308638795020976,
-1.10139101611326));
#28736=CARTESIAN_POINT('Ctrl Pts',(-0.19728546073067,-0.305251990234488,
-1.10669035995599));
#28737=CARTESIAN_POINT('Ctrl Pts',(-0.143812384801039,-0.290879136862659,
-1.11490049012186));
#28738=CARTESIAN_POINT('Ctrl Pts',(-0.117914228755037,-0.279889827963178,
-1.1178344036749));
#28739=CARTESIAN_POINT('Ctrl Pts',(-0.0680399972366989,-0.251265615809407,
-1.12208997038458));
#28740=CARTESIAN_POINT('Ctrl Pts',(-0.0383992541984084,-0.227269801620063,
-1.12335509974011));
#28741=CARTESIAN_POINT('Ctrl Pts',(0.00639229239215326,-0.177024326825049,
-1.12404235695137));
#28742=CARTESIAN_POINT('Ctrl Pts',(0.0269302585198977,-0.144299303100741,
-1.12357162229597));
#28743=CARTESIAN_POINT('Ctrl Pts',(0.04670325263426,-0.0928409665394228,
-1.12285816383385));
#28744=CARTESIAN_POINT('Ctrl Pts',(0.0515094706813703,-0.0762225747374255,
-1.12263591311425));
#28745=CARTESIAN_POINT('Ctrl Pts',(0.0548532617164176,-0.0595300000000001,
-1.12247250791414));
#28746=CARTESIAN_POINT('',(0.437601487681057,-0.05953,-1.03511272300331));
#28747=CARTESIAN_POINT('Origin',(0.,-0.05953,0.));
#28748=CARTESIAN_POINT('',(0.911784794170997,-0.05953,-0.656964154625313));
#28749=CARTESIAN_POINT('Ctrl Pts',(0.437601487681056,-0.0595300000000001,
-1.03511272300331));
#28750=CARTESIAN_POINT('Ctrl Pts',(0.440685038163619,-0.0762225747374255,
-1.03380912944435));
#28751=CARTESIAN_POINT('Ctrl Pts',(0.445111721969657,-0.0928409665394228,
-1.03192403056628));
#28752=CARTESIAN_POINT('Ctrl Pts',(0.463236132117164,-0.144299303100741,
-1.0239876538093));
#28753=CARTESIAN_POINT('Ctrl Pts',(0.481944444320713,-0.177024326825049,
-1.01550068154148));
#28754=CARTESIAN_POINT('Ctrl Pts',(0.522002043615455,-0.227269801620064,
-0.995447160474328));
#28755=CARTESIAN_POINT('Ctrl Pts',(0.548158511259203,-0.251265615809407,
-0.981446681891443));
#28756=CARTESIAN_POINT('Ctrl Pts',(0.591247219971725,-0.279889827963178,
-0.955972930713954));
#28757=CARTESIAN_POINT('Ctrl Pts',(0.613307674922609,-0.290879136862659,
-0.942092777160053));
#28758=CARTESIAN_POINT('Ctrl Pts',(0.657923009631182,-0.305251990234487,
-0.91149460735272));
#28759=CARTESIAN_POINT('Ctrl Pts',(0.680463863683393,-0.308638795020976,
-0.894757676234429));
#28760=CARTESIAN_POINT('Ctrl Pts',(0.720906778729542,-0.308638795020976,
-0.862505527716294));
#28761=CARTESIAN_POINT('Ctrl Pts',(0.742239891936899,-0.305251990234488,
-0.844254137480381));
#28762=CARTESIAN_POINT('Ctrl Pts',(0.781998747691872,-0.290879136862659,
-0.80756613568454));
#28763=CARTESIAN_POINT('Ctrl Pts',(0.800439809856112,-0.279889827963178,
-0.789147407129765));
#28764=CARTESIAN_POINT('Ctrl Pts',(0.834863020612702,-0.251265615809407,
-0.752807465209441));
#28765=CARTESIAN_POINT('Ctrl Pts',(0.854332839576145,-0.227269801620064,
-0.73042219438957));
#28766=CARTESIAN_POINT('Ctrl Pts',(0.882797231409153,-0.177024326825049,
-0.695831250979106));
#28767=CARTESIAN_POINT('Ctrl Pts',(0.895234408667242,-0.144299303100741,
-0.679480524217551));
#28768=CARTESIAN_POINT('Ctrl Pts',(0.907004864562642,-0.0928409665394228,
-0.663576540841106));
#28769=CARTESIAN_POINT('Ctrl Pts',(0.909827729890942,-0.0762225747374256,
-0.659680317203144));
#28770=CARTESIAN_POINT('Ctrl Pts',(0.911784794170998,-0.0595300000000001,
-0.656964154625312));
#28771=CARTESIAN_POINT('',(1.08212377959455,-0.05953,-0.303251606722892));
#28772=CARTESIAN_POINT('Origin',(0.,-0.05953,0.));
#28773=CARTESIAN_POINT('',(1.08212377959455,-0.05953,0.303251606722892));
#28774=CARTESIAN_POINT('Ctrl Pts',(1.08212377959455,-0.0595300000000001,
-0.303251606722892));
#28775=CARTESIAN_POINT('Ctrl Pts',(1.0830271513892,-0.0762225747374255,
-0.300028012588062));
#28776=CARTESIAN_POINT('Ctrl Pts',(1.08431331394788,-0.0928409665394228,
-0.2953917518996));
#28777=CARTESIAN_POINT('Ctrl Pts',(1.08940878963422,-0.144299303100741,
-0.276273267473431));
#28778=CARTESIAN_POINT('Ctrl Pts',(1.09443784939331,-0.177024326825049,
-0.256354979351213));
#28779=CARTESIAN_POINT('Ctrl Pts',(1.10373487993589,-0.227269801620064,
-0.212533521233765));
#28780=CARTESIAN_POINT('Ctrl Pts',(1.10909715583869,-0.251265615809407,
-0.183354415742157));
#28781=CARTESIAN_POINT('Ctrl Pts',(1.1160463456491,-0.279889827963178,-0.133783682657561));
#28782=CARTESIAN_POINT('Ctrl Pts',(1.11894887330541,-0.290879136862659,
-0.107881990270302));
#28783=CARTESIAN_POINT('Ctrl Pts',(1.12284346704144,-0.305251990234488,
-0.0539226701638766));
#28784=CARTESIAN_POINT('Ctrl Pts',(1.123812,-0.308638795020976,-0.025864214957475));
#28785=CARTESIAN_POINT('Ctrl Pts',(1.123812,-0.308638795020976,0.025864214957475));
#28786=CARTESIAN_POINT('Ctrl Pts',(1.12284346704144,-0.305251990234488,
0.0539226701638766));
#28787=CARTESIAN_POINT('Ctrl Pts',(1.11894887330541,-0.290879136862659,
0.107881990270302));
#28788=CARTESIAN_POINT('Ctrl Pts',(1.1160463456491,-0.279889827963178,0.133783682657561));
#28789=CARTESIAN_POINT('Ctrl Pts',(1.10909715583869,-0.251265615809407,
0.183354415742157));
#28790=CARTESIAN_POINT('Ctrl Pts',(1.10373487993589,-0.227269801620064,
0.212533521233765));
#28791=CARTESIAN_POINT('Ctrl Pts',(1.09443784939331,-0.177024326825049,
0.256354979351213));
#28792=CARTESIAN_POINT('Ctrl Pts',(1.08940878963422,-0.144299303100741,
0.276273267473431));
#28793=CARTESIAN_POINT('Ctrl Pts',(1.08431331394788,-0.0928409665394228,
0.2953917518996));
#28794=CARTESIAN_POINT('Ctrl Pts',(1.0830271513892,-0.0762225747374255,
0.300028012588062));
#28795=CARTESIAN_POINT('Ctrl Pts',(1.08212377959455,-0.0595300000000001,
0.303251606722892));
#28796=CARTESIAN_POINT('Origin',(0.,-0.05953,0.));
#28797=CARTESIAN_POINT('Origin',(0.,-0.05953,0.));
#28798=CARTESIAN_POINT('',(0.0589974094846122,-0.05953,1.07456964270265));
#28799=CARTESIAN_POINT('Origin',(0.,-0.05953,0.));
#28800=CARTESIAN_POINT('Origin',(-0.244773027351946,-0.05953,1.07242070340001));
#28801=CARTESIAN_POINT('Origin',(-0.244773027351946,0.,1.07242070340001));
#28802=CARTESIAN_POINT('',(-0.519393123750572,-0.05953,0.942555777842682));
#28803=CARTESIAN_POINT('Ctrl Pts',(-0.519393123750572,-0.05953,0.942555777842682));
#28804=CARTESIAN_POINT('Ctrl Pts',(-0.513714466572041,-0.0925528133349865,
0.945684988399766));
#28805=CARTESIAN_POINT('Ctrl Pts',(-0.503136848051455,-0.124911173756694,
0.951483858396181));
#28806=CARTESIAN_POINT('Ctrl Pts',(-0.47593627990192,-0.177924977804098,
0.965323333309091));
#28807=CARTESIAN_POINT('Ctrl Pts',(-0.460931856495794,-0.199697230012983,
0.972669835243841));
#28808=CARTESIAN_POINT('Ctrl Pts',(-0.426157505475872,-0.237895043532788,
0.988400002689705));
#28809=CARTESIAN_POINT('Ctrl Pts',(-0.406380688682952,-0.254319232363049,
0.996771768218699));
#28810=CARTESIAN_POINT('Ctrl Pts',(-0.364750145543744,-0.28018331644634,
1.01272583306292));
#28811=CARTESIAN_POINT('Ctrl Pts',(-0.340838910881557,-0.29104845371857,
1.02112815447116));
#28812=CARTESIAN_POINT('Ctrl Pts',(-0.290495481564827,-0.30527573347708,
1.036574285215));
#28813=CARTESIAN_POINT('Ctrl Pts',(-0.264056468041074,-0.308638795020976,
1.04359501395068));
#28814=CARTESIAN_POINT('Ctrl Pts',(-0.214892249704082,-0.308638795020976,
1.05481642595959));
#28815=CARTESIAN_POINT('Ctrl Pts',(-0.188025341585962,-0.30527573347708,
1.05996242598502));
#28816=CARTESIAN_POINT('Ctrl Pts',(-0.135965654106109,-0.29104845371857,
1.06788913840721));
#28817=CARTESIAN_POINT('Ctrl Pts',(-0.110776745452494,-0.28018331644634,
1.07069360430242));
#28818=CARTESIAN_POINT('Ctrl Pts',(-0.0663467128214646,-0.254319232363049,
1.07438230428002));
#28819=CARTESIAN_POINT('Ctrl Pts',(-0.0448960436540983,-0.237895043532788,
1.07542044338697));
#28820=CARTESIAN_POINT('Ctrl Pts',(-0.00674037211528124,-0.199697230012983,
1.07633607767727));
#28821=CARTESIAN_POINT('Ctrl Pts',(0.00996567398334777,-0.177924977804098,
1.07622728347683));
#28822=CARTESIAN_POINT('Ctrl Pts',(0.0404772621979741,-0.124911173756694,
1.07556023164702));
#28823=CARTESIAN_POINT('Ctrl Pts',(0.0525234025782719,-0.0925528133349865,
1.07492508698591));
#28824=CARTESIAN_POINT('Ctrl Pts',(0.0589974094846124,-0.05953,1.07456964270265));
#28825=CARTESIAN_POINT('Origin',(-0.244773027351946,-0.05953,1.07242070340001));
#28826=CARTESIAN_POINT('Origin',(0.,-0.05953,0.));
#28827=CARTESIAN_POINT('',(-0.803348093619616,-0.05953,0.716109245731214));
#28828=CARTESIAN_POINT('Origin',(0.,-0.05953,0.));
#28829=CARTESIAN_POINT('Origin',(-0.991065754692661,-0.05953,0.477272113029314));
#28830=CARTESIAN_POINT('Origin',(-0.991065754692661,0.,0.477272113029314));
#28831=CARTESIAN_POINT('',(-1.06075609691358,-0.05953,0.181596019242328));
#28832=CARTESIAN_POINT('Ctrl Pts',(-1.06075609691358,-0.05953,0.181596019242328));
#28833=CARTESIAN_POINT('Ctrl Pts',(-1.05966202740332,-0.0925528133349865,
0.187986803072856));
#28834=CARTESIAN_POINT('Ctrl Pts',(-1.05760072925372,-0.124911173756694,
0.199872254546857));
#28835=CARTESIAN_POINT('Ctrl Pts',(-1.05146158959546,-0.177924977804098,
0.22976728653846));
#28836=CARTESIAN_POINT('Ctrl Pts',(-1.04785021111757,-0.199697230012983,
0.246078686169301));
#28837=CARTESIAN_POINT('Ctrl Pts',(-1.03846709802406,-0.237895043532788,
0.283073967563097));
#28838=CARTESIAN_POINT('Ctrl Pts',(-1.03268176429485,-0.254319232363049,
0.303755815985685));
#28839=CARTESIAN_POINT('Ctrl Pts',(-1.01919893537026,-0.28018331644634,
0.346251081972725));
#28840=CARTESIAN_POINT('Ctrl Pts',(-1.01085972381132,-0.29104845371857,
0.370184399726282));
#28841=CARTESIAN_POINT('Ctrl Pts',(-0.99154738033959,-0.30527573347708,
0.419174982698463));
#28842=CARTESIAN_POINT('Ctrl Pts',(-0.980551951791748,-0.308638795020976,
0.444223188605045));
#28843=CARTESIAN_POINT('Ctrl Pts',(-0.958671816228589,-0.308638795020976,
0.489657758261848));
#28844=CARTESIAN_POINT('Ctrl Pts',(-0.945943877838127,-0.30527573347708,
0.51387163140139));
#28845=CARTESIAN_POINT('Ctrl Pts',(-0.91968254693063,-0.29104845371857,
0.559515758398093));
#28846=CARTESIAN_POINT('Ctrl Pts',(-0.906170138993533,-0.28018331644634,
0.580957796077825));
#28847=CARTESIAN_POINT('Ctrl Pts',(-0.8813524085237,-0.254319232363049,
0.617994461173994));
#28848=CARTESIAN_POINT('Ctrl Pts',(-0.868789784891799,-0.237895043532788,
0.635412538795143));
#28849=CARTESIAN_POINT('Ctrl Pts',(-0.845715984518854,-0.199697230012983,
0.66581473268113));
#28850=CARTESIAN_POINT('Ctrl Pts',(-0.835214876415962,-0.177924977804098,
0.678808213394124));
#28851=CARTESIAN_POINT('Ctrl Pts',(-0.815669690204649,-0.124911173756694,
0.702247233627224));
#28852=CARTESIAN_POINT('Ctrl Pts',(-0.807662468433796,-0.0925528133349865,
0.711269279199861));
#28853=CARTESIAN_POINT('Ctrl Pts',(-0.803348093619616,-0.05953,0.716109245731214));
#28854=CARTESIAN_POINT('Origin',(-0.991065754692661,-0.05953,0.477272113029314));
#28855=CARTESIAN_POINT('Origin',(0.,-0.05953,0.));
#28856=CARTESIAN_POINT('',(-1.076188,-0.05953,1.31795018948079E-16));
#28857=CARTESIAN_POINT('Origin',(0.,-0.05953,0.));
#28858=CARTESIAN_POINT('',(-1.06075609691358,-0.05953,-0.181596019242328));
#28859=CARTESIAN_POINT('Origin',(0.,-0.05953,0.));
#28860=CARTESIAN_POINT('Origin',(-0.991065754692661,-0.05953,-0.477272113029314));
#28861=CARTESIAN_POINT('Origin',(-0.991065754692661,0.,-0.477272113029314));
#28862=CARTESIAN_POINT('',(-0.803348093619616,-0.05953,-0.716109245731215));
#28863=CARTESIAN_POINT('Ctrl Pts',(-0.803348093619616,-0.05953,-0.716109245731215));
#28864=CARTESIAN_POINT('Ctrl Pts',(-0.807662468433795,-0.0925528133349865,
-0.711269279199862));
#28865=CARTESIAN_POINT('Ctrl Pts',(-0.815669690204649,-0.124911173756694,
-0.702247233627224));
#28866=CARTESIAN_POINT('Ctrl Pts',(-0.835214876415962,-0.177924977804098,
-0.678808213394124));
#28867=CARTESIAN_POINT('Ctrl Pts',(-0.845715984518854,-0.199697230012983,
-0.66581473268113));
#28868=CARTESIAN_POINT('Ctrl Pts',(-0.868789784891799,-0.237895043532788,
-0.635412538795143));
#28869=CARTESIAN_POINT('Ctrl Pts',(-0.8813524085237,-0.254319232363049,
-0.617994461173994));
#28870=CARTESIAN_POINT('Ctrl Pts',(-0.906170138993533,-0.28018331644634,
-0.580957796077826));
#28871=CARTESIAN_POINT('Ctrl Pts',(-0.91968254693063,-0.29104845371857,
-0.559515758398093));
#28872=CARTESIAN_POINT('Ctrl Pts',(-0.945943877838127,-0.30527573347708,
-0.51387163140139));
#28873=CARTESIAN_POINT('Ctrl Pts',(-0.958671816228589,-0.308638795020976,
-0.489657758261848));
#28874=CARTESIAN_POINT('Ctrl Pts',(-0.980551951791748,-0.308638795020976,
-0.444223188605045));
#28875=CARTESIAN_POINT('Ctrl Pts',(-0.99154738033959,-0.30527573347708,
-0.419174982698463));
#28876=CARTESIAN_POINT('Ctrl Pts',(-1.01085972381132,-0.29104845371857,
-0.370184399726282));
#28877=CARTESIAN_POINT('Ctrl Pts',(-1.01919893537026,-0.28018331644634,
-0.346251081972725));
#28878=CARTESIAN_POINT('Ctrl Pts',(-1.03268176429485,-0.254319232363049,
-0.303755815985685));
#28879=CARTESIAN_POINT('Ctrl Pts',(-1.03846709802406,-0.237895043532788,
-0.283073967563097));
#28880=CARTESIAN_POINT('Ctrl Pts',(-1.04785021111757,-0.199697230012983,
-0.246078686169302));
#28881=CARTESIAN_POINT('Ctrl Pts',(-1.05146158959546,-0.177924977804098,
-0.229767286538461));
#28882=CARTESIAN_POINT('Ctrl Pts',(-1.05760072925372,-0.124911173756694,
-0.199872254546858));
#28883=CARTESIAN_POINT('Ctrl Pts',(-1.05966202740332,-0.0925528133349864,
-0.187986803072857));
#28884=CARTESIAN_POINT('Ctrl Pts',(-1.06075609691358,-0.05953,-0.181596019242328));
#28885=CARTESIAN_POINT('Origin',(-0.991065754692661,-0.05953,-0.477272113029314));
#28886=CARTESIAN_POINT('Origin',(0.,-0.05953,0.));
#28887=CARTESIAN_POINT('',(-0.519393123750572,-0.05953,-0.942555777842682));
#28888=CARTESIAN_POINT('Origin',(0.,-0.05953,0.));
#28889=CARTESIAN_POINT('Origin',(-0.244773027351946,-0.05953,-1.07242070340001));
#28890=CARTESIAN_POINT('Origin',(-0.244773027351946,0.,-1.07242070340001));
#28891=CARTESIAN_POINT('',(0.0589974094846125,-0.05953,-1.07456964270265));
#28892=CARTESIAN_POINT('Ctrl Pts',(0.0589974094846127,-0.05953,-1.07456964270265));
#28893=CARTESIAN_POINT('Ctrl Pts',(0.0525234025782722,-0.0925528133349865,
-1.07492508698591));
#28894=CARTESIAN_POINT('Ctrl Pts',(0.0404772621979744,-0.124911173756694,
-1.07556023164702));
#28895=CARTESIAN_POINT('Ctrl Pts',(0.0099656739833481,-0.177924977804098,
-1.07622728347683));
#28896=CARTESIAN_POINT('Ctrl Pts',(-0.00674037211528096,-0.199697230012983,
-1.07633607767727));
#28897=CARTESIAN_POINT('Ctrl Pts',(-0.044896043654098,-0.237895043532788,
-1.07542044338697));
#28898=CARTESIAN_POINT('Ctrl Pts',(-0.0663467128214644,-0.254319232363049,
-1.07438230428002));
#28899=CARTESIAN_POINT('Ctrl Pts',(-0.110776745452493,-0.28018331644634,
-1.07069360430242));
#28900=CARTESIAN_POINT('Ctrl Pts',(-0.135965654106109,-0.29104845371857,
-1.06788913840721));
#28901=CARTESIAN_POINT('Ctrl Pts',(-0.188025341585962,-0.30527573347708,
-1.05996242598502));
#28902=CARTESIAN_POINT('Ctrl Pts',(-0.214892249704082,-0.308638795020976,
-1.05481642595959));
#28903=CARTESIAN_POINT('Ctrl Pts',(-0.264056468041074,-0.308638795020976,
-1.04359501395068));
#28904=CARTESIAN_POINT('Ctrl Pts',(-0.290495481564827,-0.30527573347708,
-1.036574285215));
#28905=CARTESIAN_POINT('Ctrl Pts',(-0.340838910881557,-0.291048453718569,
-1.02112815447116));
#28906=CARTESIAN_POINT('Ctrl Pts',(-0.364750145543744,-0.28018331644634,
-1.01272583306292));
#28907=CARTESIAN_POINT('Ctrl Pts',(-0.406380688682952,-0.254319232363049,
-0.996771768218699));
#28908=CARTESIAN_POINT('Ctrl Pts',(-0.426157505475872,-0.237895043532788,
-0.988400002689705));
#28909=CARTESIAN_POINT('Ctrl Pts',(-0.460931856495794,-0.199697230012983,
-0.972669835243841));
#28910=CARTESIAN_POINT('Ctrl Pts',(-0.475936279901919,-0.177924977804098,
-0.965323333309091));
#28911=CARTESIAN_POINT('Ctrl Pts',(-0.503136848051454,-0.124911173756694,
-0.951483858396181));
#28912=CARTESIAN_POINT('Ctrl Pts',(-0.513714466572041,-0.0925528133349865,
-0.945684988399766));
#28913=CARTESIAN_POINT('Ctrl Pts',(-0.519393123750572,-0.05953,-0.942555777842682));
#28914=CARTESIAN_POINT('Origin',(-0.244773027351946,-0.05953,-1.07242070340001));
#28915=CARTESIAN_POINT('Origin',(0.,-0.05953,0.));
#28916=CARTESIAN_POINT('',(0.413083465285518,-0.05953,-0.993751811093549));
#28917=CARTESIAN_POINT('Origin',(0.,-0.05953,0.));
#28918=CARTESIAN_POINT('Origin',(0.685838782044607,-0.05953,-0.860014630714833));
#28919=CARTESIAN_POINT('Origin',(0.685838782044607,0.,-0.860014630714833));
#28920=CARTESIAN_POINT('',(0.876916659919095,-0.05953,-0.623857181492959));
#28921=CARTESIAN_POINT('Ctrl Pts',(0.876916659919095,-0.05953,-0.623857181492958));
#28922=CARTESIAN_POINT('Ctrl Pts',(0.873158080166742,-0.0925528133349865,
-0.62914037979579));
#28923=CARTESIAN_POINT('Ctrl Pts',(0.866144010579847,-0.124911173756694,
-0.638954437806245));
#28924=CARTESIAN_POINT('Ctrl Pts',(0.847641868610495,-0.177924977804098,
-0.663225258065736));
#28925=CARTESIAN_POINT('Ctrl Pts',(0.837310877969633,-0.199697230012983,
-0.676354402927683));
#28926=CARTESIAN_POINT('Ctrl Pts',(0.81280533416753,-0.237895043532788,
-0.705614819529209));
#28927=CARTESIAN_POINT('Ctrl Pts',(0.798619410861634,-0.254319232363049,
-0.721738358858166));
#28928=CARTESIAN_POINT('Ctrl Pts',(0.768033796848072,-0.28018331644634,
-0.754175290318038));
#28929=CARTESIAN_POINT('Ctrl Pts',(0.750136149454208,-0.29104845371857,
-0.772120216227122));
#28930=CARTESIAN_POINT('Ctrl Pts',(0.711480111898423,-0.30527573347708,
-0.807879894508811));
#28931=CARTESIAN_POINT('Ctrl Pts',(0.690705563850638,-0.308638795020976,
-0.825676810575913));
#28932=CARTESIAN_POINT('Ctrl Pts',(0.651278921914856,-0.308638795020976,
-0.857118508332695));
#28933=CARTESIAN_POINT('Ctrl Pts',(0.629305439856167,-0.30527573347708,
-0.873412008702649));
#28934=CARTESIAN_POINT('Ctrl Pts',(0.585840553788742,-0.29104845371857,
-0.903141581680914));
#28935=CARTESIAN_POINT('Ctrl Pts',(0.564362943424239,-0.28018331644634,
-0.916597376014514));
#28936=CARTESIAN_POINT('Ctrl Pts',(0.525933334162556,-0.254319232363049,
-0.939198248544427));
#28937=CARTESIAN_POINT('Ctrl Pts',(0.507057380724533,-0.237895043532788,
-0.949440676105255));
#28938=CARTESIAN_POINT('Ctrl Pts',(0.473077587363686,-0.199697230012983,
-0.966820759530997));
#28939=CARTESIAN_POINT('Ctrl Pts',(0.457978755888596,-0.177924977804098,
-0.973971221090534));
#28940=CARTESIAN_POINT('Ctrl Pts',(0.430199341854858,-0.124911173756694,
-0.986608710139579));
#28941=CARTESIAN_POINT('Ctrl Pts',(0.419070565453384,-0.0925528133349865,
-0.991263089003441));
#28942=CARTESIAN_POINT('Ctrl Pts',(0.413083465285518,-0.05953,-0.993751811093549));
#28943=CARTESIAN_POINT('Origin',(0.685838782044607,-0.05953,-0.860014630714833));
#28944=CARTESIAN_POINT('Origin',(0.,-0.208355,0.));
#28945=CARTESIAN_POINT('',(-1.076188,-0.35718,1.31795018948079E-16));
#28946=CARTESIAN_POINT('Origin',(0.,-0.35718,0.));
#28947=CARTESIAN_POINT('',(-1.076188,-0.208355,1.31795018948079E-16));
#28948=CARTESIAN_POINT('',(1.03449977959455,-0.05953,0.296632461748266));
#28949=CARTESIAN_POINT('Origin',(0.,-0.05953,0.));
#28950=CARTESIAN_POINT('',(1.03449977959455,-0.05953,-0.296632461748266));
#28951=CARTESIAN_POINT('Ctrl Pts',(1.03449977959455,-0.05953,0.296632461748267));
#28952=CARTESIAN_POINT('Ctrl Pts',(1.03628691421076,-0.0925528133349865,
0.290399865505497));
#28953=CARTESIAN_POINT('Ctrl Pts',(1.03958665287714,-0.124911173756694,
0.278797079997872));
#28954=CARTESIAN_POINT('Ctrl Pts',(1.0470264474309,-0.177924977804098,0.249198913998601));
#28955=CARTESIAN_POINT('Ctrl Pts',(1.05084995891418,-0.199697230012983,
0.232935932341942));
#28956=CARTESIAN_POINT('Ctrl Pts',(1.05844771715377,-0.237895043532788,
0.195533155353269));
#28957=CARTESIAN_POINT('Ctrl Pts',(1.06220882929878,-0.254319232363049,
0.17438929156337));
#28958=CARTESIAN_POINT('Ctrl Pts',(1.06849922508772,-0.28018331644634,0.130252399648131));
#28959=CARTESIAN_POINT('Ctrl Pts',(1.07137013248666,-0.29104845371857,0.105070977154072));
#28960=CARTESIAN_POINT('Ctrl Pts',(1.07522652957392,-0.30527573347708,0.0525526752791107));
#28961=CARTESIAN_POINT('Ctrl Pts',(1.076188,-0.308638795020976,0.025214283908933));
#28962=CARTESIAN_POINT('Ctrl Pts',(1.076188,-0.308638795020976,-0.025214283908933));
#28963=CARTESIAN_POINT('Ctrl Pts',(1.07522652957392,-0.30527573347708,-0.0525526752791107));
#28964=CARTESIAN_POINT('Ctrl Pts',(1.07137013248666,-0.29104845371857,-0.105070977154072));
#28965=CARTESIAN_POINT('Ctrl Pts',(1.06849922508772,-0.28018331644634,-0.130252399648131));
#28966=CARTESIAN_POINT('Ctrl Pts',(1.06220882929878,-0.254319232363049,
-0.17438929156337));
#28967=CARTESIAN_POINT('Ctrl Pts',(1.05844771715377,-0.237895043532788,
-0.195533155353269));
#28968=CARTESIAN_POINT('Ctrl Pts',(1.05084995891418,-0.199697230012983,
-0.232935932341942));
#28969=CARTESIAN_POINT('Ctrl Pts',(1.0470264474309,-0.177924977804098,-0.249198913998601));
#28970=CARTESIAN_POINT('Ctrl Pts',(1.03958665287714,-0.124911173756694,
-0.278797079997872));
#28971=CARTESIAN_POINT('Ctrl Pts',(1.03628691421076,-0.0925528133349865,
-0.290399865505497));
#28972=CARTESIAN_POINT('Ctrl Pts',(1.03449977959455,-0.05953,-0.296632461748267));
#28973=CARTESIAN_POINT('Origin',(0.,-0.05953,0.));
#28974=CARTESIAN_POINT('Origin',(0.,-0.05953,0.));
#28975=CARTESIAN_POINT('Origin',(1.1,-0.05953,0.));
#28976=CARTESIAN_POINT('Origin',(1.1,0.,0.));
#28977=CARTESIAN_POINT('Origin',(1.1,-0.05953,0.));
#28978=CARTESIAN_POINT('Origin',(0.,-0.35718,0.));
#28979=CARTESIAN_POINT('Origin',(0.,-0.05953,0.));
#28980=CARTESIAN_POINT('',(0.,0.,0.));
#28981=CARTESIAN_POINT('Origin',(1.119765,0.495,0.));
#28982=CARTESIAN_POINT('',(-1.119765,0.495,-1.37131662304724E-16));
#28983=CARTESIAN_POINT('Origin',(0.,0.495,0.));
#28984=CARTESIAN_POINT('',(-1.085235,0.495,-1.32902956907268E-16));
#28985=CARTESIAN_POINT('Origin',(0.,0.495,0.));
#28986=CARTESIAN_POINT('Origin',(0.,0.4575,0.));
#28987=CARTESIAN_POINT('',(-1.119765,0.42,-1.37131662304724E-16));
#28988=CARTESIAN_POINT('Origin',(0.,0.42,0.));
#28989=CARTESIAN_POINT('',(-1.119765,0.4575,-1.37131662304724E-16));
#28990=CARTESIAN_POINT('Origin',(1.085235,0.42,0.));
#28991=CARTESIAN_POINT('',(-1.085235,0.42,-1.32902956907268E-16));
#28992=CARTESIAN_POINT('Origin',(0.,0.42,0.));
#28993=CARTESIAN_POINT('Origin',(0.,0.4575,0.));
#28994=CARTESIAN_POINT('',(-1.085235,0.4575,-1.32902956907268E-16));
#28995=CARTESIAN_POINT('Origin',(1.119765,-0.42,0.));
#28996=CARTESIAN_POINT('',(-1.119765,-0.42,-1.37131662304724E-16));
#28997=CARTESIAN_POINT('Origin',(0.,-0.42,0.));
#28998=CARTESIAN_POINT('',(-1.085235,-0.42,-1.32902956907268E-16));
#28999=CARTESIAN_POINT('Origin',(0.,-0.42,0.));
#29000=CARTESIAN_POINT('Origin',(0.,-0.4575,0.));
#29001=CARTESIAN_POINT('',(-1.119765,-0.495,-1.37131662304724E-16));
#29002=CARTESIAN_POINT('Origin',(0.,-0.495,0.));
#29003=CARTESIAN_POINT('',(-1.119765,-0.4575,-1.37131662304724E-16));
#29004=CARTESIAN_POINT('Origin',(1.085235,-0.495,0.));
#29005=CARTESIAN_POINT('',(-1.085235,-0.495,-1.32902956907268E-16));
#29006=CARTESIAN_POINT('Origin',(0.,-0.495,0.));
#29007=CARTESIAN_POINT('Origin',(0.,-0.4575,0.));
#29008=CARTESIAN_POINT('',(-1.085235,-0.4575,-1.32902956907268E-16));
#29009=CARTESIAN_POINT('',(0.,0.,0.));
#29010=CARTESIAN_POINT('',(0.,0.,0.));
#29011=CARTESIAN_POINT('',(0.,0.,0.));
#29012=CARTESIAN_POINT('',(0.,0.,0.));
#29013=CARTESIAN_POINT('',(0.,0.,0.));
#29014=CARTESIAN_POINT('',(0.,0.,0.));
#29015=CARTESIAN_POINT('',(0.,0.,0.));
#29016=CARTESIAN_POINT('Origin',(0.,0.,0.));
#29017=CARTESIAN_POINT('',(-1.63531,-0.410863395882378,-2.00267715711366E-16));
#29018=CARTESIAN_POINT('',(-2.00267715711366E-16,-0.410863395882378,1.63531));
#29019=CARTESIAN_POINT('Origin',(0.,-0.410863395882378,0.));
#29020=CARTESIAN_POINT('Origin',(0.,-0.410863395882378,0.));
#29021=CARTESIAN_POINT('',(-2.00267715711366E-16,0.410863395882378,1.63531));
#29022=CARTESIAN_POINT('Origin',(-2.05128338857182E-16,0.,1.675));
#29023=CARTESIAN_POINT('',(-1.63531,0.410863395882378,2.00267715711366E-16));
#29024=CARTESIAN_POINT('Origin',(0.,0.410863395882378,0.));
#29025=CARTESIAN_POINT('Origin',(0.,0.410863395882378,0.));
#29026=CARTESIAN_POINT('Origin',(0.,0.,0.));
#29027=CARTESIAN_POINT('',(-1.63531,0.7,-2.00267715711366E-16));
#29028=CARTESIAN_POINT('',(-1.63531,0.,-2.00267715711366E-16));
#29029=CARTESIAN_POINT('Origin',(0.,0.7,0.));
#29030=CARTESIAN_POINT('Origin',(0.,0.,0.));
#29031=CARTESIAN_POINT('',(-1.,-0.6,-1.22464679914735E-16));
#29032=CARTESIAN_POINT('Origin',(0.,-0.6,0.));
#29033=CARTESIAN_POINT('',(-1.,0.6,-1.22464679914735E-16));
#29034=CARTESIAN_POINT('',(-1.,0.,-1.22464679914735E-16));
#29035=CARTESIAN_POINT('Origin',(0.,0.6,0.));
#29036=CARTESIAN_POINT('Origin',(0.,0.65,0.));
#29037=CARTESIAN_POINT('',(-1.1,0.7,-1.34711147906209E-16));
#29038=CARTESIAN_POINT('',(-1.05,0.65,-1.28587913910472E-16));
#29039=CARTESIAN_POINT('Origin',(0.,0.7,0.));
#29040=CARTESIAN_POINT('Origin',(1.63531,0.7,0.));
#29041=CARTESIAN_POINT('Origin',(0.,0.,0.));
#29042=CARTESIAN_POINT('',(-1.63531,-0.7,-2.00267715711366E-16));
#29043=CARTESIAN_POINT('Origin',(0.,-0.7,0.));
#29044=CARTESIAN_POINT('',(-1.63531,0.,-2.00267715711366E-16));
#29045=CARTESIAN_POINT('Origin',(1.1,-0.7,0.));
#29046=CARTESIAN_POINT('',(-1.1,-0.7,-1.34711147906209E-16));
#29047=CARTESIAN_POINT('Origin',(0.,-0.7,0.));
#29048=CARTESIAN_POINT('Origin',(0.,-0.65,0.));
#29049=CARTESIAN_POINT('',(-1.05,-0.65,-1.28587913910472E-16));
#29050=CARTESIAN_POINT('',(0.,0.,0.));
#29051=CARTESIAN_POINT('Origin',(0.,0.,0.));
#29052=CARTESIAN_POINT('',(-1.71469,0.410863395882378,-2.09988962002998E-16));
#29053=CARTESIAN_POINT('',(-2.09988962002998E-16,0.410863395882378,1.71469));
#29054=CARTESIAN_POINT('Origin',(0.,0.410863395882378,0.));
#29055=CARTESIAN_POINT('Origin',(0.,0.410863395882378,0.));
#29056=CARTESIAN_POINT('',(-2.09988962002998E-16,-0.410863395882378,1.71469));
#29057=CARTESIAN_POINT('Origin',(-2.05128338857182E-16,0.,1.675));
#29058=CARTESIAN_POINT('',(-1.71469,-0.410863395882378,2.09988962002998E-16));
#29059=CARTESIAN_POINT('Origin',(0.,-0.410863395882378,0.));
#29060=CARTESIAN_POINT('Origin',(0.,-0.410863395882378,0.));
#29061=CARTESIAN_POINT('Origin',(0.,0.,0.));
#29062=CARTESIAN_POINT('',(-1.71469,-0.7,-2.09988962002998E-16));
#29063=CARTESIAN_POINT('Origin',(0.,-0.7,0.));
#29064=CARTESIAN_POINT('',(-1.71469,0.,-2.09988962002998E-16));
#29065=CARTESIAN_POINT('Origin',(2.25,0.7,0.));
#29066=CARTESIAN_POINT('',(-2.25,0.7,-2.75545529808154E-16));
#29067=CARTESIAN_POINT('Origin',(0.,0.7,0.));
#29068=CARTESIAN_POINT('',(-1.71469,0.7,-2.09988962002998E-16));
#29069=CARTESIAN_POINT('Origin',(0.,0.7,0.));
#29070=CARTESIAN_POINT('Origin',(0.,0.65,0.));
#29071=CARTESIAN_POINT('',(-2.35,0.6,-2.87791997799628E-16));
#29072=CARTESIAN_POINT('Origin',(0.,0.6,0.));
#29073=CARTESIAN_POINT('',(-2.3,0.65,-2.81668763803891E-16));
#29074=CARTESIAN_POINT('Origin',(0.,0.,0.));
#29075=CARTESIAN_POINT('',(-2.35,-0.6,-2.87791997799628E-16));
#29076=CARTESIAN_POINT('Origin',(0.,-0.6,0.));
#29077=CARTESIAN_POINT('',(-2.35,0.,-2.87791997799628E-16));
#29078=CARTESIAN_POINT('Origin',(0.,-0.65,0.));
#29079=CARTESIAN_POINT('',(-2.25,-0.7,-2.75545529808154E-16));
#29080=CARTESIAN_POINT('Origin',(0.,-0.7,0.));
#29081=CARTESIAN_POINT('',(-2.3,-0.65,-2.81668763803891E-16));
#29082=CARTESIAN_POINT('Origin',(1.71469,-0.7,0.));
#29083=CARTESIAN_POINT('Origin',(0.,0.,0.));
#29084=CARTESIAN_POINT('',(-1.71469,0.,-2.09988962002998E-16));
#29085=CARTESIAN_POINT('',(0.,0.,0.));
#29086=CARTESIAN_POINT('Origin',(1.675,0.,0.));
#29087=CARTESIAN_POINT('',(1.675,-2.97627328869245E-33,0.3969));
#29088=CARTESIAN_POINT('',(1.675,-2.97627328869245E-33,-0.3969));
#29089=CARTESIAN_POINT('Origin',(1.675,0.,0.));
#29090=CARTESIAN_POINT('Origin',(1.18440385848747,0.,-1.18440385848747));
#29091=CARTESIAN_POINT('',(1.46505453994041,3.1867025333467E-33,-0.903753177034526));
#29092=CARTESIAN_POINT('',(0.903753177034527,-9.13924911073161E-33,-1.46505453994041));
#29093=CARTESIAN_POINT('Origin',(1.18440385848747,0.,-1.18440385848747));
#29094=CARTESIAN_POINT('Origin',(1.02564169428591E-16,0.,-1.675));
#29095=CARTESIAN_POINT('',(0.3969,-2.97627328869246E-33,-1.675));
#29096=CARTESIAN_POINT('',(-0.3969,-2.97627328869245E-33,-1.675));
#29097=CARTESIAN_POINT('Origin',(1.02564169428591E-16,0.,-1.675));
#29098=CARTESIAN_POINT('Origin',(-1.18440385848747,0.,-1.18440385848747));
#29099=CARTESIAN_POINT('',(-0.903753177034526,3.1867025333467E-33,-1.46505453994041));
#29100=CARTESIAN_POINT('',(-1.46505453994041,-9.13924911073161E-33,-0.903753177034527));
#29101=CARTESIAN_POINT('Origin',(-1.18440385848747,0.,-1.18440385848747));
#29102=CARTESIAN_POINT('Origin',(-1.675,0.,-2.05128338857182E-16));
#29103=CARTESIAN_POINT('',(-1.675,-2.97627328869246E-33,-0.3969));
#29104=CARTESIAN_POINT('',(-1.675,-2.97627328869245E-33,0.3969));
#29105=CARTESIAN_POINT('Origin',(-1.675,0.,-2.05128338857182E-16));
#29106=CARTESIAN_POINT('Origin',(-1.18440385848747,0.,1.18440385848747));
#29107=CARTESIAN_POINT('',(-1.46505453994041,6.26819044436628E-33,0.903753177034526));
#29108=CARTESIAN_POINT('',(-0.903753177034527,-1.22207370217512E-32,1.46505453994041));
#29109=CARTESIAN_POINT('Origin',(-1.18440385848747,0.,1.18440385848747));
#29110=CARTESIAN_POINT('Origin',(-3.07692508285772E-16,0.,1.675));
#29111=CARTESIAN_POINT('',(-0.3969,-2.97627328869246E-33,1.675));
#29112=CARTESIAN_POINT('',(0.396899999999999,-2.97627328869245E-33,1.675));
#29113=CARTESIAN_POINT('Origin',(-3.07692508285772E-16,0.,1.675));
#29114=CARTESIAN_POINT('Origin',(1.18440385848747,0.,1.18440385848747));
#29115=CARTESIAN_POINT('',(0.903753177034526,9.34967835538585E-33,1.46505453994041));
#29116=CARTESIAN_POINT('',(1.46505453994041,-1.53022249327708E-32,0.903753177034527));
#29117=CARTESIAN_POINT('Origin',(1.18440385848747,0.,1.18440385848747));
#29118=CARTESIAN_POINT('',(0.,0.,0.));
#29119=CARTESIAN_POINT('Origin',(1.18440385848747,0.,1.18440385848747));
#29120=CARTESIAN_POINT('',(0.846804978391753,-0.07938,1.40825612658882));
#29121=CARTESIAN_POINT('',(1.40825612658882,-0.07938,0.846804978391754));
#29122=CARTESIAN_POINT('Ctrl Pts',(0.846804978391752,-0.0793800000000001,
1.40825612658882));
#29123=CARTESIAN_POINT('Ctrl Pts',(0.854205272175554,-0.123401821157026,
1.40380622184538));
#29124=CARTESIAN_POINT('Ctrl Pts',(0.867957148219441,-0.166543350814306,
1.39550172959303));
#29125=CARTESIAN_POINT('Ctrl Pts',(0.902193646979982,-0.237231147975234,
1.3735491215176));
#29126=CARTESIAN_POINT('Ctrl Pts',(0.920778333482564,-0.266264900654909,
1.36127834356734));
#29127=CARTESIAN_POINT('Ctrl Pts',(0.962485392528369,-0.317195968905306,
1.33211611256184));
#29128=CARTESIAN_POINT('Ctrl Pts',(0.985600426557816,-0.33909093068465,
1.31521005565926));
#29129=CARTESIAN_POINT('Ctrl Pts',(1.03253285680459,-0.373586846396559,
1.27866649102984));
#29130=CARTESIAN_POINT('Ctrl Pts',(1.05871835910697,-0.388086240756494,
1.25722555095714));
#29131=CARTESIAN_POINT('Ctrl Pts',(1.11153475808518,-0.407068917407805,
1.2107812086231));
#29132=CARTESIAN_POINT('Ctrl Pts',(1.13814686046673,-0.411552957311693,
1.18575674747573));
#29133=CARTESIAN_POINT('Ctrl Pts',(1.18575674747573,-0.411552957311693,
1.13814686046673));
#29134=CARTESIAN_POINT('Ctrl Pts',(1.2107812086231,-0.407068917407805,1.11153475808518));
#29135=CARTESIAN_POINT('Ctrl Pts',(1.25722555095713,-0.388086240756494,
1.05871835910697));
#29136=CARTESIAN_POINT('Ctrl Pts',(1.27866649102984,-0.373586846396559,
1.03253285680459));
#29137=CARTESIAN_POINT('Ctrl Pts',(1.31521005565926,-0.33909093068465,0.985600426557816));
#29138=CARTESIAN_POINT('Ctrl Pts',(1.33211611256184,-0.317195968905306,
0.962485392528369));
#29139=CARTESIAN_POINT('Ctrl Pts',(1.36127834356734,-0.266264900654909,
0.920778333482565));
#29140=CARTESIAN_POINT('Ctrl Pts',(1.3735491215176,-0.237231147975234,0.902193646979983));
#29141=CARTESIAN_POINT('Ctrl Pts',(1.39550172959303,-0.166543350814306,
0.867957148219442));
#29142=CARTESIAN_POINT('Ctrl Pts',(1.40380622184538,-0.123401821157026,
0.854205272175555));
#29143=CARTESIAN_POINT('Ctrl Pts',(1.40825612658882,-0.0793800000000001,
0.846804978391753));
#29144=CARTESIAN_POINT('',(0.886256117232623,-0.07938,1.45861320581289));
#29145=CARTESIAN_POINT('Origin',(1.18440385848747,-0.07938,1.18440385848747));
#29146=CARTESIAN_POINT('',(1.45861320581289,-0.07938,0.886256117232624));
#29147=CARTESIAN_POINT('Ctrl Pts',(1.45861320581289,-0.0793800000000001,
0.886256117232623));
#29148=CARTESIAN_POINT('Ctrl Pts',(1.45630208793976,-0.101649918886749,
0.890059788636852));
#29149=CARTESIAN_POINT('Ctrl Pts',(1.45296717977858,-0.123823518623746,
0.895520212222107));
#29150=CARTESIAN_POINT('Ctrl Pts',(1.43904931717599,-0.192480977588836,
0.917859913453975));
#29151=CARTESIAN_POINT('Ctrl Pts',(1.4243271592157,-0.236152929235938,0.940896403863072));
#29152=CARTESIAN_POINT('Ctrl Pts',(1.39055359345152,-0.303141259068212,
0.990027513266106));
#29153=CARTESIAN_POINT('Ctrl Pts',(1.36743459453896,-0.335108247315849,
1.02199477007745));
#29154=CARTESIAN_POINT('Ctrl Pts',(1.32643091652006,-0.373243761060364,
1.07446535104584));
#29155=CARTESIAN_POINT('Ctrl Pts',(1.30441816675528,-0.387888272594439,
1.10126842659597));
#29156=CARTESIAN_POINT('Ctrl Pts',(1.25681160160691,-0.407041111792943,
1.15530234155453));
#29157=CARTESIAN_POINT('Ctrl Pts',(1.23119764287622,-0.411552957311693,
1.18251418313119));
#29158=CARTESIAN_POINT('Ctrl Pts',(1.18251418313119,-0.411552957311693,
1.23119764287622));
#29159=CARTESIAN_POINT('Ctrl Pts',(1.15530234155453,-0.407041111792943,
1.25681160160691));
#29160=CARTESIAN_POINT('Ctrl Pts',(1.10126842659597,-0.387888272594439,
1.30441816675528));
#29161=CARTESIAN_POINT('Ctrl Pts',(1.07446535104584,-0.373243761060364,
1.32643091652006));
#29162=CARTESIAN_POINT('Ctrl Pts',(1.02199477007745,-0.335108247315848,
1.36743459453896));
#29163=CARTESIAN_POINT('Ctrl Pts',(0.990027513266105,-0.303141259068211,
1.39055359345152));
#29164=CARTESIAN_POINT('Ctrl Pts',(0.940896403863071,-0.236152929235937,
1.42432715921571));
#29165=CARTESIAN_POINT('Ctrl Pts',(0.917859913453974,-0.192480977588835,
1.43904931717599));
#29166=CARTESIAN_POINT('Ctrl Pts',(0.895520212222106,-0.123823518623745,
1.45296717977858));
#29167=CARTESIAN_POINT('Ctrl Pts',(0.890059788636851,-0.101649918886749,
1.45630208793976));
#29168=CARTESIAN_POINT('Ctrl Pts',(0.886256117232622,-0.0793800000000001,
1.45861320581289));
#29169=CARTESIAN_POINT('Origin',(1.18440385848747,-0.07938,1.18440385848747));
#29170=CARTESIAN_POINT('Origin',(0.,-0.27783,0.));
#29171=CARTESIAN_POINT('',(0.404717578595295,-0.07938,1.65807299932179));
#29172=CARTESIAN_POINT('Origin',(0.,-0.07938,0.));
#29173=CARTESIAN_POINT('',(-0.404717578595296,-0.07938,1.65807299932179));
#29174=CARTESIAN_POINT('Ctrl Pts',(0.404717578595296,-0.0793800000000001,
1.65807299932179));
#29175=CARTESIAN_POINT('Ctrl Pts',(0.400393769631747,-0.101649918886749,
1.65912839404491));
#29176=CARTESIAN_POINT('Ctrl Pts',(0.394174530911058,-0.123823518623745,
1.66063136041479));
#29177=CARTESIAN_POINT('Ctrl Pts',(0.368536561654407,-0.192480977588835,
1.66658649961961));
#29178=CARTESIAN_POINT('Ctrl Pts',(0.341837165343982,-0.236152929235937,
1.67246562047521));
#29179=CARTESIAN_POINT('Ctrl Pts',(0.283214707341173,-0.303141259068211,
1.68332504372461));
#29180=CARTESIAN_POINT('Ctrl Pts',(0.244262842368623,-0.335108247315849,
1.68958170688653));
#29181=CARTESIAN_POINT('Ctrl Pts',(0.178166559972324,-0.373243761060364,
1.69769003172132));
#29182=CARTESIAN_POINT('Ctrl Pts',(0.143648558862931,-0.387888272594439,
1.70107730356824));
#29183=CARTESIAN_POINT('Ctrl Pts',(0.0717778861362652,-0.407041111792943,
1.70562212620408));
#29184=CARTESIAN_POINT('Ctrl Pts',(0.0344244045173309,-0.411552957311693,
1.706752));
#29185=CARTESIAN_POINT('Ctrl Pts',(-0.0344244045173315,-0.411552957311693,
1.706752));
#29186=CARTESIAN_POINT('Ctrl Pts',(-0.0717778861362658,-0.407041111792943,
1.70562212620408));
#29187=CARTESIAN_POINT('Ctrl Pts',(-0.143648558862932,-0.387888272594439,
1.70107730356824));
#29188=CARTESIAN_POINT('Ctrl Pts',(-0.178166559972325,-0.373243761060364,
1.69769003172132));
#29189=CARTESIAN_POINT('Ctrl Pts',(-0.244262842368624,-0.335108247315849,
1.68958170688653));
#29190=CARTESIAN_POINT('Ctrl Pts',(-0.283214707341173,-0.303141259068212,
1.68332504372461));
#29191=CARTESIAN_POINT('Ctrl Pts',(-0.341837165343982,-0.236152929235937,
1.67246562047521));
#29192=CARTESIAN_POINT('Ctrl Pts',(-0.368536561654408,-0.192480977588835,
1.66658649961961));
#29193=CARTESIAN_POINT('Ctrl Pts',(-0.394174530911059,-0.123823518623745,
1.66063136041479));
#29194=CARTESIAN_POINT('Ctrl Pts',(-0.400393769631748,-0.101649918886749,
1.65912839404491));
#29195=CARTESIAN_POINT('Ctrl Pts',(-0.404717578595297,-0.0793800000000001,
1.65807299932179));
#29196=CARTESIAN_POINT('',(-0.886256117232624,-0.07938,1.45861320581289));
#29197=CARTESIAN_POINT('Origin',(0.,-0.07938,0.));
#29198=CARTESIAN_POINT('',(-1.45861320581289,-0.07938,0.886256117232623));
#29199=CARTESIAN_POINT('Ctrl Pts',(-0.886256117232623,-0.0793800000000001,
1.45861320581289));
#29200=CARTESIAN_POINT('Ctrl Pts',(-0.890059788636852,-0.101649918886749,
1.45630208793976));
#29201=CARTESIAN_POINT('Ctrl Pts',(-0.895520212222106,-0.123823518623745,
1.45296717977858));
#29202=CARTESIAN_POINT('Ctrl Pts',(-0.917859913453974,-0.192480977588835,
1.43904931717599));
#29203=CARTESIAN_POINT('Ctrl Pts',(-0.940896403863071,-0.236152929235937,
1.4243271592157));
#29204=CARTESIAN_POINT('Ctrl Pts',(-0.990027513266105,-0.303141259068211,
1.39055359345152));
#29205=CARTESIAN_POINT('Ctrl Pts',(-1.02199477007745,-0.335108247315848,
1.36743459453896));
#29206=CARTESIAN_POINT('Ctrl Pts',(-1.07446535104584,-0.373243761060364,
1.32643091652006));
#29207=CARTESIAN_POINT('Ctrl Pts',(-1.10126842659597,-0.387888272594439,
1.30441816675528));
#29208=CARTESIAN_POINT('Ctrl Pts',(-1.15530234155453,-0.407041111792943,
1.25681160160691));
#29209=CARTESIAN_POINT('Ctrl Pts',(-1.18251418313119,-0.411552957311693,
1.23119764287622));
#29210=CARTESIAN_POINT('Ctrl Pts',(-1.23119764287622,-0.411552957311693,
1.18251418313119));
#29211=CARTESIAN_POINT('Ctrl Pts',(-1.25681160160691,-0.407041111792943,
1.15530234155453));
#29212=CARTESIAN_POINT('Ctrl Pts',(-1.30441816675528,-0.387888272594439,
1.10126842659597));
#29213=CARTESIAN_POINT('Ctrl Pts',(-1.32643091652006,-0.373243761060365,
1.07446535104584));
#29214=CARTESIAN_POINT('Ctrl Pts',(-1.36743459453896,-0.335108247315849,
1.02199477007745));
#29215=CARTESIAN_POINT('Ctrl Pts',(-1.39055359345152,-0.303141259068212,
0.990027513266106));
#29216=CARTESIAN_POINT('Ctrl Pts',(-1.4243271592157,-0.236152929235938,
0.940896403863071));
#29217=CARTESIAN_POINT('Ctrl Pts',(-1.43904931717599,-0.192480977588836,
0.917859913453974));
#29218=CARTESIAN_POINT('Ctrl Pts',(-1.45296717977858,-0.123823518623746,
0.895520212222106));
#29219=CARTESIAN_POINT('Ctrl Pts',(-1.45630208793976,-0.101649918886749,
0.890059788636852));
#29220=CARTESIAN_POINT('Ctrl Pts',(-1.45861320581289,-0.0793800000000001,
0.886256117232623));
#29221=CARTESIAN_POINT('',(-1.65807299932179,-0.07938,0.404717578595295));
#29222=CARTESIAN_POINT('Origin',(0.,-0.07938,0.));
#29223=CARTESIAN_POINT('',(-1.706752,-0.411552957311693,2.08591827245526E-16));
#29224=CARTESIAN_POINT('Ctrl Pts',(-1.65807299932179,-0.0793800000000001,
0.404717578595296));
#29225=CARTESIAN_POINT('Ctrl Pts',(-1.65912839404491,-0.101649918886749,
0.400393769631747));
#29226=CARTESIAN_POINT('Ctrl Pts',(-1.66063136041479,-0.123823518623745,
0.394174530911058));
#29227=CARTESIAN_POINT('Ctrl Pts',(-1.66658649961961,-0.192480977588835,
0.368536561654407));
#29228=CARTESIAN_POINT('Ctrl Pts',(-1.67246562047521,-0.236152929235937,
0.341837165343982));
#29229=CARTESIAN_POINT('Ctrl Pts',(-1.68332504372461,-0.303141259068211,
0.283214707341173));
#29230=CARTESIAN_POINT('Ctrl Pts',(-1.68958170688653,-0.335108247315848,
0.244262842368623));
#29231=CARTESIAN_POINT('Ctrl Pts',(-1.69769003172132,-0.373243761060364,
0.178166559972324));
#29232=CARTESIAN_POINT('Ctrl Pts',(-1.70107730356824,-0.387888272594439,
0.143648558862931));
#29233=CARTESIAN_POINT('Ctrl Pts',(-1.70562212620408,-0.407041111792943,
0.0717778861362656));
#29234=CARTESIAN_POINT('Ctrl Pts',(-1.706752,-0.411552957311693,0.0344244045173313));
#29235=CARTESIAN_POINT('Ctrl Pts',(-1.706752,-0.411552957311693,2.08166817117217E-16));
#29236=CARTESIAN_POINT('',(-1.706752,-0.47628,2.09016837373834E-16));
#29237=CARTESIAN_POINT('',(-1.706752,-0.27783,2.09016837373834E-16));
#29238=CARTESIAN_POINT('Origin',(0.,-0.47628,0.));
#29239=CARTESIAN_POINT('',(-1.65807299932179,-0.07938,-0.404717578595296));
#29240=CARTESIAN_POINT('Ctrl Pts',(-1.706752,-0.411552957311693,2.0122792321331E-16));
#29241=CARTESIAN_POINT('Ctrl Pts',(-1.706752,-0.411552957311693,-0.0344244045173309));
#29242=CARTESIAN_POINT('Ctrl Pts',(-1.70562212620408,-0.407041111792943,
-0.0717778861362652));
#29243=CARTESIAN_POINT('Ctrl Pts',(-1.70107730356824,-0.387888272594439,
-0.143648558862931));
#29244=CARTESIAN_POINT('Ctrl Pts',(-1.69769003172132,-0.373243761060365,
-0.178166559972324));
#29245=CARTESIAN_POINT('Ctrl Pts',(-1.68958170688653,-0.335108247315849,
-0.244262842368623));
#29246=CARTESIAN_POINT('Ctrl Pts',(-1.68332504372461,-0.303141259068212,
-0.283214707341173));
#29247=CARTESIAN_POINT('Ctrl Pts',(-1.67246562047521,-0.236152929235938,
-0.341837165343982));
#29248=CARTESIAN_POINT('Ctrl Pts',(-1.66658649961961,-0.192480977588836,
-0.368536561654407));
#29249=CARTESIAN_POINT('Ctrl Pts',(-1.66063136041479,-0.123823518623745,
-0.394174530911059));
#29250=CARTESIAN_POINT('Ctrl Pts',(-1.65912839404491,-0.101649918886749,
-0.400393769631748));
#29251=CARTESIAN_POINT('Ctrl Pts',(-1.65807299932179,-0.0793800000000001,
-0.404717578595296));
#29252=CARTESIAN_POINT('',(-1.45861320581289,-0.07938,-0.886256117232623));
#29253=CARTESIAN_POINT('Origin',(0.,-0.07938,0.));
#29254=CARTESIAN_POINT('',(-0.886256117232623,-0.07938,-1.45861320581289));
#29255=CARTESIAN_POINT('Ctrl Pts',(-1.45861320581289,-0.0793800000000001,
-0.886256117232623));
#29256=CARTESIAN_POINT('Ctrl Pts',(-1.45630208793976,-0.101649918886749,
-0.890059788636852));
#29257=CARTESIAN_POINT('Ctrl Pts',(-1.45296717977858,-0.123823518623745,
-0.895520212222106));
#29258=CARTESIAN_POINT('Ctrl Pts',(-1.43904931717599,-0.192480977588835,
-0.917859913453974));
#29259=CARTESIAN_POINT('Ctrl Pts',(-1.4243271592157,-0.236152929235937,
-0.940896403863072));
#29260=CARTESIAN_POINT('Ctrl Pts',(-1.39055359345152,-0.303141259068212,
-0.990027513266106));
#29261=CARTESIAN_POINT('Ctrl Pts',(-1.36743459453896,-0.335108247315849,
-1.02199477007745));
#29262=CARTESIAN_POINT('Ctrl Pts',(-1.32643091652006,-0.373243761060364,
-1.07446535104584));
#29263=CARTESIAN_POINT('Ctrl Pts',(-1.30441816675528,-0.387888272594439,
-1.10126842659597));
#29264=CARTESIAN_POINT('Ctrl Pts',(-1.25681160160691,-0.407041111792943,
-1.15530234155453));
#29265=CARTESIAN_POINT('Ctrl Pts',(-1.23119764287622,-0.411552957311693,
-1.18251418313119));
#29266=CARTESIAN_POINT('Ctrl Pts',(-1.18251418313119,-0.411552957311693,
-1.23119764287622));
#29267=CARTESIAN_POINT('Ctrl Pts',(-1.15530234155453,-0.407041111792943,
-1.25681160160691));
#29268=CARTESIAN_POINT('Ctrl Pts',(-1.10126842659597,-0.387888272594439,
-1.30441816675528));
#29269=CARTESIAN_POINT('Ctrl Pts',(-1.07446535104584,-0.373243761060364,
-1.32643091652006));
#29270=CARTESIAN_POINT('Ctrl Pts',(-1.02199477007745,-0.335108247315848,
-1.36743459453896));
#29271=CARTESIAN_POINT('Ctrl Pts',(-0.990027513266105,-0.303141259068211,
-1.39055359345152));
#29272=CARTESIAN_POINT('Ctrl Pts',(-0.940896403863071,-0.236152929235936,
-1.42432715921571));
#29273=CARTESIAN_POINT('Ctrl Pts',(-0.917859913453974,-0.192480977588835,
-1.43904931717599));
#29274=CARTESIAN_POINT('Ctrl Pts',(-0.895520212222106,-0.123823518623745,
-1.45296717977858));
#29275=CARTESIAN_POINT('Ctrl Pts',(-0.890059788636851,-0.101649918886749,
-1.45630208793976));
#29276=CARTESIAN_POINT('Ctrl Pts',(-0.886256117232623,-0.0793800000000001,
-1.45861320581289));
#29277=CARTESIAN_POINT('',(-0.404717578595295,-0.07938,-1.65807299932179));
#29278=CARTESIAN_POINT('Origin',(0.,-0.07938,0.));
#29279=CARTESIAN_POINT('',(0.404717578595296,-0.07938,-1.65807299932179));
#29280=CARTESIAN_POINT('Ctrl Pts',(-0.404717578595296,-0.0793800000000001,
-1.65807299932179));
#29281=CARTESIAN_POINT('Ctrl Pts',(-0.400393769631747,-0.101649918886749,
-1.65912839404491));
#29282=CARTESIAN_POINT('Ctrl Pts',(-0.394174530911058,-0.123823518623746,
-1.66063136041479));
#29283=CARTESIAN_POINT('Ctrl Pts',(-0.368536561654407,-0.192480977588836,
-1.66658649961961));
#29284=CARTESIAN_POINT('Ctrl Pts',(-0.341837165343982,-0.236152929235938,
-1.67246562047521));
#29285=CARTESIAN_POINT('Ctrl Pts',(-0.283214707341173,-0.303141259068212,
-1.68332504372461));
#29286=CARTESIAN_POINT('Ctrl Pts',(-0.244262842368623,-0.335108247315849,
-1.68958170688653));
#29287=CARTESIAN_POINT('Ctrl Pts',(-0.178166559972324,-0.373243761060364,
-1.69769003172132));
#29288=CARTESIAN_POINT('Ctrl Pts',(-0.143648558862931,-0.387888272594439,
-1.70107730356824));
#29289=CARTESIAN_POINT('Ctrl Pts',(-0.0717778861362653,-0.407041111792943,
-1.70562212620408));
#29290=CARTESIAN_POINT('Ctrl Pts',(-0.034424404517331,-0.411552957311693,
-1.706752));
#29291=CARTESIAN_POINT('Ctrl Pts',(0.0344244045173312,-0.411552957311693,
-1.706752));
#29292=CARTESIAN_POINT('Ctrl Pts',(0.0717778861362655,-0.407041111792943,
-1.70562212620408));
#29293=CARTESIAN_POINT('Ctrl Pts',(0.143648558862931,-0.387888272594439,
-1.70107730356824));
#29294=CARTESIAN_POINT('Ctrl Pts',(0.178166559972324,-0.373243761060364,
-1.69769003172132));
#29295=CARTESIAN_POINT('Ctrl Pts',(0.244262842368623,-0.335108247315849,
-1.68958170688653));
#29296=CARTESIAN_POINT('Ctrl Pts',(0.283214707341173,-0.303141259068212,
-1.68332504372461));
#29297=CARTESIAN_POINT('Ctrl Pts',(0.341837165343982,-0.236152929235937,
-1.67246562047521));
#29298=CARTESIAN_POINT('Ctrl Pts',(0.368536561654407,-0.192480977588835,
-1.66658649961961));
#29299=CARTESIAN_POINT('Ctrl Pts',(0.394174530911059,-0.123823518623745,
-1.66063136041479));
#29300=CARTESIAN_POINT('Ctrl Pts',(0.400393769631748,-0.101649918886749,
-1.65912839404491));
#29301=CARTESIAN_POINT('Ctrl Pts',(0.404717578595296,-0.0793800000000001,
-1.65807299932179));
#29302=CARTESIAN_POINT('',(0.886256117232623,-0.07938,-1.45861320581289));
#29303=CARTESIAN_POINT('Origin',(0.,-0.07938,0.));
#29304=CARTESIAN_POINT('',(1.45861320581289,-0.07938,-0.886256117232623));
#29305=CARTESIAN_POINT('Ctrl Pts',(0.886256117232623,-0.0793800000000001,
-1.45861320581289));
#29306=CARTESIAN_POINT('Ctrl Pts',(0.890059788636852,-0.101649918886749,
-1.45630208793976));
#29307=CARTESIAN_POINT('Ctrl Pts',(0.895520212222106,-0.123823518623745,
-1.45296717977858));
#29308=CARTESIAN_POINT('Ctrl Pts',(0.917859913453974,-0.192480977588835,
-1.43904931717599));
#29309=CARTESIAN_POINT('Ctrl Pts',(0.940896403863072,-0.236152929235937,
-1.4243271592157));
#29310=CARTESIAN_POINT('Ctrl Pts',(0.990027513266106,-0.303141259068211,
-1.39055359345152));
#29311=CARTESIAN_POINT('Ctrl Pts',(1.02199477007745,-0.335108247315849,
-1.36743459453896));
#29312=CARTESIAN_POINT('Ctrl Pts',(1.07446535104584,-0.373243761060364,
-1.32643091652006));
#29313=CARTESIAN_POINT('Ctrl Pts',(1.10126842659597,-0.387888272594439,
-1.30441816675528));
#29314=CARTESIAN_POINT('Ctrl Pts',(1.15530234155453,-0.407041111792943,
-1.25681160160691));
#29315=CARTESIAN_POINT('Ctrl Pts',(1.18251418313119,-0.411552957311693,
-1.23119764287622));
#29316=CARTESIAN_POINT('Ctrl Pts',(1.23119764287622,-0.411552957311693,
-1.18251418313119));
#29317=CARTESIAN_POINT('Ctrl Pts',(1.25681160160691,-0.407041111792943,
-1.15530234155453));
#29318=CARTESIAN_POINT('Ctrl Pts',(1.30441816675528,-0.387888272594439,
-1.10126842659597));
#29319=CARTESIAN_POINT('Ctrl Pts',(1.32643091652006,-0.373243761060364,
-1.07446535104584));
#29320=CARTESIAN_POINT('Ctrl Pts',(1.36743459453896,-0.335108247315849,
-1.02199477007745));
#29321=CARTESIAN_POINT('Ctrl Pts',(1.39055359345152,-0.303141259068212,
-0.990027513266105));
#29322=CARTESIAN_POINT('Ctrl Pts',(1.4243271592157,-0.236152929235937,-0.940896403863071));
#29323=CARTESIAN_POINT('Ctrl Pts',(1.43904931717599,-0.192480977588835,
-0.917859913453974));
#29324=CARTESIAN_POINT('Ctrl Pts',(1.45296717977858,-0.123823518623745,
-0.895520212222106));
#29325=CARTESIAN_POINT('Ctrl Pts',(1.45630208793976,-0.101649918886749,
-0.890059788636852));
#29326=CARTESIAN_POINT('Ctrl Pts',(1.45861320581289,-0.0793800000000001,
-0.886256117232623));
#29327=CARTESIAN_POINT('',(1.65807299932179,-0.07938,-0.404717578595296));
#29328=CARTESIAN_POINT('Origin',(0.,-0.07938,0.));
#29329=CARTESIAN_POINT('',(1.65807299932179,-0.07938,0.404717578595296));
#29330=CARTESIAN_POINT('Ctrl Pts',(1.65807299932179,-0.0793800000000001,
-0.404717578595296));
#29331=CARTESIAN_POINT('Ctrl Pts',(1.65912839404491,-0.101649918886749,
-0.400393769631747));
#29332=CARTESIAN_POINT('Ctrl Pts',(1.66063136041479,-0.123823518623745,
-0.394174530911058));
#29333=CARTESIAN_POINT('Ctrl Pts',(1.66658649961961,-0.192480977588835,
-0.368536561654407));
#29334=CARTESIAN_POINT('Ctrl Pts',(1.67246562047521,-0.236152929235937,
-0.341837165343982));
#29335=CARTESIAN_POINT('Ctrl Pts',(1.68332504372461,-0.303141259068212,
-0.283214707341173));
#29336=CARTESIAN_POINT('Ctrl Pts',(1.68958170688653,-0.335108247315849,
-0.244262842368623));
#29337=CARTESIAN_POINT('Ctrl Pts',(1.69769003172132,-0.373243761060364,
-0.178166559972324));
#29338=CARTESIAN_POINT('Ctrl Pts',(1.70107730356824,-0.387888272594439,
-0.143648558862931));
#29339=CARTESIAN_POINT('Ctrl Pts',(1.70562212620408,-0.407041111792943,
-0.0717778861362655));
#29340=CARTESIAN_POINT('Ctrl Pts',(1.706752,-0.411552957311693,-0.0344244045173312));
#29341=CARTESIAN_POINT('Ctrl Pts',(1.706752,-0.411552957311693,0.0344244045173312));
#29342=CARTESIAN_POINT('Ctrl Pts',(1.70562212620408,-0.407041111792943,
0.0717778861362655));
#29343=CARTESIAN_POINT('Ctrl Pts',(1.70107730356824,-0.387888272594439,
0.143648558862931));
#29344=CARTESIAN_POINT('Ctrl Pts',(1.69769003172132,-0.373243761060364,
0.178166559972324));
#29345=CARTESIAN_POINT('Ctrl Pts',(1.68958170688653,-0.335108247315849,
0.244262842368623));
#29346=CARTESIAN_POINT('Ctrl Pts',(1.68332504372461,-0.303141259068212,
0.283214707341173));
#29347=CARTESIAN_POINT('Ctrl Pts',(1.67246562047521,-0.236152929235937,
0.341837165343982));
#29348=CARTESIAN_POINT('Ctrl Pts',(1.66658649961961,-0.192480977588835,
0.368536561654407));
#29349=CARTESIAN_POINT('Ctrl Pts',(1.66063136041479,-0.123823518623745,
0.394174530911058));
#29350=CARTESIAN_POINT('Ctrl Pts',(1.65912839404491,-0.101649918886749,
0.400393769631747));
#29351=CARTESIAN_POINT('Ctrl Pts',(1.65807299932179,-0.0793800000000001,
0.404717578595296));
#29352=CARTESIAN_POINT('Origin',(0.,-0.07938,0.));
#29353=CARTESIAN_POINT('Origin',(0.,-0.07938,0.));
#29354=CARTESIAN_POINT('',(0.397005914195118,-0.07938,1.59456899932179));
#29355=CARTESIAN_POINT('Origin',(0.,-0.07938,0.));
#29356=CARTESIAN_POINT('Origin',(-3.33066907387547E-16,-0.07938,1.675));
#29357=CARTESIAN_POINT('Origin',(-3.33066907387547E-16,0.,1.675));
#29358=CARTESIAN_POINT('',(-0.397005914195118,-0.07938,1.59456899932179));
#29359=CARTESIAN_POINT('Ctrl Pts',(-0.397005914195119,-0.0793800000000001,
1.59456899932179));
#29360=CARTESIAN_POINT('Ctrl Pts',(-0.3886265584581,-0.123401821157026,
1.59665523941937));
#29361=CARTESIAN_POINT('Ctrl Pts',(-0.373030350867485,-0.166543350814306,
1.60050712143809));
#29362=CARTESIAN_POINT('Ctrl Pts',(-0.333298652394954,-0.237231147975234,
1.60919314384089));
#29363=CARTESIAN_POINT('Ctrl Pts',(-0.311480544243687,-0.266264900654909,
1.61365775139403));
#29364=CARTESIAN_POINT('Ctrl Pts',(-0.261368388670537,-0.317195968905306,
1.62252828437015));
#29365=CARTESIAN_POINT('Ctrl Pts',(-0.233069203882014,-0.33909093068465,
1.62691869420078));
#29366=CARTESIAN_POINT('Ctrl Pts',(-0.174042761838764,-0.373586846396559,
1.63426473152765));
#29367=CARTESIAN_POINT('Ctrl Pts',(-0.14036578147155,-0.388086240756494,
1.63761964365402));
#29368=CARTESIAN_POINT('Ctrl Pts',(-0.0701778381840615,-0.407068917407805,
1.64212536811722));
#29369=CARTESIAN_POINT('Ctrl Pts',(-0.0336652739555918,-0.411552957311693,
1.643248));
#29370=CARTESIAN_POINT('Ctrl Pts',(0.0336652739555913,-0.411552957311693,
1.643248));
#29371=CARTESIAN_POINT('Ctrl Pts',(0.070177838184061,-0.407068917407805,
1.64212536811722));
#29372=CARTESIAN_POINT('Ctrl Pts',(0.140365781471549,-0.388086240756494,
1.63761964365402));
#29373=CARTESIAN_POINT('Ctrl Pts',(0.174042761838763,-0.373586846396559,
1.63426473152765));
#29374=CARTESIAN_POINT('Ctrl Pts',(0.233069203882014,-0.33909093068465,
1.62691869420078));
#29375=CARTESIAN_POINT('Ctrl Pts',(0.261368388670536,-0.317195968905306,
1.62252828437015));
#29376=CARTESIAN_POINT('Ctrl Pts',(0.311480544243686,-0.266264900654908,
1.61365775139403));
#29377=CARTESIAN_POINT('Ctrl Pts',(0.333298652394954,-0.237231147975234,
1.60919314384089));
#29378=CARTESIAN_POINT('Ctrl Pts',(0.373030350867484,-0.166543350814306,
1.60050712143809));
#29379=CARTESIAN_POINT('Ctrl Pts',(0.388626558458099,-0.123401821157026,
1.59665523941937));
#29380=CARTESIAN_POINT('Ctrl Pts',(0.397005914195118,-0.07938,1.59456899932179));
#29381=CARTESIAN_POINT('Origin',(-3.33066907387547E-16,-0.07938,1.675));
#29382=CARTESIAN_POINT('Origin',(0.,-0.07938,0.));
#29383=CARTESIAN_POINT('',(-0.846804978391754,-0.07938,1.40825612658882));
#29384=CARTESIAN_POINT('Origin',(0.,-0.07938,0.));
#29385=CARTESIAN_POINT('Origin',(-1.18440385848747,-0.07938,1.18440385848747));
#29386=CARTESIAN_POINT('Origin',(-1.18440385848747,0.,1.18440385848747));
#29387=CARTESIAN_POINT('',(-1.40825612658882,-0.07938,0.846804978391753));
#29388=CARTESIAN_POINT('Ctrl Pts',(-1.40825612658882,-0.0793800000000001,
0.846804978391753));
#29389=CARTESIAN_POINT('Ctrl Pts',(-1.40380622184538,-0.123401821157026,
0.854205272175555));
#29390=CARTESIAN_POINT('Ctrl Pts',(-1.39550172959303,-0.166543350814306,
0.867957148219442));
#29391=CARTESIAN_POINT('Ctrl Pts',(-1.3735491215176,-0.237231147975235,
0.902193646979983));
#29392=CARTESIAN_POINT('Ctrl Pts',(-1.36127834356734,-0.266264900654909,
0.920778333482565));
#29393=CARTESIAN_POINT('Ctrl Pts',(-1.33211611256184,-0.317195968905306,
0.962485392528369));
#29394=CARTESIAN_POINT('Ctrl Pts',(-1.31521005565926,-0.339090930684651,
0.985600426557816));
#29395=CARTESIAN_POINT('Ctrl Pts',(-1.27866649102984,-0.373586846396559,
1.03253285680459));
#29396=CARTESIAN_POINT('Ctrl Pts',(-1.25722555095714,-0.388086240756494,
1.05871835910697));
#29397=CARTESIAN_POINT('Ctrl Pts',(-1.2107812086231,-0.407068917407805,
1.11153475808518));
#29398=CARTESIAN_POINT('Ctrl Pts',(-1.18575674747573,-0.411552957311693,
1.13814686046673));
#29399=CARTESIAN_POINT('Ctrl Pts',(-1.13814686046673,-0.411552957311693,
1.18575674747573));
#29400=CARTESIAN_POINT('Ctrl Pts',(-1.11153475808518,-0.407068917407805,
1.2107812086231));
#29401=CARTESIAN_POINT('Ctrl Pts',(-1.05871835910697,-0.388086240756494,
1.25722555095714));
#29402=CARTESIAN_POINT('Ctrl Pts',(-1.03253285680459,-0.373586846396559,
1.27866649102984));
#29403=CARTESIAN_POINT('Ctrl Pts',(-0.985600426557816,-0.33909093068465,
1.31521005565926));
#29404=CARTESIAN_POINT('Ctrl Pts',(-0.962485392528369,-0.317195968905306,
1.33211611256184));
#29405=CARTESIAN_POINT('Ctrl Pts',(-0.920778333482565,-0.266264900654908,
1.36127834356734));
#29406=CARTESIAN_POINT('Ctrl Pts',(-0.902193646979983,-0.237231147975234,
1.3735491215176));
#29407=CARTESIAN_POINT('Ctrl Pts',(-0.867957148219442,-0.166543350814306,
1.39550172959303));
#29408=CARTESIAN_POINT('Ctrl Pts',(-0.854205272175555,-0.123401821157026,
1.40380622184538));
#29409=CARTESIAN_POINT('Ctrl Pts',(-0.846804978391753,-0.0793800000000001,
1.40825612658882));
#29410=CARTESIAN_POINT('Origin',(-1.18440385848747,-0.07938,1.18440385848747));
#29411=CARTESIAN_POINT('Origin',(0.,-0.07938,0.));
#29412=CARTESIAN_POINT('',(-1.59456899932179,-0.07938,0.397005914195118));
#29413=CARTESIAN_POINT('Origin',(0.,-0.07938,0.));
#29414=CARTESIAN_POINT('Origin',(-1.675,-0.07938,-2.22044604925031E-16));
#29415=CARTESIAN_POINT('Origin',(-1.675,0.,-2.22044604925031E-16));
#29416=CARTESIAN_POINT('',(-1.59456899932179,-0.07938,-0.397005914195118));
#29417=CARTESIAN_POINT('',(-1.643248,-0.411552957311693,3.47540551556327E-18));
#29418=CARTESIAN_POINT('Ctrl Pts',(-1.59456899932179,-0.0793800000000001,
-0.397005914195119));
#29419=CARTESIAN_POINT('Ctrl Pts',(-1.59665523941937,-0.123401821157026,
-0.388626558458099));
#29420=CARTESIAN_POINT('Ctrl Pts',(-1.60050712143809,-0.166543350814306,
-0.373030350867485));
#29421=CARTESIAN_POINT('Ctrl Pts',(-1.60919314384089,-0.237231147975234,
-0.333298652394954));
#29422=CARTESIAN_POINT('Ctrl Pts',(-1.61365775139403,-0.266264900654909,
-0.311480544243686));
#29423=CARTESIAN_POINT('Ctrl Pts',(-1.62252828437015,-0.317195968905306,
-0.261368388670537));
#29424=CARTESIAN_POINT('Ctrl Pts',(-1.62691869420078,-0.33909093068465,
-0.233069203882014));
#29425=CARTESIAN_POINT('Ctrl Pts',(-1.63426473152765,-0.373586846396559,
-0.174042761838764));
#29426=CARTESIAN_POINT('Ctrl Pts',(-1.63761964365402,-0.388086240756494,
-0.140365781471549));
#29427=CARTESIAN_POINT('Ctrl Pts',(-1.64212536811722,-0.407068917407805,
-0.0701778381840614));
#29428=CARTESIAN_POINT('Ctrl Pts',(-1.643248,-0.411552957311693,-0.0336652739555917));
#29429=CARTESIAN_POINT('Ctrl Pts',(-1.643248,-0.411552957311693,-2.0122792321331E-16));
#29430=CARTESIAN_POINT('Origin',(-1.675,-0.07938,-2.22044604925031E-16));
#29431=CARTESIAN_POINT('Ctrl Pts',(-1.643248,-0.411552957311693,-1.94289029309402E-16));
#29432=CARTESIAN_POINT('Ctrl Pts',(-1.643248,-0.411552957311693,0.0336652739555913));
#29433=CARTESIAN_POINT('Ctrl Pts',(-1.64212536811722,-0.407068917407805,
0.0701778381840609));
#29434=CARTESIAN_POINT('Ctrl Pts',(-1.63761964365402,-0.388086240756494,
0.140365781471549));
#29435=CARTESIAN_POINT('Ctrl Pts',(-1.63426473152765,-0.373586846396559,
0.174042761838763));
#29436=CARTESIAN_POINT('Ctrl Pts',(-1.62691869420078,-0.33909093068465,
0.233069203882014));
#29437=CARTESIAN_POINT('Ctrl Pts',(-1.62252828437015,-0.317195968905306,
0.261368388670536));
#29438=CARTESIAN_POINT('Ctrl Pts',(-1.61365775139403,-0.266264900654909,
0.311480544243686));
#29439=CARTESIAN_POINT('Ctrl Pts',(-1.60919314384089,-0.237231147975235,
0.333298652394954));
#29440=CARTESIAN_POINT('Ctrl Pts',(-1.60050712143809,-0.166543350814306,
0.373030350867484));
#29441=CARTESIAN_POINT('Ctrl Pts',(-1.59665523941937,-0.123401821157026,
0.388626558458099));
#29442=CARTESIAN_POINT('Ctrl Pts',(-1.59456899932179,-0.0793800000000001,
0.397005914195118));
#29443=CARTESIAN_POINT('Origin',(0.,-0.07938,0.));
#29444=CARTESIAN_POINT('',(-1.40825612658882,-0.07938,-0.846804978391753));
#29445=CARTESIAN_POINT('Origin',(0.,-0.07938,0.));
#29446=CARTESIAN_POINT('Origin',(-1.18440385848747,-0.07938,-1.18440385848747));
#29447=CARTESIAN_POINT('Origin',(-1.18440385848747,0.,-1.18440385848747));
#29448=CARTESIAN_POINT('',(-0.846804978391753,-0.07938,-1.40825612658882));
#29449=CARTESIAN_POINT('Ctrl Pts',(-0.846804978391753,-0.0793800000000001,
-1.40825612658882));
#29450=CARTESIAN_POINT('Ctrl Pts',(-0.854205272175555,-0.123401821157026,
-1.40380622184538));
#29451=CARTESIAN_POINT('Ctrl Pts',(-0.867957148219442,-0.166543350814306,
-1.39550172959303));
#29452=CARTESIAN_POINT('Ctrl Pts',(-0.902193646979982,-0.237231147975234,
-1.3735491215176));
#29453=CARTESIAN_POINT('Ctrl Pts',(-0.920778333482564,-0.266264900654908,
-1.36127834356734));
#29454=CARTESIAN_POINT('Ctrl Pts',(-0.962485392528368,-0.317195968905306,
-1.33211611256184));
#29455=CARTESIAN_POINT('Ctrl Pts',(-0.985600426557816,-0.33909093068465,
-1.31521005565926));
#29456=CARTESIAN_POINT('Ctrl Pts',(-1.03253285680459,-0.373586846396559,
-1.27866649102984));
#29457=CARTESIAN_POINT('Ctrl Pts',(-1.05871835910697,-0.388086240756494,
-1.25722555095714));
#29458=CARTESIAN_POINT('Ctrl Pts',(-1.11153475808518,-0.407068917407805,
-1.2107812086231));
#29459=CARTESIAN_POINT('Ctrl Pts',(-1.13814686046673,-0.411552957311693,
-1.18575674747573));
#29460=CARTESIAN_POINT('Ctrl Pts',(-1.18575674747573,-0.411552957311693,
-1.13814686046673));
#29461=CARTESIAN_POINT('Ctrl Pts',(-1.2107812086231,-0.407068917407805,
-1.11153475808518));
#29462=CARTESIAN_POINT('Ctrl Pts',(-1.25722555095714,-0.388086240756494,
-1.05871835910697));
#29463=CARTESIAN_POINT('Ctrl Pts',(-1.27866649102984,-0.373586846396559,
-1.03253285680459));
#29464=CARTESIAN_POINT('Ctrl Pts',(-1.31521005565926,-0.33909093068465,
-0.985600426557816));
#29465=CARTESIAN_POINT('Ctrl Pts',(-1.33211611256184,-0.317195968905306,
-0.962485392528369));
#29466=CARTESIAN_POINT('Ctrl Pts',(-1.36127834356734,-0.266264900654909,
-0.920778333482565));
#29467=CARTESIAN_POINT('Ctrl Pts',(-1.3735491215176,-0.237231147975234,
-0.902193646979983));
#29468=CARTESIAN_POINT('Ctrl Pts',(-1.39550172959303,-0.166543350814306,
-0.867957148219442));
#29469=CARTESIAN_POINT('Ctrl Pts',(-1.40380622184538,-0.123401821157026,
-0.854205272175555));
#29470=CARTESIAN_POINT('Ctrl Pts',(-1.40825612658882,-0.07938,-0.846804978391753));
#29471=CARTESIAN_POINT('Origin',(-1.18440385848747,-0.07938,-1.18440385848747));
#29472=CARTESIAN_POINT('Origin',(0.,-0.07938,0.));
#29473=CARTESIAN_POINT('',(-0.397005914195118,-0.07938,-1.59456899932179));
#29474=CARTESIAN_POINT('Origin',(0.,-0.07938,0.));
#29475=CARTESIAN_POINT('Origin',(1.11022302462516E-16,-0.07938,-1.675));
#29476=CARTESIAN_POINT('Origin',(1.11022302462516E-16,0.,-1.675));
#29477=CARTESIAN_POINT('',(0.397005914195118,-0.07938,-1.59456899932179));
#29478=CARTESIAN_POINT('Ctrl Pts',(0.397005914195119,-0.0793800000000001,
-1.59456899932179));
#29479=CARTESIAN_POINT('Ctrl Pts',(0.388626558458099,-0.123401821157026,
-1.59665523941937));
#29480=CARTESIAN_POINT('Ctrl Pts',(0.373030350867485,-0.166543350814306,
-1.60050712143809));
#29481=CARTESIAN_POINT('Ctrl Pts',(0.333298652394954,-0.237231147975234,
-1.60919314384089));
#29482=CARTESIAN_POINT('Ctrl Pts',(0.311480544243686,-0.266264900654909,
-1.61365775139403));
#29483=CARTESIAN_POINT('Ctrl Pts',(0.261368388670537,-0.317195968905306,
-1.62252828437015));
#29484=CARTESIAN_POINT('Ctrl Pts',(0.233069203882014,-0.33909093068465,
-1.62691869420078));
#29485=CARTESIAN_POINT('Ctrl Pts',(0.174042761838763,-0.373586846396559,
-1.63426473152765));
#29486=CARTESIAN_POINT('Ctrl Pts',(0.140365781471549,-0.388086240756494,
-1.63761964365402));
#29487=CARTESIAN_POINT('Ctrl Pts',(0.0701778381840612,-0.407068917407805,
-1.64212536811722));
#29488=CARTESIAN_POINT('Ctrl Pts',(0.0336652739555916,-0.411552957311693,
-1.643248));
#29489=CARTESIAN_POINT('Ctrl Pts',(-0.0336652739555915,-0.411552957311693,
-1.643248));
#29490=CARTESIAN_POINT('Ctrl Pts',(-0.0701778381840612,-0.407068917407805,
-1.64212536811722));
#29491=CARTESIAN_POINT('Ctrl Pts',(-0.140365781471549,-0.388086240756494,
-1.63761964365402));
#29492=CARTESIAN_POINT('Ctrl Pts',(-0.174042761838764,-0.373586846396559,
-1.63426473152765));
#29493=CARTESIAN_POINT('Ctrl Pts',(-0.233069203882014,-0.33909093068465,
-1.62691869420078));
#29494=CARTESIAN_POINT('Ctrl Pts',(-0.261368388670536,-0.317195968905306,
-1.62252828437015));
#29495=CARTESIAN_POINT('Ctrl Pts',(-0.311480544243686,-0.266264900654908,
-1.61365775139403));
#29496=CARTESIAN_POINT('Ctrl Pts',(-0.333298652394954,-0.237231147975234,
-1.60919314384089));
#29497=CARTESIAN_POINT('Ctrl Pts',(-0.373030350867485,-0.166543350814306,
-1.60050712143809));
#29498=CARTESIAN_POINT('Ctrl Pts',(-0.388626558458099,-0.123401821157026,
-1.59665523941937));
#29499=CARTESIAN_POINT('Ctrl Pts',(-0.397005914195118,-0.07938,-1.59456899932179));
#29500=CARTESIAN_POINT('Origin',(1.11022302462516E-16,-0.07938,-1.675));
#29501=CARTESIAN_POINT('Origin',(0.,-0.07938,0.));
#29502=CARTESIAN_POINT('',(0.846804978391753,-0.07938,-1.40825612658882));
#29503=CARTESIAN_POINT('Origin',(0.,-0.07938,0.));
#29504=CARTESIAN_POINT('Origin',(1.18440385848747,-0.07938,-1.18440385848747));
#29505=CARTESIAN_POINT('Origin',(1.18440385848747,0.,-1.18440385848747));
#29506=CARTESIAN_POINT('',(1.40825612658882,-0.07938,-0.846804978391753));
#29507=CARTESIAN_POINT('Ctrl Pts',(1.40825612658882,-0.0793800000000001,
-0.846804978391753));
#29508=CARTESIAN_POINT('Ctrl Pts',(1.40380622184538,-0.123401821157026,
-0.854205272175555));
#29509=CARTESIAN_POINT('Ctrl Pts',(1.39550172959303,-0.166543350814306,
-0.867957148219442));
#29510=CARTESIAN_POINT('Ctrl Pts',(1.3735491215176,-0.237231147975234,-0.902193646979983));
#29511=CARTESIAN_POINT('Ctrl Pts',(1.36127834356734,-0.266264900654908,
-0.920778333482565));
#29512=CARTESIAN_POINT('Ctrl Pts',(1.33211611256184,-0.317195968905306,
-0.962485392528369));
#29513=CARTESIAN_POINT('Ctrl Pts',(1.31521005565926,-0.33909093068465,-0.985600426557816));
#29514=CARTESIAN_POINT('Ctrl Pts',(1.27866649102984,-0.373586846396559,
-1.03253285680459));
#29515=CARTESIAN_POINT('Ctrl Pts',(1.25722555095714,-0.388086240756494,
-1.05871835910697));
#29516=CARTESIAN_POINT('Ctrl Pts',(1.2107812086231,-0.407068917407805,-1.11153475808518));
#29517=CARTESIAN_POINT('Ctrl Pts',(1.18575674747573,-0.411552957311693,
-1.13814686046673));
#29518=CARTESIAN_POINT('Ctrl Pts',(1.13814686046673,-0.411552957311693,
-1.18575674747573));
#29519=CARTESIAN_POINT('Ctrl Pts',(1.11153475808518,-0.407068917407805,
-1.2107812086231));
#29520=CARTESIAN_POINT('Ctrl Pts',(1.05871835910697,-0.388086240756494,
-1.25722555095714));
#29521=CARTESIAN_POINT('Ctrl Pts',(1.03253285680459,-0.373586846396559,
-1.27866649102984));
#29522=CARTESIAN_POINT('Ctrl Pts',(0.985600426557816,-0.33909093068465,
-1.31521005565926));
#29523=CARTESIAN_POINT('Ctrl Pts',(0.962485392528369,-0.317195968905306,
-1.33211611256184));
#29524=CARTESIAN_POINT('Ctrl Pts',(0.920778333482565,-0.266264900654909,
-1.36127834356734));
#29525=CARTESIAN_POINT('Ctrl Pts',(0.902193646979983,-0.237231147975234,
-1.3735491215176));
#29526=CARTESIAN_POINT('Ctrl Pts',(0.867957148219442,-0.166543350814306,
-1.39550172959303));
#29527=CARTESIAN_POINT('Ctrl Pts',(0.854205272175555,-0.123401821157026,
-1.40380622184538));
#29528=CARTESIAN_POINT('Ctrl Pts',(0.846804978391753,-0.0793800000000001,
-1.40825612658882));
#29529=CARTESIAN_POINT('Origin',(1.18440385848747,-0.07938,-1.18440385848747));
#29530=CARTESIAN_POINT('Origin',(0.,-0.27783,0.));
#29531=CARTESIAN_POINT('',(-1.643248,-0.47628,2.01239840340529E-16));
#29532=CARTESIAN_POINT('Origin',(0.,-0.47628,0.));
#29533=CARTESIAN_POINT('',(-1.643248,-0.27783,2.01239840340529E-16));
#29534=CARTESIAN_POINT('',(1.59456899932179,-0.07938,0.397005914195118));
#29535=CARTESIAN_POINT('Origin',(0.,-0.07938,0.));
#29536=CARTESIAN_POINT('',(1.59456899932179,-0.07938,-0.397005914195118));
#29537=CARTESIAN_POINT('Ctrl Pts',(1.59456899932179,-0.0793800000000001,
0.397005914195118));
#29538=CARTESIAN_POINT('Ctrl Pts',(1.59665523941937,-0.123401821157026,
0.388626558458099));
#29539=CARTESIAN_POINT('Ctrl Pts',(1.60050712143809,-0.166543350814306,
0.373030350867485));
#29540=CARTESIAN_POINT('Ctrl Pts',(1.60919314384089,-0.237231147975234,
0.333298652394954));
#29541=CARTESIAN_POINT('Ctrl Pts',(1.61365775139403,-0.266264900654909,
0.311480544243686));
#29542=CARTESIAN_POINT('Ctrl Pts',(1.62252828437015,-0.317195968905306,
0.261368388670537));
#29543=CARTESIAN_POINT('Ctrl Pts',(1.62691869420078,-0.33909093068465,0.233069203882014));
#29544=CARTESIAN_POINT('Ctrl Pts',(1.63426473152765,-0.373586846396559,
0.174042761838764));
#29545=CARTESIAN_POINT('Ctrl Pts',(1.63761964365402,-0.388086240756494,
0.140365781471549));
#29546=CARTESIAN_POINT('Ctrl Pts',(1.64212536811722,-0.407068917407805,
0.0701778381840612));
#29547=CARTESIAN_POINT('Ctrl Pts',(1.643248,-0.411552957311693,0.0336652739555916));
#29548=CARTESIAN_POINT('Ctrl Pts',(1.643248,-0.411552957311693,-0.0336652739555916));
#29549=CARTESIAN_POINT('Ctrl Pts',(1.64212536811722,-0.407068917407805,
-0.0701778381840612));
#29550=CARTESIAN_POINT('Ctrl Pts',(1.63761964365402,-0.388086240756494,
-0.140365781471549));
#29551=CARTESIAN_POINT('Ctrl Pts',(1.63426473152765,-0.373586846396559,
-0.174042761838764));
#29552=CARTESIAN_POINT('Ctrl Pts',(1.62691869420078,-0.33909093068465,-0.233069203882014));
#29553=CARTESIAN_POINT('Ctrl Pts',(1.62252828437015,-0.317195968905306,
-0.261368388670537));
#29554=CARTESIAN_POINT('Ctrl Pts',(1.61365775139403,-0.266264900654909,
-0.311480544243686));
#29555=CARTESIAN_POINT('Ctrl Pts',(1.60919314384089,-0.237231147975234,
-0.333298652394954));
#29556=CARTESIAN_POINT('Ctrl Pts',(1.60050712143809,-0.166543350814306,
-0.373030350867485));
#29557=CARTESIAN_POINT('Ctrl Pts',(1.59665523941937,-0.123401821157026,
-0.388626558458099));
#29558=CARTESIAN_POINT('Ctrl Pts',(1.59456899932179,-0.07938,-0.397005914195118));
#29559=CARTESIAN_POINT('Origin',(0.,-0.07938,0.));
#29560=CARTESIAN_POINT('Origin',(0.,-0.07938,0.));
#29561=CARTESIAN_POINT('Origin',(1.675,-0.07938,0.));
#29562=CARTESIAN_POINT('Origin',(1.675,0.,0.));
#29563=CARTESIAN_POINT('Origin',(1.675,-0.07938,0.));
#29564=CARTESIAN_POINT('Origin',(0.,-0.47628,0.));
#29565=CARTESIAN_POINT('Origin',(0.,-0.07938,0.));
#29566=CARTESIAN_POINT('',(0.,0.,0.));
#29567=CARTESIAN_POINT('Origin',(1.70469,0.695,0.));
#29568=CARTESIAN_POINT('',(-1.70469,0.695,-2.0876431520385E-16));
#29569=CARTESIAN_POINT('Origin',(0.,0.695,0.));
#29570=CARTESIAN_POINT('',(-1.65031,0.695,-2.02104685910087E-16));
#29571=CARTESIAN_POINT('Origin',(0.,0.695,0.));
#29572=CARTESIAN_POINT('Origin',(0.,0.6575,0.));
#29573=CARTESIAN_POINT('',(-1.70469,0.62,-2.0876431520385E-16));
#29574=CARTESIAN_POINT('Origin',(0.,0.62,0.));
#29575=CARTESIAN_POINT('',(-1.70469,0.6575,-2.0876431520385E-16));
#29576=CARTESIAN_POINT('Origin',(1.65031,0.62,0.));
#29577=CARTESIAN_POINT('',(-1.65031,0.62,-2.02104685910087E-16));
#29578=CARTESIAN_POINT('Origin',(0.,0.62,0.));
#29579=CARTESIAN_POINT('Origin',(0.,0.6575,0.));
#29580=CARTESIAN_POINT('',(-1.65031,0.6575,-2.02104685910087E-16));
#29581=CARTESIAN_POINT('Origin',(1.70469,-0.62,0.));
#29582=CARTESIAN_POINT('',(-1.70469,-0.62,-2.0876431520385E-16));
#29583=CARTESIAN_POINT('Origin',(0.,-0.62,0.));
#29584=CARTESIAN_POINT('',(-1.65031,-0.62,-2.02104685910087E-16));
#29585=CARTESIAN_POINT('Origin',(0.,-0.62,0.));
#29586=CARTESIAN_POINT('Origin',(0.,-0.6575,0.));
#29587=CARTESIAN_POINT('',(-1.70469,-0.695,-2.0876431520385E-16));
#29588=CARTESIAN_POINT('Origin',(0.,-0.695,0.));
#29589=CARTESIAN_POINT('',(-1.70469,-0.6575,-2.0876431520385E-16));
#29590=CARTESIAN_POINT('Origin',(1.65031,-0.695,0.));
#29591=CARTESIAN_POINT('',(-1.65031,-0.695,-2.02104685910087E-16));
#29592=CARTESIAN_POINT('Origin',(0.,-0.695,0.));
#29593=CARTESIAN_POINT('Origin',(0.,-0.6575,0.));
#29594=CARTESIAN_POINT('',(-1.65031,-0.6575,-2.02104685910087E-16));
#29595=CARTESIAN_POINT('',(0.,0.,0.));
#29596=CARTESIAN_POINT('',(0.,0.,0.));
#29597=CARTESIAN_POINT('',(0.,0.,0.));
#29598=CARTESIAN_POINT('',(0.,0.,0.));
#29599=CARTESIAN_POINT('',(0.,0.,0.));
#29600=CARTESIAN_POINT('',(0.,0.,0.));
#29601=CARTESIAN_POINT('Origin',(0.,-2.5,0.));
#29602=CARTESIAN_POINT('',(-0.25,-2.5,3.06161699786838E-17));
#29603=CARTESIAN_POINT('Origin',(0.,-2.5,0.));
#29604=CARTESIAN_POINT('Origin',(0.,-1.9,0.));
#29605=CARTESIAN_POINT('',(-0.25,-1.9,3.06161699786838E-17));
#29606=CARTESIAN_POINT('Origin',(0.,-1.9,0.));
#29607=CARTESIAN_POINT('',(-0.24505,-1.9,3.00099698131059E-17));
#29608=CARTESIAN_POINT('Origin',(0.,-1.9,0.));
#29609=CARTESIAN_POINT('Origin',(0.,-3.,0.));
#29610=CARTESIAN_POINT('',(-0.25,-3.,3.06161699786838E-17));
#29611=CARTESIAN_POINT('Origin',(0.375,0.5,0.));
#29612=CARTESIAN_POINT('',(-0.375,0.5,-4.59242549680257E-17));
#29613=CARTESIAN_POINT('Origin',(0.,0.5,0.));
#29614=CARTESIAN_POINT('Origin',(0.,0.475,0.));
#29615=CARTESIAN_POINT('',(-0.425,0.45,-5.20474889637625E-17));
#29616=CARTESIAN_POINT('Origin',(0.,0.45,0.));
#29617=CARTESIAN_POINT('',(-0.4,0.475,-4.89858719658941E-17));
#29618=CARTESIAN_POINT('Origin',(0.,0.24,0.));
#29619=CARTESIAN_POINT('',(-0.425,0.0299999999999998,-5.20474889637625E-17));
#29620=CARTESIAN_POINT('Origin',(0.,0.0299999999999998,0.));
#29621=CARTESIAN_POINT('',(-0.425,0.24,-5.20474889637625E-17));
#29622=CARTESIAN_POINT('Origin',(0.,0.0150000000000001,0.));
#29623=CARTESIAN_POINT('',(-0.395,4.85722573273506E-17,-4.83735485663204E-17));
#29624=CARTESIAN_POINT('Origin',(0.,0.,0.));
#29625=CARTESIAN_POINT('',(-0.41,0.0150000000000001,-5.02105187650415E-17));
#29626=CARTESIAN_POINT('Origin',(0.27,0.,0.));
#29627=CARTESIAN_POINT('',(-0.27,0.,-3.30654635769785E-17));
#29628=CARTESIAN_POINT('Origin',(0.,0.,0.));
#29629=CARTESIAN_POINT('Origin',(0.,-0.02,0.));
#29630=CARTESIAN_POINT('',(-0.24505,-0.0498999999999999,3.00099698131059E-17));
#29631=CARTESIAN_POINT('Origin',(0.,-0.0498999999999999,0.));
#29632=CARTESIAN_POINT('',(-0.26,-0.02,-3.18408167778312E-17));
#29633=CARTESIAN_POINT('Origin',(0.,-0.995,0.));
#29634=CARTESIAN_POINT('',(-0.24505,-0.995,-3.00099698131059E-17));
#29635=CARTESIAN_POINT('Origin',(0.115470053837925,-0.5,-0.2));
#29636=CARTESIAN_POINT('',(0.23094010767585,-0.5,0.));
#29637=CARTESIAN_POINT('',(0.115470053837925,-0.5,-0.2));
#29638=CARTESIAN_POINT('',(0.23094010767585,-0.5,0.));
#29639=CARTESIAN_POINT('',(0.115470053837925,-0.8,-0.2));
#29640=CARTESIAN_POINT('',(0.115470053837925,-0.5,-0.2));
#29641=CARTESIAN_POINT('',(0.23094010767585,-0.8,0.));
#29642=CARTESIAN_POINT('',(0.23094010767585,-0.8,0.));
#29643=CARTESIAN_POINT('',(0.23094010767585,-0.5,0.));
#29644=CARTESIAN_POINT('Origin',(-0.115470053837925,-0.5,-0.2));
#29645=CARTESIAN_POINT('',(-0.115470053837925,-0.5,-0.2));
#29646=CARTESIAN_POINT('',(0.115470053837925,-0.5,-0.2));
#29647=CARTESIAN_POINT('',(-0.115470053837925,-0.8,-0.2));
#29648=CARTESIAN_POINT('',(-0.115470053837925,-0.5,-0.2));
#29649=CARTESIAN_POINT('',(0.115470053837925,-0.8,-0.2));
#29650=CARTESIAN_POINT('Origin',(-0.23094010767585,-0.5,-2.77555756156289E-17));
#29651=CARTESIAN_POINT('',(-0.23094010767585,-0.5,-2.82820063659975E-17));
#29652=CARTESIAN_POINT('',(-0.115470053837925,-0.5,-0.2));
#29653=CARTESIAN_POINT('',(-0.23094010767585,-0.8,-2.77555756156289E-17));
#29654=CARTESIAN_POINT('',(-0.23094010767585,-0.5,-2.82820063659975E-17));
#29655=CARTESIAN_POINT('',(-0.115470053837925,-0.8,-0.2));
#29656=CARTESIAN_POINT('Origin',(-0.115470053837925,-0.5,0.2));
#29657=CARTESIAN_POINT('',(-0.115470053837925,-0.5,0.2));
#29658=CARTESIAN_POINT('',(-0.23094010767585,-0.5,-2.82820063659975E-17));
#29659=CARTESIAN_POINT('',(-0.115470053837925,-0.8,0.2));
#29660=CARTESIAN_POINT('',(-0.115470053837925,-0.5,0.2));
#29661=CARTESIAN_POINT('',(-0.23094010767585,-0.8,-2.82820063659975E-17));
#29662=CARTESIAN_POINT('Origin',(0.115470053837925,-0.5,0.2));
#29663=CARTESIAN_POINT('',(0.115470053837925,-0.5,0.2));
#29664=CARTESIAN_POINT('',(-0.115470053837925,-0.5,0.2));
#29665=CARTESIAN_POINT('',(0.115470053837925,-0.8,0.2));
#29666=CARTESIAN_POINT('',(0.115470053837925,-0.5,0.2));
#29667=CARTESIAN_POINT('',(-0.115470053837925,-0.8,0.2));
#29668=CARTESIAN_POINT('Origin',(0.23094010767585,-0.5,0.));
#29669=CARTESIAN_POINT('',(0.115470053837925,-0.5,0.2));
#29670=CARTESIAN_POINT('',(0.115470053837925,-0.8,0.2));
#29671=CARTESIAN_POINT('Origin',(0.,-0.5,0.));
#29672=CARTESIAN_POINT('Origin',(0.,-0.8,0.));
#29673=CARTESIAN_POINT('',(0.,0.,0.));
#29674=CARTESIAN_POINT('Origin',(0.0866025403784439,-0.4,-0.15));
#29675=CARTESIAN_POINT('',(0.173205080756888,-0.4,0.));
#29676=CARTESIAN_POINT('',(0.0866025403784439,-0.4,-0.15));
#29677=CARTESIAN_POINT('',(0.173205080756888,-0.4,0.));
#29678=CARTESIAN_POINT('',(0.0866025403784439,-0.64,-0.15));
#29679=CARTESIAN_POINT('',(0.0866025403784439,-0.4,-0.15));
#29680=CARTESIAN_POINT('',(0.173205080756888,-0.64,0.));
#29681=CARTESIAN_POINT('',(0.173205080756888,-0.64,0.));
#29682=CARTESIAN_POINT('',(0.173205080756888,-0.4,0.));
#29683=CARTESIAN_POINT('Origin',(-0.0866025403784438,-0.4,-0.15));
#29684=CARTESIAN_POINT('',(-0.0866025403784438,-0.4,-0.15));
#29685=CARTESIAN_POINT('',(0.0866025403784439,-0.4,-0.15));
#29686=CARTESIAN_POINT('',(-0.0866025403784438,-0.64,-0.15));
#29687=CARTESIAN_POINT('',(-0.0866025403784438,-0.4,-0.15));
#29688=CARTESIAN_POINT('',(0.0866025403784439,-0.64,-0.15));
#29689=CARTESIAN_POINT('Origin',(-0.173205080756888,-0.4,-2.77555756156289E-17));
#29690=CARTESIAN_POINT('',(-0.173205080756888,-0.4,-2.12115047744981E-17));
#29691=CARTESIAN_POINT('',(-0.0866025403784438,-0.4,-0.15));
#29692=CARTESIAN_POINT('',(-0.173205080756888,-0.64,-2.77555756156289E-17));
#29693=CARTESIAN_POINT('',(-0.173205080756888,-0.4,-2.12115047744981E-17));
#29694=CARTESIAN_POINT('',(-0.0866025403784438,-0.64,-0.15));
#29695=CARTESIAN_POINT('Origin',(-0.0866025403784439,-0.4,0.15));
#29696=CARTESIAN_POINT('',(-0.0866025403784439,-0.4,0.15));
#29697=CARTESIAN_POINT('',(-0.173205080756888,-0.4,-2.12115047744981E-17));
#29698=CARTESIAN_POINT('',(-0.0866025403784439,-0.64,0.15));
#29699=CARTESIAN_POINT('',(-0.0866025403784439,-0.4,0.15));
#29700=CARTESIAN_POINT('',(-0.173205080756888,-0.64,-2.12115047744981E-17));
#29701=CARTESIAN_POINT('Origin',(0.0866025403784439,-0.4,0.15));
#29702=CARTESIAN_POINT('',(0.0866025403784439,-0.4,0.15));
#29703=CARTESIAN_POINT('',(-0.0866025403784439,-0.4,0.15));
#29704=CARTESIAN_POINT('',(0.0866025403784439,-0.64,0.15));
#29705=CARTESIAN_POINT('',(0.0866025403784439,-0.4,0.15));
#29706=CARTESIAN_POINT('',(-0.0866025403784439,-0.64,0.15));
#29707=CARTESIAN_POINT('Origin',(0.173205080756888,-0.4,0.));
#29708=CARTESIAN_POINT('',(0.0866025403784439,-0.4,0.15));
#29709=CARTESIAN_POINT('',(0.0866025403784439,-0.64,0.15));
#29710=CARTESIAN_POINT('Origin',(0.,-0.4,-2.77555756156289E-17));
#29711=CARTESIAN_POINT('Origin',(0.,-0.64,-2.77555756156289E-17));
#29712=CARTESIAN_POINT('Origin',(0.,-1.,0.));
#29713=CARTESIAN_POINT('',(-0.1954,-1.,2.39295984553393E-17));
#29714=CARTESIAN_POINT('Origin',(0.,-1.,0.));
#29715=CARTESIAN_POINT('Origin',(0.3,0.4,0.));
#29716=CARTESIAN_POINT('',(-0.3,0.4,-3.67394039744206E-17));
#29717=CARTESIAN_POINT('Origin',(0.,0.4,0.));
#29718=CARTESIAN_POINT('Origin',(0.,0.375,0.));
#29719=CARTESIAN_POINT('',(-0.35,0.35,-4.28626379701573E-17));
#29720=CARTESIAN_POINT('Origin',(0.,0.35,0.));
#29721=CARTESIAN_POINT('',(-0.325,0.375,-3.9801020972289E-17));
#29722=CARTESIAN_POINT('Origin',(0.,0.19,0.));
#29723=CARTESIAN_POINT('',(-0.35,0.03,-4.28626379701574E-17));
#29724=CARTESIAN_POINT('Origin',(0.,0.03,0.));
#29725=CARTESIAN_POINT('',(-0.35,0.19,-4.28626379701574E-17));
#29726=CARTESIAN_POINT('Origin',(0.,0.0149999999999999,0.));
#29727=CARTESIAN_POINT('',(-0.32,-3.29597460435593E-17,-3.91886975727153E-17));
#29728=CARTESIAN_POINT('Origin',(0.,0.,0.));
#29729=CARTESIAN_POINT('',(-0.335,0.0149999999999999,-4.10256677714363E-17));
#29730=CARTESIAN_POINT('Origin',(0.22,0.,0.));
#29731=CARTESIAN_POINT('',(-0.22,-6.93889390390723E-18,-2.69422295812418E-17));
#29732=CARTESIAN_POINT('Origin',(0.,0.,0.));
#29733=CARTESIAN_POINT('Origin',(0.,-0.02,0.));
#29734=CARTESIAN_POINT('',(-0.1954,-0.0492,2.39295984553393E-17));
#29735=CARTESIAN_POINT('Origin',(0.,-0.0492,0.));
#29736=CARTESIAN_POINT('',(-0.21,-0.02,-2.57175827820944E-17));
#29737=CARTESIAN_POINT('Origin',(0.,-0.8,0.));
#29738=CARTESIAN_POINT('',(-0.1954,-0.8,-2.39295984553393E-17));
#29739=CARTESIAN_POINT('',(0.,0.,0.));
#29740=CARTESIAN_POINT('Origin',(-0.1,0.82,-0.3));
#29741=CARTESIAN_POINT('',(0.,0.82,-0.3));
#29742=CARTESIAN_POINT('',(0.,1.,-0.3));
#29743=CARTESIAN_POINT('',(0.,0.41,-0.3));
#29744=CARTESIAN_POINT('',(40.,0.82,-0.3));
#29745=CARTESIAN_POINT('',(-0.1,0.82,-0.3));
#29746=CARTESIAN_POINT('',(40.,1.,-0.3));
#29747=CARTESIAN_POINT('',(40.,0.41,-0.3));
#29748=CARTESIAN_POINT('',(-0.05,1.,-0.3));
#29749=CARTESIAN_POINT('Origin',(-0.1,0.82,-0.55));
#29750=CARTESIAN_POINT('',(0.,0.82,-0.55));
#29751=CARTESIAN_POINT('',(0.,0.82,-0.275));
#29752=CARTESIAN_POINT('',(40.,0.82,-0.55));
#29753=CARTESIAN_POINT('',(-0.1,0.82,-0.55));
#29754=CARTESIAN_POINT('',(40.,0.82,-0.275));
#29755=CARTESIAN_POINT('Origin',(-0.1,0.67,-0.55));
#29756=CARTESIAN_POINT('',(0.,0.67,-0.55));
#29757=CARTESIAN_POINT('',(0.,0.335,-0.55));
#29758=CARTESIAN_POINT('',(40.,0.67,-0.55));
#29759=CARTESIAN_POINT('',(-0.1,0.67,-0.55));
#29760=CARTESIAN_POINT('',(40.,0.335,-0.55));
#29761=CARTESIAN_POINT('Origin',(-0.1,0.42,-0.3));
#29762=CARTESIAN_POINT('',(0.,0.42,-0.3));
#29763=CARTESIAN_POINT('',(0.,0.24,-0.12));
#29764=CARTESIAN_POINT('',(40.,0.42,-0.3));
#29765=CARTESIAN_POINT('',(-0.1,0.42,-0.3));
#29766=CARTESIAN_POINT('',(40.,0.24,-0.12));
#29767=CARTESIAN_POINT('Origin',(-0.1,0.42,0.3));
#29768=CARTESIAN_POINT('',(0.,0.42,0.3));
#29769=CARTESIAN_POINT('',(0.,0.42,0.15));
#29770=CARTESIAN_POINT('',(40.,0.42,0.3));
#29771=CARTESIAN_POINT('',(-0.1,0.42,0.3));
#29772=CARTESIAN_POINT('',(40.,0.42,0.15));
#29773=CARTESIAN_POINT('Origin',(-0.1,0.67,0.55));
#29774=CARTESIAN_POINT('',(0.,0.67,0.55));
#29775=CARTESIAN_POINT('',(6.93889390390723E-18,0.365,0.245));
#29776=CARTESIAN_POINT('',(40.,0.67,0.55));
#29777=CARTESIAN_POINT('',(-0.1,0.67,0.55));
#29778=CARTESIAN_POINT('',(40.,0.365,0.245));
#29779=CARTESIAN_POINT('Origin',(-0.1,0.82,0.55));
#29780=CARTESIAN_POINT('',(0.,0.82,0.55));
#29781=CARTESIAN_POINT('',(0.,0.41,0.55));
#29782=CARTESIAN_POINT('',(40.,0.82,0.55));
#29783=CARTESIAN_POINT('',(-0.1,0.82,0.55));
#29784=CARTESIAN_POINT('',(40.,0.41,0.55));
#29785=CARTESIAN_POINT('Origin',(-0.1,0.82,0.3));
#29786=CARTESIAN_POINT('',(0.,0.82,0.3));
#29787=CARTESIAN_POINT('',(0.,0.82,0.15));
#29788=CARTESIAN_POINT('',(40.,0.82,0.3));
#29789=CARTESIAN_POINT('',(-0.1,0.82,0.3));
#29790=CARTESIAN_POINT('',(40.,0.82,0.15));
#29791=CARTESIAN_POINT('Origin',(-0.1,1.05,0.3));
#29792=CARTESIAN_POINT('',(0.,1.,0.3));
#29793=CARTESIAN_POINT('',(0.,0.525,0.3));
#29794=CARTESIAN_POINT('',(40.,1.,0.3));
#29795=CARTESIAN_POINT('',(-0.05,1.,0.3));
#29796=CARTESIAN_POINT('',(40.,0.525,0.3));
#29797=CARTESIAN_POINT('Origin',(-0.1,-0.3,-0.82));
#29798=CARTESIAN_POINT('',(0.,-0.3,-0.82));
#29799=CARTESIAN_POINT('',(0.,-0.3,-1.));
#29800=CARTESIAN_POINT('',(0.,-0.3,-0.41));
#29801=CARTESIAN_POINT('',(40.,-0.3,-0.82));
#29802=CARTESIAN_POINT('',(-0.1,-0.3,-0.82));
#29803=CARTESIAN_POINT('',(40.,-0.3,-1.));
#29804=CARTESIAN_POINT('',(40.,-0.3,-0.41));
#29805=CARTESIAN_POINT('',(-0.05,-0.3,-1.));
#29806=CARTESIAN_POINT('Origin',(-0.1,-0.55,-0.82));
#29807=CARTESIAN_POINT('',(0.,-0.55,-0.82));
#29808=CARTESIAN_POINT('',(0.,-0.275,-0.82));
#29809=CARTESIAN_POINT('',(40.,-0.55,-0.82));
#29810=CARTESIAN_POINT('',(-0.1,-0.55,-0.82));
#29811=CARTESIAN_POINT('',(40.,-0.275,-0.82));
#29812=CARTESIAN_POINT('Origin',(-0.1,-0.55,-0.67));
#29813=CARTESIAN_POINT('',(0.,-0.55,-0.67));
#29814=CARTESIAN_POINT('',(0.,-0.55,-0.335));
#29815=CARTESIAN_POINT('',(40.,-0.55,-0.67));
#29816=CARTESIAN_POINT('',(-0.1,-0.55,-0.67));
#29817=CARTESIAN_POINT('',(40.,-0.55,-0.335));
#29818=CARTESIAN_POINT('Origin',(-0.1,-0.3,-0.42));
#29819=CARTESIAN_POINT('',(0.,-0.3,-0.42));
#29820=CARTESIAN_POINT('',(0.,-0.12,-0.24));
#29821=CARTESIAN_POINT('',(40.,-0.3,-0.42));
#29822=CARTESIAN_POINT('',(-0.1,-0.3,-0.42));
#29823=CARTESIAN_POINT('',(40.,-0.12,-0.24));
#29824=CARTESIAN_POINT('Origin',(-0.1,0.3,-0.42));
#29825=CARTESIAN_POINT('',(0.,0.3,-0.42));
#29826=CARTESIAN_POINT('',(0.,0.15,-0.42));
#29827=CARTESIAN_POINT('',(40.,0.3,-0.42));
#29828=CARTESIAN_POINT('',(-0.1,0.3,-0.42));
#29829=CARTESIAN_POINT('',(40.,0.15,-0.42));
#29830=CARTESIAN_POINT('Origin',(-0.1,0.55,-0.67));
#29831=CARTESIAN_POINT('',(0.,0.55,-0.67));
#29832=CARTESIAN_POINT('',(0.,0.245,-0.365));
#29833=CARTESIAN_POINT('',(40.,0.55,-0.67));
#29834=CARTESIAN_POINT('',(-0.1,0.55,-0.67));
#29835=CARTESIAN_POINT('',(40.,0.245,-0.365));
#29836=CARTESIAN_POINT('Origin',(-0.1,0.55,-0.82));
#29837=CARTESIAN_POINT('',(0.,0.55,-0.82));
#29838=CARTESIAN_POINT('',(0.,0.55,-0.41));
#29839=CARTESIAN_POINT('',(40.,0.55,-0.82));
#29840=CARTESIAN_POINT('',(-0.1,0.55,-0.82));
#29841=CARTESIAN_POINT('',(40.,0.55,-0.41));
#29842=CARTESIAN_POINT('Origin',(-0.1,0.3,-0.82));
#29843=CARTESIAN_POINT('',(0.,0.3,-0.82));
#29844=CARTESIAN_POINT('',(0.,0.15,-0.82));
#29845=CARTESIAN_POINT('',(40.,0.3,-0.82));
#29846=CARTESIAN_POINT('',(-0.1,0.3,-0.82));
#29847=CARTESIAN_POINT('',(40.,0.15,-0.82));
#29848=CARTESIAN_POINT('Origin',(-0.1,0.3,-1.05));
#29849=CARTESIAN_POINT('',(0.,0.3,-1.));
#29850=CARTESIAN_POINT('',(0.,0.3,-0.525));
#29851=CARTESIAN_POINT('',(40.,0.3,-1.));
#29852=CARTESIAN_POINT('',(-0.05,0.3,-1.));
#29853=CARTESIAN_POINT('',(40.,0.3,-0.525));
#29854=CARTESIAN_POINT('Origin',(-0.1,-0.82,0.3));
#29855=CARTESIAN_POINT('',(0.,-0.82,0.3));
#29856=CARTESIAN_POINT('',(0.,-1.,0.3));
#29857=CARTESIAN_POINT('',(0.,-0.41,0.3));
#29858=CARTESIAN_POINT('',(40.,-0.82,0.3));
#29859=CARTESIAN_POINT('',(-0.1,-0.82,0.3));
#29860=CARTESIAN_POINT('',(40.,-1.,0.3));
#29861=CARTESIAN_POINT('',(40.,-0.41,0.3));
#29862=CARTESIAN_POINT('',(-0.05,-1.,0.3));
#29863=CARTESIAN_POINT('Origin',(-0.1,-0.82,0.55));
#29864=CARTESIAN_POINT('',(0.,-0.82,0.55));
#29865=CARTESIAN_POINT('',(0.,-0.82,0.275));
#29866=CARTESIAN_POINT('',(40.,-0.82,0.55));
#29867=CARTESIAN_POINT('',(-0.1,-0.82,0.55));
#29868=CARTESIAN_POINT('',(40.,-0.82,0.275));
#29869=CARTESIAN_POINT('Origin',(-0.1,-0.67,0.55));
#29870=CARTESIAN_POINT('',(0.,-0.67,0.55));
#29871=CARTESIAN_POINT('',(0.,-0.335,0.55));
#29872=CARTESIAN_POINT('',(40.,-0.67,0.55));
#29873=CARTESIAN_POINT('',(-0.1,-0.67,0.55));
#29874=CARTESIAN_POINT('',(40.,-0.335,0.55));
#29875=CARTESIAN_POINT('Origin',(-0.1,-0.42,0.3));
#29876=CARTESIAN_POINT('',(0.,-0.42,0.3));
#29877=CARTESIAN_POINT('',(-6.93889390390723E-18,-0.24,0.12));
#29878=CARTESIAN_POINT('',(40.,-0.42,0.3));
#29879=CARTESIAN_POINT('',(-0.1,-0.42,0.3));
#29880=CARTESIAN_POINT('',(40.,-0.24,0.12));
#29881=CARTESIAN_POINT('Origin',(-0.1,-0.42,-0.3));
#29882=CARTESIAN_POINT('',(0.,-0.42,-0.3));
#29883=CARTESIAN_POINT('',(0.,-0.42,-0.15));
#29884=CARTESIAN_POINT('',(40.,-0.42,-0.3));
#29885=CARTESIAN_POINT('',(-0.1,-0.42,-0.3));
#29886=CARTESIAN_POINT('',(40.,-0.42,-0.15));
#29887=CARTESIAN_POINT('Origin',(-0.1,-0.67,-0.55));
#29888=CARTESIAN_POINT('',(0.,-0.67,-0.55));
#29889=CARTESIAN_POINT('',(0.,-0.365,-0.245));
#29890=CARTESIAN_POINT('',(40.,-0.67,-0.55));
#29891=CARTESIAN_POINT('',(-0.1,-0.67,-0.55));
#29892=CARTESIAN_POINT('',(40.,-0.365,-0.245));
#29893=CARTESIAN_POINT('Origin',(-0.1,-0.82,-0.55));
#29894=CARTESIAN_POINT('',(0.,-0.82,-0.55));
#29895=CARTESIAN_POINT('',(0.,-0.41,-0.55));
#29896=CARTESIAN_POINT('',(40.,-0.82,-0.55));
#29897=CARTESIAN_POINT('',(-0.1,-0.82,-0.55));
#29898=CARTESIAN_POINT('',(40.,-0.41,-0.55));
#29899=CARTESIAN_POINT('Origin',(-0.1,-0.82,-0.3));
#29900=CARTESIAN_POINT('',(0.,-0.82,-0.3));
#29901=CARTESIAN_POINT('',(0.,-0.82,-0.15));
#29902=CARTESIAN_POINT('',(40.,-0.82,-0.3));
#29903=CARTESIAN_POINT('',(-0.1,-0.82,-0.3));
#29904=CARTESIAN_POINT('',(40.,-0.82,-0.15));
#29905=CARTESIAN_POINT('Origin',(-0.1,-1.05,-0.3));
#29906=CARTESIAN_POINT('',(0.,-1.,-0.3));
#29907=CARTESIAN_POINT('',(0.,-0.525,-0.3));
#29908=CARTESIAN_POINT('',(40.,-1.,-0.3));
#29909=CARTESIAN_POINT('',(-0.05,-1.,-0.3));
#29910=CARTESIAN_POINT('',(40.,-0.525,-0.3));
#29911=CARTESIAN_POINT('Origin',(-0.1,0.3,0.82));
#29912=CARTESIAN_POINT('',(0.,0.3,0.82));
#29913=CARTESIAN_POINT('',(0.,0.3,1.));
#29914=CARTESIAN_POINT('',(0.,0.3,0.41));
#29915=CARTESIAN_POINT('',(40.,0.3,0.82));
#29916=CARTESIAN_POINT('',(-0.1,0.3,0.82));
#29917=CARTESIAN_POINT('',(40.,0.3,1.));
#29918=CARTESIAN_POINT('',(40.,0.3,0.41));
#29919=CARTESIAN_POINT('',(-0.05,0.3,1.));
#29920=CARTESIAN_POINT('Origin',(-0.1,0.55,0.82));
#29921=CARTESIAN_POINT('',(0.,0.55,0.82));
#29922=CARTESIAN_POINT('',(0.,0.275,0.82));
#29923=CARTESIAN_POINT('',(40.,0.55,0.82));
#29924=CARTESIAN_POINT('',(-0.1,0.55,0.82));
#29925=CARTESIAN_POINT('',(40.,0.275,0.82));
#29926=CARTESIAN_POINT('Origin',(-0.1,0.55,0.67));
#29927=CARTESIAN_POINT('',(0.,0.55,0.67));
#29928=CARTESIAN_POINT('',(0.,0.55,0.335));
#29929=CARTESIAN_POINT('',(40.,0.55,0.67));
#29930=CARTESIAN_POINT('',(-0.1,0.55,0.67));
#29931=CARTESIAN_POINT('',(40.,0.55,0.335));
#29932=CARTESIAN_POINT('Origin',(-0.1,0.3,0.42));
#29933=CARTESIAN_POINT('',(0.,0.3,0.42));
#29934=CARTESIAN_POINT('',(6.93889390390723E-18,0.12,0.24));
#29935=CARTESIAN_POINT('',(40.,0.3,0.42));
#29936=CARTESIAN_POINT('',(-0.1,0.3,0.42));
#29937=CARTESIAN_POINT('',(40.,0.12,0.24));
#29938=CARTESIAN_POINT('Origin',(-0.1,-0.3,0.42));
#29939=CARTESIAN_POINT('',(0.,-0.3,0.42));
#29940=CARTESIAN_POINT('',(0.,-0.15,0.42));
#29941=CARTESIAN_POINT('',(40.,-0.3,0.42));
#29942=CARTESIAN_POINT('',(-0.1,-0.3,0.42));
#29943=CARTESIAN_POINT('',(40.,-0.15,0.42));
#29944=CARTESIAN_POINT('Origin',(-0.1,-0.55,0.67));
#29945=CARTESIAN_POINT('',(0.,-0.55,0.67));
#29946=CARTESIAN_POINT('',(6.93889390390723E-18,-0.245,0.365));
#29947=CARTESIAN_POINT('',(40.,-0.55,0.67));
#29948=CARTESIAN_POINT('',(-0.1,-0.55,0.67));
#29949=CARTESIAN_POINT('',(40.,-0.245,0.365));
#29950=CARTESIAN_POINT('Origin',(-0.1,-0.55,0.82));
#29951=CARTESIAN_POINT('',(0.,-0.55,0.82));
#29952=CARTESIAN_POINT('',(0.,-0.55,0.41));
#29953=CARTESIAN_POINT('',(40.,-0.55,0.82));
#29954=CARTESIAN_POINT('',(-0.1,-0.55,0.82));
#29955=CARTESIAN_POINT('',(40.,-0.55,0.41));
#29956=CARTESIAN_POINT('Origin',(-0.1,-0.3,0.82));
#29957=CARTESIAN_POINT('',(0.,-0.3,0.82));
#29958=CARTESIAN_POINT('',(0.,-0.15,0.82));
#29959=CARTESIAN_POINT('',(40.,-0.3,0.82));
#29960=CARTESIAN_POINT('',(-0.1,-0.3,0.82));
#29961=CARTESIAN_POINT('',(40.,-0.15,0.82));
#29962=CARTESIAN_POINT('Origin',(-0.1,-0.3,1.05));
#29963=CARTESIAN_POINT('',(0.,-0.3,1.));
#29964=CARTESIAN_POINT('',(0.,-0.3,0.525));
#29965=CARTESIAN_POINT('',(40.,-0.3,1.));
#29966=CARTESIAN_POINT('',(-0.05,-0.3,1.));
#29967=CARTESIAN_POINT('',(40.,-0.3,0.525));
#29968=CARTESIAN_POINT('Origin',(-0.1,0.,0.));
#29969=CARTESIAN_POINT('',(0.,-2.57175827820944E-17,0.21));
#29970=CARTESIAN_POINT('Origin',(0.,0.,0.));
#29971=CARTESIAN_POINT('',(40.,2.57175827820944E-17,0.21));
#29972=CARTESIAN_POINT('',(-0.1,-2.57175827820944E-17,0.21));
#29973=CARTESIAN_POINT('Origin',(40.,0.,0.));
#29974=CARTESIAN_POINT('Origin',(0.,1.,-1.));
#29975=CARTESIAN_POINT('',(0.,1.,1.));
#29976=CARTESIAN_POINT('',(0.,1.,-1.));
#29977=CARTESIAN_POINT('',(40.,1.,1.));
#29978=CARTESIAN_POINT('',(0.,1.,1.));
#29979=CARTESIAN_POINT('',(40.,1.,-1.));
#29980=CARTESIAN_POINT('Origin',(0.,1.,-1.));
#29981=CARTESIAN_POINT('',(40.,1.,-1.));
#29982=CARTESIAN_POINT('',(40.,1.,-1.));
#29983=CARTESIAN_POINT('',(0.,1.,-1.));
#29984=CARTESIAN_POINT('',(0.,1.,-1.));
#29985=CARTESIAN_POINT('',(0.,1.,-1.));
#29986=CARTESIAN_POINT('Origin',(0.,-1.,-1.));
#29987=CARTESIAN_POINT('',(0.,-1.,-1.));
#29988=CARTESIAN_POINT('',(40.,-1.,-1.));
#29989=CARTESIAN_POINT('Origin',(0.,-1.,-1.));
#29990=CARTESIAN_POINT('',(40.,-1.,-1.));
#29991=CARTESIAN_POINT('',(40.,-1.,-1.));
#29992=CARTESIAN_POINT('',(0.,-1.,-1.));
#29993=CARTESIAN_POINT('',(0.,-1.,-1.));
#29994=CARTESIAN_POINT('',(0.,-1.,-1.));
#29995=CARTESIAN_POINT('Origin',(0.,-1.,1.));
#29996=CARTESIAN_POINT('',(0.,-1.,1.));
#29997=CARTESIAN_POINT('',(40.,-1.,1.));
#29998=CARTESIAN_POINT('Origin',(0.,-1.,1.));
#29999=CARTESIAN_POINT('',(40.,-1.,1.));
#30000=CARTESIAN_POINT('',(40.,-1.,1.));
#30001=CARTESIAN_POINT('',(0.,-1.,1.));
#30002=CARTESIAN_POINT('',(0.,-1.,1.));
#30003=CARTESIAN_POINT('',(0.,-1.,1.));
#30004=CARTESIAN_POINT('Origin',(0.,1.,1.));
#30005=CARTESIAN_POINT('',(0.,1.,1.));
#30006=CARTESIAN_POINT('',(40.,1.,1.));
#30007=CARTESIAN_POINT('Origin',(0.,1.,1.));
#30008=CARTESIAN_POINT('',(40.,1.,1.));
#30009=CARTESIAN_POINT('',(0.,1.,1.));
#30010=CARTESIAN_POINT('Origin',(40.,0.,0.));
#30011=CARTESIAN_POINT('Origin',(0.,0.,0.));
#30012=CARTESIAN_POINT('',(0.,0.,0.));
#30013=CARTESIAN_POINT('Origin',(0.375,0.5,0.));
#30014=CARTESIAN_POINT('',(-0.375,0.5,-4.59242549680257E-17));
#30015=CARTESIAN_POINT('Origin',(0.,0.5,0.));
#30016=CARTESIAN_POINT('Origin',(0.,0.475,0.));
#30017=CARTESIAN_POINT('',(-0.425,0.45,-5.20474889637625E-17));
#30018=CARTESIAN_POINT('Origin',(0.,0.45,0.));
#30019=CARTESIAN_POINT('',(-0.4,0.475,-4.89858719658941E-17));
#30020=CARTESIAN_POINT('Origin',(0.,0.24,0.));
#30021=CARTESIAN_POINT('',(-0.425,0.0299999999999998,-5.20474889637625E-17));
#30022=CARTESIAN_POINT('Origin',(0.,0.0299999999999998,0.));
#30023=CARTESIAN_POINT('',(-0.425,0.24,-5.20474889637625E-17));
#30024=CARTESIAN_POINT('Origin',(0.,0.0150000000000001,0.));
#30025=CARTESIAN_POINT('',(-0.395,4.85722573273506E-17,-4.83735485663204E-17));
#30026=CARTESIAN_POINT('Origin',(0.,0.,0.));
#30027=CARTESIAN_POINT('',(-0.41,0.0150000000000001,-5.02105187650415E-17));
#30028=CARTESIAN_POINT('Origin',(0.27,0.,0.));
#30029=CARTESIAN_POINT('',(-0.27,0.,-3.30654635769785E-17));
#30030=CARTESIAN_POINT('Origin',(0.,0.,0.));
#30031=CARTESIAN_POINT('Origin',(0.,-0.02,0.));
#30032=CARTESIAN_POINT('',(-0.24505,-0.0498999999999999,3.00099698131059E-17));
#30033=CARTESIAN_POINT('Origin',(0.,-0.0498999999999999,0.));
#30034=CARTESIAN_POINT('',(-0.26,-0.02,-3.18408167778312E-17));
#30035=CARTESIAN_POINT('Origin',(0.,-0.995,0.));
#30036=CARTESIAN_POINT('',(-0.24505,-1.95495,3.00099698131059E-17));
#30037=CARTESIAN_POINT('Origin',(0.,-1.95495,0.));
#30038=CARTESIAN_POINT('',(-0.24505,-0.995,-3.00099698131059E-17));
#30039=CARTESIAN_POINT('Origin',(0.,-1.975,0.));
#30040=CARTESIAN_POINT('',(-0.2,-2.,-2.44929359829471E-17));
#30041=CARTESIAN_POINT('Origin',(0.,-2.,0.));
#30042=CARTESIAN_POINT('',(-0.225,-1.975,-2.75545529808154E-17));
#30043=CARTESIAN_POINT('Origin',(0.,-2.,0.));
#30044=CARTESIAN_POINT('Origin',(0.115470053837925,-0.5,-0.2));
#30045=CARTESIAN_POINT('',(0.23094010767585,-0.5,0.));
#30046=CARTESIAN_POINT('',(0.115470053837925,-0.5,-0.2));
#30047=CARTESIAN_POINT('',(0.23094010767585,-0.5,0.));
#30048=CARTESIAN_POINT('',(0.115470053837925,-0.8,-0.2));
#30049=CARTESIAN_POINT('',(0.115470053837925,-0.5,-0.2));
#30050=CARTESIAN_POINT('',(0.23094010767585,-0.8,0.));
#30051=CARTESIAN_POINT('',(0.23094010767585,-0.8,0.));
#30052=CARTESIAN_POINT('',(0.23094010767585,-0.5,0.));
#30053=CARTESIAN_POINT('Origin',(-0.115470053837925,-0.5,-0.2));
#30054=CARTESIAN_POINT('',(-0.115470053837925,-0.5,-0.2));
#30055=CARTESIAN_POINT('',(0.115470053837925,-0.5,-0.2));
#30056=CARTESIAN_POINT('',(-0.115470053837925,-0.8,-0.2));
#30057=CARTESIAN_POINT('',(-0.115470053837925,-0.5,-0.2));
#30058=CARTESIAN_POINT('',(0.115470053837925,-0.8,-0.2));
#30059=CARTESIAN_POINT('Origin',(-0.23094010767585,-0.5,-2.77555756156289E-17));
#30060=CARTESIAN_POINT('',(-0.23094010767585,-0.5,-2.82820063659975E-17));
#30061=CARTESIAN_POINT('',(-0.115470053837925,-0.5,-0.2));
#30062=CARTESIAN_POINT('',(-0.23094010767585,-0.8,-2.77555756156289E-17));
#30063=CARTESIAN_POINT('',(-0.23094010767585,-0.5,-2.82820063659975E-17));
#30064=CARTESIAN_POINT('',(-0.115470053837925,-0.8,-0.2));
#30065=CARTESIAN_POINT('Origin',(-0.115470053837925,-0.5,0.2));
#30066=CARTESIAN_POINT('',(-0.115470053837925,-0.5,0.2));
#30067=CARTESIAN_POINT('',(-0.23094010767585,-0.5,-2.82820063659975E-17));
#30068=CARTESIAN_POINT('',(-0.115470053837925,-0.8,0.2));
#30069=CARTESIAN_POINT('',(-0.115470053837925,-0.5,0.2));
#30070=CARTESIAN_POINT('',(-0.23094010767585,-0.8,-2.82820063659975E-17));
#30071=CARTESIAN_POINT('Origin',(0.115470053837925,-0.5,0.2));
#30072=CARTESIAN_POINT('',(0.115470053837925,-0.5,0.2));
#30073=CARTESIAN_POINT('',(-0.115470053837925,-0.5,0.2));
#30074=CARTESIAN_POINT('',(0.115470053837925,-0.8,0.2));
#30075=CARTESIAN_POINT('',(0.115470053837925,-0.5,0.2));
#30076=CARTESIAN_POINT('',(-0.115470053837925,-0.8,0.2));
#30077=CARTESIAN_POINT('Origin',(0.23094010767585,-0.5,0.));
#30078=CARTESIAN_POINT('',(0.115470053837925,-0.5,0.2));
#30079=CARTESIAN_POINT('',(0.115470053837925,-0.8,0.2));
#30080=CARTESIAN_POINT('Origin',(0.,-0.5,0.));
#30081=CARTESIAN_POINT('Origin',(0.,-0.8,0.));
#30082=CARTESIAN_POINT('',(0.,0.,0.));
#30083=CARTESIAN_POINT('Origin',(0.,0.395,0.25));
#30084=CARTESIAN_POINT('',(-0.5,0.3,0.25));
#30085=CARTESIAN_POINT('',(0.5,0.3,0.25));
#30086=CARTESIAN_POINT('',(0.25,0.3,0.25));
#30087=CARTESIAN_POINT('',(-0.5,0.5,0.25));
#30088=CARTESIAN_POINT('',(-0.5,0.5,0.25));
#30089=CARTESIAN_POINT('',(0.5,0.5,0.25));
#30090=CARTESIAN_POINT('',(0.5,0.5,0.25));
#30091=CARTESIAN_POINT('',(0.5,0.29,0.25));
#30092=CARTESIAN_POINT('Origin',(0.5,0.5,0.25));
#30093=CARTESIAN_POINT('',(-0.5,0.5,0.4));
#30094=CARTESIAN_POINT('',(-0.5,0.5,0.25));
#30095=CARTESIAN_POINT('',(0.5,0.5,0.4));
#30096=CARTESIAN_POINT('',(0.5,0.5,0.4));
#30097=CARTESIAN_POINT('',(0.5,0.5,0.25));
#30098=CARTESIAN_POINT('Origin',(0.,0.,0.4));
#30099=CARTESIAN_POINT('',(-0.5,-0.5,0.4));
#30100=CARTESIAN_POINT('',(-0.5,0.5,0.4));
#30101=CARTESIAN_POINT('',(0.5,-0.5,0.4));
#30102=CARTESIAN_POINT('',(-0.5,-0.5,0.4));
#30103=CARTESIAN_POINT('',(0.5,-0.3,0.4));
#30104=CARTESIAN_POINT('',(-0.2117,2.59257727379495E-17,0.4));
#30105=CARTESIAN_POINT('Origin',(0.,0.,0.4));
#30106=CARTESIAN_POINT('Origin',(-0.5,0.3,0.));
#30107=CARTESIAN_POINT('',(-0.5,0.3,0.15));
#30108=CARTESIAN_POINT('',(-0.5,0.3,0.));
#30109=CARTESIAN_POINT('',(-0.5,0.15,0.));
#30110=CARTESIAN_POINT('',(-0.5,0.225,0.075));
#30111=CARTESIAN_POINT('',(-0.5,-0.15,0.));
#30112=CARTESIAN_POINT('',(-0.5,0.3,0.));
#30113=CARTESIAN_POINT('',(-0.5,-0.3,0.15));
#30114=CARTESIAN_POINT('',(-0.5,-0.075,-0.075));
#30115=CARTESIAN_POINT('',(-0.5,-0.3,0.25));
#30116=CARTESIAN_POINT('',(-0.5,-0.3,0.));
#30117=CARTESIAN_POINT('',(-0.5,-0.5,0.25));
#30118=CARTESIAN_POINT('',(-0.5,-0.29,0.25));
#30119=CARTESIAN_POINT('',(-0.5,-0.5,0.25));
#30120=CARTESIAN_POINT('Origin',(-0.5,-0.5,0.25));
#30121=CARTESIAN_POINT('',(0.5,-0.5,0.25));
#30122=CARTESIAN_POINT('',(-0.5,-0.5,0.25));
#30123=CARTESIAN_POINT('',(0.5,-0.5,0.25));
#30124=CARTESIAN_POINT('Origin',(0.,-0.395,0.25));
#30125=CARTESIAN_POINT('',(0.5,-0.3,0.25));
#30126=CARTESIAN_POINT('',(-0.25,-0.3,0.25));
#30127=CARTESIAN_POINT('',(0.5,-0.5,0.25));
#30128=CARTESIAN_POINT('Origin',(0.5,-0.3,0.));
#30129=CARTESIAN_POINT('',(0.5,-0.3,0.15));
#30130=CARTESIAN_POINT('',(0.5,-0.3,0.));
#30131=CARTESIAN_POINT('',(0.5,-0.15,0.));
#30132=CARTESIAN_POINT('',(0.5,-0.225,0.075));
#30133=CARTESIAN_POINT('',(0.5,0.15,0.));
#30134=CARTESIAN_POINT('',(0.5,-0.3,0.));
#30135=CARTESIAN_POINT('',(0.5,0.3,0.15));
#30136=CARTESIAN_POINT('',(0.5,0.075,-0.075));
#30137=CARTESIAN_POINT('',(0.5,0.3,0.));
#30138=CARTESIAN_POINT('Origin',(-0.5,-0.3,0.));
#30139=CARTESIAN_POINT('',(-0.25,-0.3,0.15));
#30140=CARTESIAN_POINT('Origin',(-0.25,-0.225,0.075));
#30141=CARTESIAN_POINT('',(-0.149388386429468,-0.15,0.));
#30142=CARTESIAN_POINT('',(-0.25,-0.15,0.));
#30143=CARTESIAN_POINT('',(0.149388386429468,-0.15,0.));
#30144=CARTESIAN_POINT('Origin',(0.,0.,-0.15));
#30145=CARTESIAN_POINT('',(-0.25,-0.15,0.));
#30146=CARTESIAN_POINT('Origin',(0.,0.,-0.1));
#30147=CARTESIAN_POINT('',(-0.2117,-2.59257727379495E-17,0.));
#30148=CARTESIAN_POINT('Origin',(0.,0.,0.));
#30149=CARTESIAN_POINT('',(-0.2117,-2.59257727379495E-17,-0.1));
#30150=CARTESIAN_POINT('',(-0.149388386429468,0.15,0.));
#30151=CARTESIAN_POINT('Origin',(0.,0.,0.));
#30152=CARTESIAN_POINT('',(0.149388386429468,0.15,0.));
#30153=CARTESIAN_POINT('Origin',(0.,0.,-0.15));
#30154=CARTESIAN_POINT('Origin',(0.,0.,0.));
#30155=CARTESIAN_POINT('Origin',(0.,0.,0.));
#30156=CARTESIAN_POINT('',(0.25,0.15,0.));
#30157=CARTESIAN_POINT('Origin',(0.,0.,0.));
#30158=CARTESIAN_POINT('',(0.25,0.15,0.));
#30159=CARTESIAN_POINT('Origin',(0.25,0.225,0.075));
#30160=CARTESIAN_POINT('',(0.25,0.3,0.15));
#30161=CARTESIAN_POINT('Origin',(0.5,0.3,0.));
#30162=CARTESIAN_POINT('',(0.,0.,0.));
#30163=CARTESIAN_POINT('Origin',(0.,-0.8,0.));
#30164=CARTESIAN_POINT('',(-0.24505,-0.8,3.00099698131059E-17));
#30165=CARTESIAN_POINT('Origin',(0.,-0.8,0.));
#30166=CARTESIAN_POINT('',(0.115470053837925,-0.8,-0.2));
#30167=CARTESIAN_POINT('',(0.23094010767585,-0.8,0.));
#30168=CARTESIAN_POINT('',(0.23094010767585,-0.8,0.));
#30169=CARTESIAN_POINT('',(-0.115470053837925,-0.8,-0.2));
#30170=CARTESIAN_POINT('',(0.115470053837925,-0.8,-0.2));
#30171=CARTESIAN_POINT('',(-0.23094010767585,-0.8,-2.77555756156289E-17));
#30172=CARTESIAN_POINT('',(-0.115470053837925,-0.8,-0.2));
#30173=CARTESIAN_POINT('',(-0.115470053837925,-0.8,0.2));
#30174=CARTESIAN_POINT('',(-0.23094010767585,-0.8,-2.82820063659975E-17));
#30175=CARTESIAN_POINT('',(0.115470053837925,-0.8,0.2));
#30176=CARTESIAN_POINT('',(-0.115470053837925,-0.8,0.2));
#30177=CARTESIAN_POINT('',(0.115470053837925,-0.8,0.2));
#30178=CARTESIAN_POINT('Origin',(0.375,0.5,0.));
#30179=CARTESIAN_POINT('',(-0.375,0.5,-4.59242549680257E-17));
#30180=CARTESIAN_POINT('Origin',(0.,0.5,0.));
#30181=CARTESIAN_POINT('Origin',(0.,0.475,0.));
#30182=CARTESIAN_POINT('',(-0.425,0.45,-5.20474889637625E-17));
#30183=CARTESIAN_POINT('Origin',(0.,0.45,0.));
#30184=CARTESIAN_POINT('',(-0.4,0.475,-4.89858719658941E-17));
#30185=CARTESIAN_POINT('Origin',(0.,0.24,0.));
#30186=CARTESIAN_POINT('',(-0.425,0.0299999999999998,-5.20474889637625E-17));
#30187=CARTESIAN_POINT('Origin',(0.,0.0299999999999998,0.));
#30188=CARTESIAN_POINT('',(-0.425,0.24,-5.20474889637625E-17));
#30189=CARTESIAN_POINT('Origin',(0.,0.0150000000000001,0.));
#30190=CARTESIAN_POINT('',(-0.395,4.85722573273506E-17,-4.83735485663204E-17));
#30191=CARTESIAN_POINT('Origin',(0.,0.,0.));
#30192=CARTESIAN_POINT('',(-0.41,0.0150000000000001,-5.02105187650415E-17));
#30193=CARTESIAN_POINT('Origin',(0.27,0.,0.));
#30194=CARTESIAN_POINT('',(-0.27,0.,-3.30654635769785E-17));
#30195=CARTESIAN_POINT('Origin',(0.,0.,0.));
#30196=CARTESIAN_POINT('Origin',(0.,-0.02,0.));
#30197=CARTESIAN_POINT('',(-0.24505,-0.0498999999999999,3.00099698131059E-17));
#30198=CARTESIAN_POINT('Origin',(0.,-0.0498999999999999,0.));
#30199=CARTESIAN_POINT('',(-0.26,-0.02,-3.18408167778312E-17));
#30200=CARTESIAN_POINT('Origin',(0.,-0.995,0.));
#30201=CARTESIAN_POINT('',(-0.24505,-0.995,-3.00099698131059E-17));
#30202=CARTESIAN_POINT('Origin',(0.115470053837925,-0.5,-0.2));
#30203=CARTESIAN_POINT('',(0.23094010767585,-0.5,0.));
#30204=CARTESIAN_POINT('',(0.115470053837925,-0.5,-0.2));
#30205=CARTESIAN_POINT('',(0.23094010767585,-0.5,0.));
#30206=CARTESIAN_POINT('',(0.115470053837925,-0.5,-0.2));
#30207=CARTESIAN_POINT('',(0.23094010767585,-0.5,0.));
#30208=CARTESIAN_POINT('Origin',(-0.115470053837925,-0.5,-0.2));
#30209=CARTESIAN_POINT('',(-0.115470053837925,-0.5,-0.2));
#30210=CARTESIAN_POINT('',(0.115470053837925,-0.5,-0.2));
#30211=CARTESIAN_POINT('',(-0.115470053837925,-0.5,-0.2));
#30212=CARTESIAN_POINT('Origin',(-0.23094010767585,-0.5,-2.77555756156289E-17));
#30213=CARTESIAN_POINT('',(-0.23094010767585,-0.5,-2.82820063659975E-17));
#30214=CARTESIAN_POINT('',(-0.115470053837925,-0.5,-0.2));
#30215=CARTESIAN_POINT('',(-0.23094010767585,-0.5,-2.82820063659975E-17));
#30216=CARTESIAN_POINT('Origin',(-0.115470053837925,-0.5,0.2));
#30217=CARTESIAN_POINT('',(-0.115470053837925,-0.5,0.2));
#30218=CARTESIAN_POINT('',(-0.23094010767585,-0.5,-2.82820063659975E-17));
#30219=CARTESIAN_POINT('',(-0.115470053837925,-0.5,0.2));
#30220=CARTESIAN_POINT('Origin',(0.115470053837925,-0.5,0.2));
#30221=CARTESIAN_POINT('',(0.115470053837925,-0.5,0.2));
#30222=CARTESIAN_POINT('',(-0.115470053837925,-0.5,0.2));
#30223=CARTESIAN_POINT('',(0.115470053837925,-0.5,0.2));
#30224=CARTESIAN_POINT('Origin',(0.23094010767585,-0.5,0.));
#30225=CARTESIAN_POINT('',(0.115470053837925,-0.5,0.2));
#30226=CARTESIAN_POINT('Origin',(0.,-0.5,0.));
#30227=CARTESIAN_POINT('',(0.,0.,0.));
#30228=CARTESIAN_POINT('',(0.,0.,0.));
#30229=CARTESIAN_POINT('Origin',(7.2,-0.35,15.));
#30230=CARTESIAN_POINT('',(7.035,-0.35,15.1));
#30231=CARTESIAN_POINT('Origin',(7.2,-0.35,15.1));
#30232=CARTESIAN_POINT('',(7.035,-0.35,16.3));
#30233=CARTESIAN_POINT('',(7.035,-0.35,15.));
#30234=CARTESIAN_POINT('Origin',(7.2,-0.35,16.3));
#30235=CARTESIAN_POINT('Origin',(7.2,0.35,15.));
#30236=CARTESIAN_POINT('',(7.035,0.35,15.1));
#30237=CARTESIAN_POINT('Origin',(7.2,0.35,15.1));
#30238=CARTESIAN_POINT('',(7.035,0.35,16.3));
#30239=CARTESIAN_POINT('',(7.035,0.35,15.));
#30240=CARTESIAN_POINT('Origin',(7.2,0.35,16.3));
#30241=CARTESIAN_POINT('Origin',(-2.,-1.5,15.));
#30242=CARTESIAN_POINT('',(-2.225,-1.5,15.1));
#30243=CARTESIAN_POINT('Origin',(-2.,-1.5,15.1));
#30244=CARTESIAN_POINT('',(-2.225,-1.5,16.3));
#30245=CARTESIAN_POINT('',(-2.225,-1.5,15.));
#30246=CARTESIAN_POINT('Origin',(-2.,-1.5,16.3));
#30247=CARTESIAN_POINT('Origin',(2.,-1.5,15.));
#30248=CARTESIAN_POINT('',(1.775,-1.5,15.1));
#30249=CARTESIAN_POINT('Origin',(2.,-1.5,15.1));
#30250=CARTESIAN_POINT('',(1.775,-1.5,16.3));
#30251=CARTESIAN_POINT('',(1.775,-1.5,15.));
#30252=CARTESIAN_POINT('Origin',(2.,-1.5,16.3));
#30253=CARTESIAN_POINT('Origin',(0.,3.5,15.));
#30254=CARTESIAN_POINT('',(-0.225,3.5,15.1));
#30255=CARTESIAN_POINT('Origin',(0.,3.5,15.1));
#30256=CARTESIAN_POINT('',(-0.225,3.5,16.3));
#30257=CARTESIAN_POINT('',(-0.225,3.5,15.));
#30258=CARTESIAN_POINT('Origin',(0.,3.5,16.3));
#30259=CARTESIAN_POINT('Origin',(0.,6.5,15.));
#30260=CARTESIAN_POINT('',(-0.225,6.5,15.1));
#30261=CARTESIAN_POINT('Origin',(0.,6.5,15.1));
#30262=CARTESIAN_POINT('',(-0.225,6.5,16.3));
#30263=CARTESIAN_POINT('',(-0.225,6.5,15.));
#30264=CARTESIAN_POINT('Origin',(0.,6.5,16.3));
#30265=CARTESIAN_POINT('Origin',(-1.5,5.,15.));
#30266=CARTESIAN_POINT('',(-1.725,5.,15.1));
#30267=CARTESIAN_POINT('Origin',(-1.5,5.,15.1));
#30268=CARTESIAN_POINT('',(-1.725,5.,16.3));
#30269=CARTESIAN_POINT('',(-1.725,5.,15.));
#30270=CARTESIAN_POINT('Origin',(-1.5,5.,16.3));
#30271=CARTESIAN_POINT('Origin',(4.86862915010152,-1.13137084989848,15.));
#30272=CARTESIAN_POINT('',(4.64362915010152,-1.13137084989848,15.1));
#30273=CARTESIAN_POINT('Origin',(4.86862915010152,-1.13137084989848,15.1));
#30274=CARTESIAN_POINT('',(4.64362915010152,-1.13137084989848,16.3));
#30275=CARTESIAN_POINT('',(4.64362915010152,-1.13137084989848,15.));
#30276=CARTESIAN_POINT('Origin',(4.86862915010152,-1.13137084989848,16.3));
#30277=CARTESIAN_POINT('Origin',(4.86862915010152,1.13137084989848,15.));
#30278=CARTESIAN_POINT('',(4.64362915010152,1.13137084989848,15.1));
#30279=CARTESIAN_POINT('Origin',(4.86862915010152,1.13137084989848,15.1));
#30280=CARTESIAN_POINT('',(4.64362915010152,1.13137084989848,16.3));
#30281=CARTESIAN_POINT('',(4.64362915010152,1.13137084989848,15.));
#30282=CARTESIAN_POINT('Origin',(4.86862915010152,1.13137084989848,16.3));
#30283=CARTESIAN_POINT('Origin',(7.13137084989848,1.13137084989848,15.));
#30284=CARTESIAN_POINT('',(6.90637084989848,1.13137084989848,15.1));
#30285=CARTESIAN_POINT('Origin',(7.13137084989848,1.13137084989848,15.1));
#30286=CARTESIAN_POINT('',(6.90637084989848,1.13137084989848,16.3));
#30287=CARTESIAN_POINT('',(6.90637084989848,1.13137084989848,15.));
#30288=CARTESIAN_POINT('Origin',(7.13137084989848,1.13137084989848,16.3));
#30289=CARTESIAN_POINT('Origin',(7.13137084989848,-1.13137084989848,15.));
#30290=CARTESIAN_POINT('',(6.90637084989848,-1.13137084989848,15.1));
#30291=CARTESIAN_POINT('Origin',(7.13137084989848,-1.13137084989848,15.1));
#30292=CARTESIAN_POINT('',(6.90637084989848,-1.13137084989848,16.3));
#30293=CARTESIAN_POINT('',(6.90637084989848,-1.13137084989848,15.));
#30294=CARTESIAN_POINT('Origin',(7.13137084989848,-1.13137084989848,16.3));
#30295=CARTESIAN_POINT('Origin',(-7.13137084989848,-1.13137084989848,15.));
#30296=CARTESIAN_POINT('',(-7.35637084989848,-1.13137084989848,15.1));
#30297=CARTESIAN_POINT('Origin',(-7.13137084989848,-1.13137084989848,15.1));
#30298=CARTESIAN_POINT('',(-7.35637084989848,-1.13137084989848,16.3));
#30299=CARTESIAN_POINT('',(-7.35637084989848,-1.13137084989848,15.));
#30300=CARTESIAN_POINT('Origin',(-7.13137084989848,-1.13137084989848,16.3));
#30301=CARTESIAN_POINT('Origin',(-7.13137084989848,1.13137084989848,15.));
#30302=CARTESIAN_POINT('',(-7.35637084989848,1.13137084989848,15.1));
#30303=CARTESIAN_POINT('Origin',(-7.13137084989848,1.13137084989848,15.1));
#30304=CARTESIAN_POINT('',(-7.35637084989848,1.13137084989848,16.3));
#30305=CARTESIAN_POINT('',(-7.35637084989848,1.13137084989848,15.));
#30306=CARTESIAN_POINT('Origin',(-7.13137084989848,1.13137084989848,16.3));
#30307=CARTESIAN_POINT('Origin',(-4.86862915010152,1.13137084989848,15.));
#30308=CARTESIAN_POINT('',(-5.09362915010152,1.13137084989848,15.1));
#30309=CARTESIAN_POINT('Origin',(-4.86862915010152,1.13137084989848,15.1));
#30310=CARTESIAN_POINT('',(-5.09362915010152,1.13137084989848,16.3));
#30311=CARTESIAN_POINT('',(-5.09362915010152,1.13137084989848,15.));
#30312=CARTESIAN_POINT('Origin',(-4.86862915010152,1.13137084989848,16.3));
#30313=CARTESIAN_POINT('Origin',(-4.86862915010152,-1.13137084989848,15.));
#30314=CARTESIAN_POINT('',(-5.09362915010152,-1.13137084989848,15.1));
#30315=CARTESIAN_POINT('Origin',(-4.86862915010152,-1.13137084989848,15.1));
#30316=CARTESIAN_POINT('',(-5.09362915010152,-1.13137084989848,16.3));
#30317=CARTESIAN_POINT('',(-5.09362915010152,-1.13137084989848,15.));
#30318=CARTESIAN_POINT('Origin',(-4.86862915010152,-1.13137084989848,16.3));
#30319=CARTESIAN_POINT('Origin',(0.,5.,15.));
#30320=CARTESIAN_POINT('',(-0.625,5.,15.1));
#30321=CARTESIAN_POINT('Origin',(0.,5.,15.1));
#30322=CARTESIAN_POINT('',(-0.625,5.,16.3));
#30323=CARTESIAN_POINT('',(-0.625,5.,15.));
#30324=CARTESIAN_POINT('Origin',(0.,5.,16.3));
#30325=CARTESIAN_POINT('Origin',(-6.,0.,15.));
#30326=CARTESIAN_POINT('',(-6.625,-7.65404249467096E-17,15.1));
#30327=CARTESIAN_POINT('Origin',(-6.,0.,15.1));
#30328=CARTESIAN_POINT('',(-6.625,7.65404249467096E-17,16.3));
#30329=CARTESIAN_POINT('',(-6.625,-7.65404249467096E-17,15.));
#30330=CARTESIAN_POINT('Origin',(-6.,0.,16.3));
#30331=CARTESIAN_POINT('Origin',(6.,0.,15.));
#30332=CARTESIAN_POINT('',(5.375,-7.65404249467096E-17,15.1));
#30333=CARTESIAN_POINT('Origin',(6.,0.,15.1));
#30334=CARTESIAN_POINT('',(5.375,7.65404249467096E-17,16.3));
#30335=CARTESIAN_POINT('',(5.375,-7.65404249467096E-17,15.));
#30336=CARTESIAN_POINT('Origin',(6.,0.,16.3));
#30337=CARTESIAN_POINT('Origin',(7.5,7.5,15.1));
#30338=CARTESIAN_POINT('',(7.5,7.5,15.1));
#30339=CARTESIAN_POINT('',(-7.5,7.5,15.1));
#30340=CARTESIAN_POINT('',(7.5,7.5,15.1));
#30341=CARTESIAN_POINT('',(-7.5,7.5,16.3));
#30342=CARTESIAN_POINT('',(-7.5,7.5,15.1));
#30343=CARTESIAN_POINT('',(7.5,7.5,16.3));
#30344=CARTESIAN_POINT('',(7.5,7.5,16.3));
#30345=CARTESIAN_POINT('',(7.5,7.5,15.1));
#30346=CARTESIAN_POINT('Origin',(7.5,-3.5,15.1));
#30347=CARTESIAN_POINT('',(7.5,-3.5,15.1));
#30348=CARTESIAN_POINT('',(7.5,-3.5,15.1));
#30349=CARTESIAN_POINT('',(7.5,-3.5,16.3));
#30350=CARTESIAN_POINT('',(7.5,-3.5,16.3));
#30351=CARTESIAN_POINT('',(7.5,-3.5,15.1));
#30352=CARTESIAN_POINT('Origin',(-7.5,-3.5,15.1));
#30353=CARTESIAN_POINT('',(-7.5,-3.5,15.1));
#30354=CARTESIAN_POINT('',(-7.5,-3.5,15.1));
#30355=CARTESIAN_POINT('',(-7.5,-3.5,16.3));
#30356=CARTESIAN_POINT('',(-7.5,-3.5,16.3));
#30357=CARTESIAN_POINT('',(-7.5,-3.5,15.1));
#30358=CARTESIAN_POINT('Origin',(-7.5,7.5,15.1));
#30359=CARTESIAN_POINT('',(-7.5,7.5,15.1));
#30360=CARTESIAN_POINT('',(-7.5,7.5,16.3));
#30361=CARTESIAN_POINT('Origin',(0.,2.,16.3));
#30362=CARTESIAN_POINT('Origin',(0.,2.,15.1));
#30363=CARTESIAN_POINT('',(0.,0.,0.));
#30364=CARTESIAN_POINT('Origin',(-7.13137084989848,-1.13137084989848,14.));
#30365=CARTESIAN_POINT('',(-6.96707794165985,-1.14662995545858,14.));
#30366=CARTESIAN_POINT('',(-7.14662995545858,-0.96707794165985,14.));
#30367=CARTESIAN_POINT('Origin',(-6.,0.,14.));
#30368=CARTESIAN_POINT('Origin',(-7.13137084989848,-1.13137084989848,14.));
#30369=CARTESIAN_POINT('Origin',(-7.13137084989848,-1.13137084989848,14.));
#30370=CARTESIAN_POINT('',(-6.96707794165985,-1.14662995545858,14.6));
#30371=CARTESIAN_POINT('',(-6.96707794165985,-1.14662995545858,14.));
#30372=CARTESIAN_POINT('',(-7.29637084989848,-1.13137084989848,14.6));
#30373=CARTESIAN_POINT('Origin',(-7.13137084989848,-1.13137084989848,14.6));
#30374=CARTESIAN_POINT('',(-7.29637084989848,-1.13137084989848,15.1));
#30375=CARTESIAN_POINT('',(-7.29637084989848,-1.13137084989848,14.));
#30376=CARTESIAN_POINT('Origin',(-7.13137084989848,-1.13137084989848,15.1));
#30377=CARTESIAN_POINT('',(-7.14662995545858,-0.967077941659851,14.6));
#30378=CARTESIAN_POINT('Origin',(-7.13137084989848,-1.13137084989848,14.6));
#30379=CARTESIAN_POINT('',(-7.14662995545858,-0.96707794165985,14.));
#30380=CARTESIAN_POINT('Origin',(-7.13137084989848,1.13137084989848,14.));
#30381=CARTESIAN_POINT('',(-7.14662995545858,0.96707794165985,14.));
#30382=CARTESIAN_POINT('',(-6.96707794165985,1.14662995545858,14.));
#30383=CARTESIAN_POINT('Origin',(-6.,0.,14.));
#30384=CARTESIAN_POINT('Origin',(-7.13137084989848,1.13137084989848,14.));
#30385=CARTESIAN_POINT('Origin',(-7.13137084989848,1.13137084989848,14.));
#30386=CARTESIAN_POINT('',(-7.14662995545858,0.967077941659851,14.6));
#30387=CARTESIAN_POINT('',(-7.14662995545858,0.96707794165985,14.));
#30388=CARTESIAN_POINT('',(-7.29637084989848,1.13137084989848,14.6));
#30389=CARTESIAN_POINT('Origin',(-7.13137084989848,1.13137084989848,14.6));
#30390=CARTESIAN_POINT('',(-7.29637084989848,1.13137084989848,15.1));
#30391=CARTESIAN_POINT('',(-7.29637084989848,1.13137084989848,14.));
#30392=CARTESIAN_POINT('Origin',(-7.13137084989848,1.13137084989848,15.1));
#30393=CARTESIAN_POINT('',(-6.96707794165985,1.14662995545858,14.6));
#30394=CARTESIAN_POINT('Origin',(-7.13137084989848,1.13137084989848,14.6));
#30395=CARTESIAN_POINT('',(-6.96707794165985,1.14662995545858,14.));
#30396=CARTESIAN_POINT('Origin',(-4.86862915010152,1.13137084989848,14.));
#30397=CARTESIAN_POINT('',(-5.03292205834015,1.14662995545858,14.));
#30398=CARTESIAN_POINT('',(-4.85337004454142,0.96707794165985,14.));
#30399=CARTESIAN_POINT('Origin',(-6.,0.,14.));
#30400=CARTESIAN_POINT('',(-5.03362915010152,1.13137084989848,14.));
#30401=CARTESIAN_POINT('Origin',(-4.86862915010152,1.13137084989848,14.));
#30402=CARTESIAN_POINT('Origin',(-4.86862915010152,1.13137084989848,14.));
#30403=CARTESIAN_POINT('Origin',(-4.86862915010152,1.13137084989848,14.));
#30404=CARTESIAN_POINT('',(-5.03292205834015,1.14662995545858,14.6));
#30405=CARTESIAN_POINT('',(-5.03292205834015,1.14662995545858,14.));
#30406=CARTESIAN_POINT('',(-4.85337004454142,0.967077941659849,14.6));
#30407=CARTESIAN_POINT('Origin',(-4.86862915010152,1.13137084989848,14.6));
#30408=CARTESIAN_POINT('',(-4.85337004454142,0.96707794165985,14.));
#30409=CARTESIAN_POINT('',(-5.03362915010152,1.13137084989848,15.1));
#30410=CARTESIAN_POINT('',(-5.03362915010152,1.13137084989848,14.));
#30411=CARTESIAN_POINT('Origin',(-4.86862915010152,1.13137084989848,15.1));
#30412=CARTESIAN_POINT('Origin',(-4.86862915010152,-1.13137084989848,14.));
#30413=CARTESIAN_POINT('',(-4.85337004454142,-0.96707794165985,14.));
#30414=CARTESIAN_POINT('',(-5.03292205834015,-1.14662995545858,14.));
#30415=CARTESIAN_POINT('Origin',(-6.,0.,14.));
#30416=CARTESIAN_POINT('',(-5.03362915010152,-1.13137084989848,14.));
#30417=CARTESIAN_POINT('Origin',(-4.86862915010152,-1.13137084989848,14.));
#30418=CARTESIAN_POINT('Origin',(-4.86862915010152,-1.13137084989848,14.));
#30419=CARTESIAN_POINT('Origin',(-4.86862915010152,-1.13137084989848,14.));
#30420=CARTESIAN_POINT('',(-4.85337004454142,-0.967077941659849,14.6));
#30421=CARTESIAN_POINT('',(-4.85337004454142,-0.96707794165985,14.));
#30422=CARTESIAN_POINT('',(-5.03292205834015,-1.14662995545858,14.6));
#30423=CARTESIAN_POINT('Origin',(-4.86862915010152,-1.13137084989848,14.6));
#30424=CARTESIAN_POINT('',(-5.03292205834015,-1.14662995545858,14.));
#30425=CARTESIAN_POINT('',(-5.03362915010152,-1.13137084989848,15.1));
#30426=CARTESIAN_POINT('',(-5.03362915010152,-1.13137084989848,14.));
#30427=CARTESIAN_POINT('Origin',(-4.86862915010152,-1.13137084989848,15.1));
#30428=CARTESIAN_POINT('Origin',(-6.,0.,11.5));
#30429=CARTESIAN_POINT('',(-7.5,-1.83697019872103E-16,14.6));
#30430=CARTESIAN_POINT('Origin',(-6.,0.,14.6));
#30431=CARTESIAN_POINT('',(-7.5,-1.83697019872103E-16,11.5));
#30432=CARTESIAN_POINT('',(-7.5,-1.83697019872103E-16,11.5));
#30433=CARTESIAN_POINT('Origin',(-6.,0.,11.5));
#30434=CARTESIAN_POINT('Origin',(-6.,0.,14.6));
#30435=CARTESIAN_POINT('Origin',(-6.,0.,14.6));
#30436=CARTESIAN_POINT('Origin',(-6.,0.,14.6));
#30437=CARTESIAN_POINT('Origin',(-6.,0.,14.6));
#30438=CARTESIAN_POINT('Origin',(-6.,0.,12.1));
#30439=CARTESIAN_POINT('',(-7.05,-1.28587913910472E-16,12.1));
#30440=CARTESIAN_POINT('Origin',(-6.,0.,12.1));
#30441=CARTESIAN_POINT('',(-7.05,1.28587913910472E-16,15.1));
#30442=CARTESIAN_POINT('',(-7.05,-1.28587913910472E-16,12.1));
#30443=CARTESIAN_POINT('Origin',(-6.,0.,15.1));
#30444=CARTESIAN_POINT('Origin',(-6.,0.,12.1));
#30445=CARTESIAN_POINT('',(-6.625,-7.65404249467096E-17,12.1));
#30446=CARTESIAN_POINT('Origin',(-6.,0.,12.1));
#30447=CARTESIAN_POINT('Origin',(-6.,0.,14.6));
#30448=CARTESIAN_POINT('',(-8.,-2.44929359829471E-16,14.6));
#30449=CARTESIAN_POINT('Origin',(-6.,0.,14.6));
#30450=CARTESIAN_POINT('Origin',(-6.,0.,14.6));
#30451=CARTESIAN_POINT('',(-8.,-2.44929359829471E-16,15.1));
#30452=CARTESIAN_POINT('Origin',(-6.,0.,15.1));
#30453=CARTESIAN_POINT('',(-8.,-2.44929359829471E-16,14.6));
#30454=CARTESIAN_POINT('Origin',(-6.,0.,11.5));
#30455=CARTESIAN_POINT('',(-6.625,-7.65404249467096E-17,11.5));
#30456=CARTESIAN_POINT('',(-6.625,-7.65404249467096E-17,11.5));
#30457=CARTESIAN_POINT('Origin',(-6.,0.,11.5));
#30458=CARTESIAN_POINT('Origin',(-6.,0.,15.1));
#30459=CARTESIAN_POINT('Origin',(-6.,0.,11.5));
#30460=CARTESIAN_POINT('',(0.,0.,0.));
#30461=CARTESIAN_POINT('Origin',(4.86862915010152,-1.13137084989848,14.));
#30462=CARTESIAN_POINT('',(5.03292205834015,-1.14662995545858,14.));
#30463=CARTESIAN_POINT('',(4.85337004454142,-0.96707794165985,14.));
#30464=CARTESIAN_POINT('Origin',(6.,0.,14.));
#30465=CARTESIAN_POINT('Origin',(4.86862915010152,-1.13137084989848,14.));
#30466=CARTESIAN_POINT('Origin',(4.86862915010152,-1.13137084989848,14.));
#30467=CARTESIAN_POINT('',(5.03292205834015,-1.14662995545858,14.6));
#30468=CARTESIAN_POINT('',(5.03292205834015,-1.14662995545858,14.));
#30469=CARTESIAN_POINT('',(4.70362915010152,-1.13137084989848,14.6));
#30470=CARTESIAN_POINT('Origin',(4.86862915010152,-1.13137084989848,14.6));
#30471=CARTESIAN_POINT('',(4.70362915010152,-1.13137084989848,15.1));
#30472=CARTESIAN_POINT('',(4.70362915010152,-1.13137084989848,14.));
#30473=CARTESIAN_POINT('Origin',(4.86862915010152,-1.13137084989848,15.1));
#30474=CARTESIAN_POINT('',(4.85337004454142,-0.967077941659851,14.6));
#30475=CARTESIAN_POINT('Origin',(4.86862915010152,-1.13137084989848,14.6));
#30476=CARTESIAN_POINT('',(4.85337004454142,-0.96707794165985,14.));
#30477=CARTESIAN_POINT('Origin',(4.86862915010152,1.13137084989848,14.));
#30478=CARTESIAN_POINT('',(4.85337004454142,0.96707794165985,14.));
#30479=CARTESIAN_POINT('',(5.03292205834015,1.14662995545858,14.));
#30480=CARTESIAN_POINT('Origin',(6.,0.,14.));
#30481=CARTESIAN_POINT('Origin',(4.86862915010152,1.13137084989848,14.));
#30482=CARTESIAN_POINT('Origin',(4.86862915010152,1.13137084989848,14.));
#30483=CARTESIAN_POINT('',(4.85337004454142,0.967077941659849,14.6));
#30484=CARTESIAN_POINT('',(4.85337004454142,0.96707794165985,14.));
#30485=CARTESIAN_POINT('',(4.70362915010152,1.13137084989848,14.6));
#30486=CARTESIAN_POINT('Origin',(4.86862915010152,1.13137084989848,14.6));
#30487=CARTESIAN_POINT('',(4.70362915010152,1.13137084989848,15.1));
#30488=CARTESIAN_POINT('',(4.70362915010152,1.13137084989848,14.));
#30489=CARTESIAN_POINT('Origin',(4.86862915010152,1.13137084989848,15.1));
#30490=CARTESIAN_POINT('',(5.03292205834015,1.14662995545858,14.6));
#30491=CARTESIAN_POINT('Origin',(4.86862915010152,1.13137084989848,14.6));
#30492=CARTESIAN_POINT('',(5.03292205834015,1.14662995545858,14.));
#30493=CARTESIAN_POINT('Origin',(7.13137084989848,1.13137084989848,14.));
#30494=CARTESIAN_POINT('',(6.96707794165985,1.14662995545858,14.));
#30495=CARTESIAN_POINT('',(7.14662995545858,0.96707794165985,14.));
#30496=CARTESIAN_POINT('Origin',(6.,0.,14.));
#30497=CARTESIAN_POINT('',(6.96637084989848,1.13137084989848,14.));
#30498=CARTESIAN_POINT('Origin',(7.13137084989848,1.13137084989848,14.));
#30499=CARTESIAN_POINT('Origin',(7.13137084989848,1.13137084989848,14.));
#30500=CARTESIAN_POINT('Origin',(7.13137084989848,1.13137084989848,14.));
#30501=CARTESIAN_POINT('',(6.96707794165985,1.14662995545858,14.6));
#30502=CARTESIAN_POINT('',(6.96707794165985,1.14662995545858,14.));
#30503=CARTESIAN_POINT('',(7.14662995545858,0.967077941659851,14.6));
#30504=CARTESIAN_POINT('Origin',(7.13137084989848,1.13137084989848,14.6));
#30505=CARTESIAN_POINT('',(7.14662995545858,0.96707794165985,14.));
#30506=CARTESIAN_POINT('',(6.96637084989848,1.13137084989848,15.1));
#30507=CARTESIAN_POINT('',(6.96637084989848,1.13137084989848,14.));
#30508=CARTESIAN_POINT('Origin',(7.13137084989848,1.13137084989848,15.1));
#30509=CARTESIAN_POINT('Origin',(7.13137084989848,-1.13137084989848,14.));
#30510=CARTESIAN_POINT('',(7.14662995545858,-0.96707794165985,14.));
#30511=CARTESIAN_POINT('',(6.96707794165985,-1.14662995545858,14.));
#30512=CARTESIAN_POINT('Origin',(6.,0.,14.));
#30513=CARTESIAN_POINT('',(6.96637084989848,-1.13137084989848,14.));
#30514=CARTESIAN_POINT('Origin',(7.13137084989848,-1.13137084989848,14.));
#30515=CARTESIAN_POINT('Origin',(7.13137084989848,-1.13137084989848,14.));
#30516=CARTESIAN_POINT('Origin',(7.13137084989848,-1.13137084989848,14.));
#30517=CARTESIAN_POINT('',(7.14662995545858,-0.967077941659849,14.6));
#30518=CARTESIAN_POINT('',(7.14662995545858,-0.96707794165985,14.));
#30519=CARTESIAN_POINT('',(6.96707794165985,-1.14662995545858,14.6));
#30520=CARTESIAN_POINT('Origin',(7.13137084989848,-1.13137084989848,14.6));
#30521=CARTESIAN_POINT('',(6.96707794165985,-1.14662995545858,14.));
#30522=CARTESIAN_POINT('',(6.96637084989848,-1.13137084989848,15.1));
#30523=CARTESIAN_POINT('',(6.96637084989848,-1.13137084989848,14.));
#30524=CARTESIAN_POINT('Origin',(7.13137084989848,-1.13137084989848,15.1));
#30525=CARTESIAN_POINT('Origin',(6.,0.,11.5));
#30526=CARTESIAN_POINT('',(4.5,-1.83697019872103E-16,14.6));
#30527=CARTESIAN_POINT('Origin',(6.,0.,14.6));
#30528=CARTESIAN_POINT('',(4.5,-1.83697019872103E-16,11.5));
#30529=CARTESIAN_POINT('',(4.5,-1.83697019872103E-16,11.5));
#30530=CARTESIAN_POINT('Origin',(6.,0.,11.5));
#30531=CARTESIAN_POINT('Origin',(6.,0.,14.6));
#30532=CARTESIAN_POINT('Origin',(6.,0.,14.6));
#30533=CARTESIAN_POINT('Origin',(6.,0.,14.6));
#30534=CARTESIAN_POINT('Origin',(6.,0.,14.6));
#30535=CARTESIAN_POINT('Origin',(6.,0.,12.1));
#30536=CARTESIAN_POINT('',(4.95,-1.28587913910472E-16,12.1));
#30537=CARTESIAN_POINT('Origin',(6.,0.,12.1));
#30538=CARTESIAN_POINT('',(4.95,1.28587913910472E-16,15.1));
#30539=CARTESIAN_POINT('',(4.95,-1.28587913910472E-16,12.1));
#30540=CARTESIAN_POINT('Origin',(6.,0.,15.1));
#30541=CARTESIAN_POINT('Origin',(6.,0.,12.1));
#30542=CARTESIAN_POINT('',(5.375,-7.65404249467096E-17,12.1));
#30543=CARTESIAN_POINT('Origin',(6.,0.,12.1));
#30544=CARTESIAN_POINT('Origin',(6.,0.,14.6));
#30545=CARTESIAN_POINT('',(4.,-2.44929359829471E-16,14.6));
#30546=CARTESIAN_POINT('Origin',(6.,0.,14.6));
#30547=CARTESIAN_POINT('Origin',(6.,0.,14.6));
#30548=CARTESIAN_POINT('',(4.,-2.44929359829471E-16,15.1));
#30549=CARTESIAN_POINT('Origin',(6.,0.,15.1));
#30550=CARTESIAN_POINT('',(4.,-2.44929359829471E-16,14.6));
#30551=CARTESIAN_POINT('Origin',(6.,0.,11.5));
#30552=CARTESIAN_POINT('',(5.375,-7.65404249467096E-17,11.5));
#30553=CARTESIAN_POINT('',(5.375,-7.65404249467096E-17,11.5));
#30554=CARTESIAN_POINT('Origin',(6.,0.,11.5));
#30555=CARTESIAN_POINT('Origin',(6.,0.,15.1));
#30556=CARTESIAN_POINT('Origin',(6.,0.,11.5));
#30557=CARTESIAN_POINT('',(0.,0.,0.));
#30558=CARTESIAN_POINT('Origin',(0.,3.5,12.8));
#30559=CARTESIAN_POINT('',(-0.165,3.5,12.8));
#30560=CARTESIAN_POINT('Origin',(0.,3.5,12.8));
#30561=CARTESIAN_POINT('',(-0.165,3.5,14.5));
#30562=CARTESIAN_POINT('',(-0.165,3.5,12.8));
#30563=CARTESIAN_POINT('Origin',(0.,3.5,14.5));
#30564=CARTESIAN_POINT('Origin',(0.,3.5,12.8));
#30565=CARTESIAN_POINT('Origin',(0.,6.5,12.8));
#30566=CARTESIAN_POINT('',(-0.165,6.5,12.8));
#30567=CARTESIAN_POINT('Origin',(0.,6.5,12.8));
#30568=CARTESIAN_POINT('',(-0.165,6.5,14.5));
#30569=CARTESIAN_POINT('',(-0.165,6.5,12.8));
#30570=CARTESIAN_POINT('Origin',(0.,6.5,14.5));
#30571=CARTESIAN_POINT('Origin',(0.,6.5,12.8));
#30572=CARTESIAN_POINT('Origin',(-1.5,5.,12.8));
#30573=CARTESIAN_POINT('',(-1.665,5.,12.8));
#30574=CARTESIAN_POINT('Origin',(-1.5,5.,12.8));
#30575=CARTESIAN_POINT('',(-1.665,5.,14.5));
#30576=CARTESIAN_POINT('',(-1.665,5.,12.8));
#30577=CARTESIAN_POINT('Origin',(-1.5,5.,14.5));
#30578=CARTESIAN_POINT('Origin',(-1.5,5.,12.8));
#30579=CARTESIAN_POINT('Origin',(0.,5.,12.5));
#30580=CARTESIAN_POINT('',(-1.11,5.,14.5));
#30581=CARTESIAN_POINT('Origin',(0.,5.,14.5));
#30582=CARTESIAN_POINT('',(-1.11,5.,12.5));
#30583=CARTESIAN_POINT('',(-1.11,5.,12.5));
#30584=CARTESIAN_POINT('Origin',(0.,5.,12.5));
#30585=CARTESIAN_POINT('Origin',(0.,5.,12.5));
#30586=CARTESIAN_POINT('',(-2.2,5.,14.5));
#30587=CARTESIAN_POINT('Origin',(0.,5.,14.5));
#30588=CARTESIAN_POINT('',(-2.2,5.,12.5));
#30589=CARTESIAN_POINT('',(-2.2,5.,12.5));
#30590=CARTESIAN_POINT('Origin',(0.,5.,12.5));
#30591=CARTESIAN_POINT('Origin',(0.,5.,14.5));
#30592=CARTESIAN_POINT('Origin',(0.,5.,12.5));
#30593=CARTESIAN_POINT('',(0.,0.,0.));
#30594=CARTESIAN_POINT('Origin',(-2.,-1.5,14.5));
#30595=CARTESIAN_POINT('',(-2.165,-1.5,14.6));
#30596=CARTESIAN_POINT('Origin',(-2.,-1.5,14.6));
#30597=CARTESIAN_POINT('',(-2.165,-1.5,15.1));
#30598=CARTESIAN_POINT('',(-2.165,-1.5,14.5));
#30599=CARTESIAN_POINT('Origin',(-2.,-1.5,15.1));
#30600=CARTESIAN_POINT('Origin',(2.,-1.5,14.5));
#30601=CARTESIAN_POINT('',(1.835,-1.5,14.6));
#30602=CARTESIAN_POINT('Origin',(2.,-1.5,14.6));
#30603=CARTESIAN_POINT('',(1.835,-1.5,15.1));
#30604=CARTESIAN_POINT('',(1.835,-1.5,14.5));
#30605=CARTESIAN_POINT('Origin',(2.,-1.5,15.1));
#30606=CARTESIAN_POINT('Origin',(0.,-1.5,14.6));
#30607=CARTESIAN_POINT('',(-3.,-1.5,15.1));
#30608=CARTESIAN_POINT('Origin',(0.,-1.5,15.1));
#30609=CARTESIAN_POINT('',(-3.,-1.5,14.6));
#30610=CARTESIAN_POINT('',(-3.,-1.5,14.6));
#30611=CARTESIAN_POINT('Origin',(0.,-1.5,14.6));
#30612=CARTESIAN_POINT('Origin',(0.,-1.5,15.1));
#30613=CARTESIAN_POINT('Origin',(0.,-1.5,14.6));
#30614=CARTESIAN_POINT('',(0.,0.,0.));
#30615=CARTESIAN_POINT('Origin',(7.2,-0.35,16.2));
#30616=CARTESIAN_POINT('',(6.975,-0.35,16.3));
#30617=CARTESIAN_POINT('Origin',(7.2,-0.35,16.3));
#30618=CARTESIAN_POINT('',(6.975,-0.35,16.7));
#30619=CARTESIAN_POINT('',(6.975,-0.35,16.2));
#30620=CARTESIAN_POINT('Origin',(7.2,-0.35,16.7));
#30621=CARTESIAN_POINT('Origin',(7.2,0.35,16.2));
#30622=CARTESIAN_POINT('',(6.975,0.35,16.3));
#30623=CARTESIAN_POINT('Origin',(7.2,0.35,16.3));
#30624=CARTESIAN_POINT('',(6.975,0.35,16.7));
#30625=CARTESIAN_POINT('',(6.975,0.35,16.2));
#30626=CARTESIAN_POINT('Origin',(7.2,0.35,16.7));
#30627=CARTESIAN_POINT('Origin',(8.65,0.,15.1));
#30628=CARTESIAN_POINT('',(8.65,0.,15.1));
#30629=CARTESIAN_POINT('',(8.,0.2,15.1));
#30630=CARTESIAN_POINT('',(8.65,0.,15.1));
#30631=CARTESIAN_POINT('',(8.,0.2,15.3));
#30632=CARTESIAN_POINT('',(8.,0.2,15.1));
#30633=CARTESIAN_POINT('',(8.65,0.,15.3));
#30634=CARTESIAN_POINT('',(8.65,0.,15.3));
#30635=CARTESIAN_POINT('',(8.65,0.,15.1));
#30636=CARTESIAN_POINT('Origin',(8.,-0.2,15.1));
#30637=CARTESIAN_POINT('',(8.,-0.2,15.1));
#30638=CARTESIAN_POINT('',(8.,-0.2,15.1));
#30639=CARTESIAN_POINT('',(8.,-0.2,15.3));
#30640=CARTESIAN_POINT('',(8.,-0.2,15.3));
#30641=CARTESIAN_POINT('',(8.,-0.2,15.1));
#30642=CARTESIAN_POINT('Origin',(8.325,0.,15.3));
#30643=CARTESIAN_POINT('',(8.,-0.4,15.3));
#30644=CARTESIAN_POINT('Origin',(8.,0.75,16.3));
#30645=CARTESIAN_POINT('',(7.5,0.75,16.3));
#30646=CARTESIAN_POINT('',(7.5,0.75,16.7));
#30647=CARTESIAN_POINT('',(7.5,0.75,15.7));
#30648=CARTESIAN_POINT('',(6.7,0.75,16.3));
#30649=CARTESIAN_POINT('',(8.,0.75,16.3));
#30650=CARTESIAN_POINT('',(6.7,0.75,16.7));
#30651=CARTESIAN_POINT('',(6.7,0.75,16.3));
#30652=CARTESIAN_POINT('',(8.,0.75,16.7));
#30653=CARTESIAN_POINT('Origin',(7.35,0.,16.3));
#30654=CARTESIAN_POINT('',(7.5,-0.75,16.3));
#30655=CARTESIAN_POINT('',(7.5,0.4,16.3));
#30656=CARTESIAN_POINT('',(6.7,-0.75,16.3));
#30657=CARTESIAN_POINT('',(6.7,-0.75,16.3));
#30658=CARTESIAN_POINT('',(6.7,0.75,16.3));
#30659=CARTESIAN_POINT('Origin',(6.7,-0.75,16.3));
#30660=CARTESIAN_POINT('',(7.5,-0.75,16.7));
#30661=CARTESIAN_POINT('',(7.5,-0.75,15.7));
#30662=CARTESIAN_POINT('',(6.7,-0.75,16.7));
#30663=CARTESIAN_POINT('',(6.7,-0.75,16.7));
#30664=CARTESIAN_POINT('',(6.7,-0.75,16.3));
#30665=CARTESIAN_POINT('Origin',(6.7,0.75,16.3));
#30666=CARTESIAN_POINT('',(6.7,0.75,16.7));
#30667=CARTESIAN_POINT('Origin',(8.,-0.8,15.1));
#30668=CARTESIAN_POINT('',(8.,0.8,15.1));
#30669=CARTESIAN_POINT('',(8.,-0.8,15.1));
#30670=CARTESIAN_POINT('',(8.,0.8,16.7));
#30671=CARTESIAN_POINT('',(8.,0.8,15.1));
#30672=CARTESIAN_POINT('',(8.,-0.8,16.7));
#30673=CARTESIAN_POINT('',(8.,-0.8,16.7));
#30674=CARTESIAN_POINT('',(8.,-0.8,15.1));
#30675=CARTESIAN_POINT('',(8.,-0.8,15.1));
#30676=CARTESIAN_POINT('',(8.,-0.8,15.1));
#30677=CARTESIAN_POINT('Origin',(8.,0.8,15.1));
#30678=CARTESIAN_POINT('',(7.5,0.8,15.1));
#30679=CARTESIAN_POINT('',(8.,0.8,15.1));
#30680=CARTESIAN_POINT('',(7.5,0.8,16.7));
#30681=CARTESIAN_POINT('',(7.5,0.8,15.1));
#30682=CARTESIAN_POINT('',(8.,0.8,16.7));
#30683=CARTESIAN_POINT('Origin',(7.5,-0.8,15.1));
#30684=CARTESIAN_POINT('',(7.5,-0.8,15.1));
#30685=CARTESIAN_POINT('',(7.5,-0.8,15.1));
#30686=CARTESIAN_POINT('',(7.5,-0.8,16.7));
#30687=CARTESIAN_POINT('',(7.5,-0.8,16.7));
#30688=CARTESIAN_POINT('',(7.5,-0.8,15.1));
#30689=CARTESIAN_POINT('Origin',(7.5,0.8,15.1));
#30690=CARTESIAN_POINT('',(7.5,0.8,16.7));
#30691=CARTESIAN_POINT('',(7.5,0.8,15.1));
#30692=CARTESIAN_POINT('',(7.5,0.8,16.7));
#30693=CARTESIAN_POINT('Origin',(7.75,0.,16.7));
#30694=CARTESIAN_POINT('Origin',(7.75,0.,15.1));
#30695=CARTESIAN_POINT('',(0.,0.,0.));
#30696=CARTESIAN_POINT('',(0.,0.,0.));
#30697=CARTESIAN_POINT('Origin',(0.75,1.2,0.));
#30698=CARTESIAN_POINT('',(0.885663593019381,1.2,-0.16));
#30699=CARTESIAN_POINT('',(0.885663593019381,1.2,0.16));
#30700=CARTESIAN_POINT('Origin',(0.,1.2,0.));
#30701=CARTESIAN_POINT('',(0.93,1.2,-0.16));
#30702=CARTESIAN_POINT('',(0.93,1.2,-0.16));
#30703=CARTESIAN_POINT('',(0.93,1.2,0.16));
#30704=CARTESIAN_POINT('',(0.93,1.2,0.16));
#30705=CARTESIAN_POINT('',(0.57,1.2,0.16));
#30706=CARTESIAN_POINT('Origin',(0.57,0.,0.16));
#30707=CARTESIAN_POINT('',(0.885663593019381,-1.2,0.16));
#30708=CARTESIAN_POINT('',(0.885663593019381,0.,0.16));
#30709=CARTESIAN_POINT('',(0.93,-1.2,0.16));
#30710=CARTESIAN_POINT('',(0.93,0.,0.16));
#30711=CARTESIAN_POINT('',(0.57,-1.2,0.16));
#30712=CARTESIAN_POINT('Origin',(0.75,-1.2,0.));
#30713=CARTESIAN_POINT('',(0.885663593019381,-1.2,-0.16));
#30714=CARTESIAN_POINT('Origin',(0.,-1.2,0.));
#30715=CARTESIAN_POINT('',(0.93,-1.2,-0.16));
#30716=CARTESIAN_POINT('',(0.93,-1.2,0.16));
#30717=CARTESIAN_POINT('',(0.93,-1.2,-0.16));
#30718=CARTESIAN_POINT('Origin',(0.93,0.,-0.16));
#30719=CARTESIAN_POINT('',(0.885663593019381,0.,-0.16));
#30720=CARTESIAN_POINT('',(0.93,0.,-0.16));
#30721=CARTESIAN_POINT('Origin',(0.93,0.,0.16));
#30722=CARTESIAN_POINT('Origin',(1.05,1.5,0.));
#30723=CARTESIAN_POINT('',(-1.05,1.5,-1.28587913910472E-16));
#30724=CARTESIAN_POINT('Origin',(0.,1.5,0.));
#30725=CARTESIAN_POINT('',(-0.9,1.5,-1.10218211923262E-16));
#30726=CARTESIAN_POINT('Origin',(0.,1.5,0.));
#30727=CARTESIAN_POINT('Origin',(0.,1.315,0.));
#30728=CARTESIAN_POINT('',(-1.05,1.13,-1.28587913910472E-16));
#30729=CARTESIAN_POINT('Origin',(0.,1.13,0.));
#30730=CARTESIAN_POINT('',(-1.05,1.315,-1.28587913910472E-16));
#30731=CARTESIAN_POINT('Origin',(1.,1.13,0.));
#30732=CARTESIAN_POINT('',(-1.,1.13,-1.22464679914735E-16));
#30733=CARTESIAN_POINT('Origin',(0.,1.13,0.));
#30734=CARTESIAN_POINT('Origin',(0.,1.065,0.));
#30735=CARTESIAN_POINT('',(-1.,1.,-1.22464679914735E-16));
#30736=CARTESIAN_POINT('Origin',(0.,1.,0.));
#30737=CARTESIAN_POINT('',(-1.,1.065,-1.22464679914735E-16));
#30738=CARTESIAN_POINT('Origin',(1.05,1.,0.));
#30739=CARTESIAN_POINT('',(-1.05,1.,-1.28587913910472E-16));
#30740=CARTESIAN_POINT('Origin',(0.,1.,0.));
#30741=CARTESIAN_POINT('Origin',(0.,0.,0.));
#30742=CARTESIAN_POINT('',(-1.05,-1.,-1.28587913910472E-16));
#30743=CARTESIAN_POINT('Origin',(0.,-1.,0.));
#30744=CARTESIAN_POINT('',(-1.05,0.,-1.28587913910472E-16));
#30745=CARTESIAN_POINT('Origin',(1.,-1.,0.));
#30746=CARTESIAN_POINT('',(-1.,-1.,-1.22464679914735E-16));
#30747=CARTESIAN_POINT('Origin',(0.,-1.,0.));
#30748=CARTESIAN_POINT('Origin',(0.,-1.065,0.));
#30749=CARTESIAN_POINT('',(-1.,-1.13,-1.22464679914735E-16));
#30750=CARTESIAN_POINT('Origin',(0.,-1.13,0.));
#30751=CARTESIAN_POINT('',(-1.,-1.065,-1.22464679914735E-16));
#30752=CARTESIAN_POINT('Origin',(1.05,-1.13,0.));
#30753=CARTESIAN_POINT('',(-1.05,-1.13,-1.28587913910472E-16));
#30754=CARTESIAN_POINT('Origin',(0.,-1.13,0.));
#30755=CARTESIAN_POINT('Origin',(0.,-1.315,0.));
#30756=CARTESIAN_POINT('',(-1.05,-1.5,-1.28587913910472E-16));
#30757=CARTESIAN_POINT('Origin',(0.,-1.5,0.));
#30758=CARTESIAN_POINT('',(-1.05,-1.315,-1.28587913910472E-16));
#30759=CARTESIAN_POINT('Origin',(0.9,-1.5,0.));
#30760=CARTESIAN_POINT('',(-0.9,-1.5,-1.10218211923262E-16));
#30761=CARTESIAN_POINT('Origin',(0.,-1.5,0.));
#30762=CARTESIAN_POINT('Origin',(0.,0.,0.));
#30763=CARTESIAN_POINT('',(-0.9,0.,-1.10218211923262E-16));
#30764=CARTESIAN_POINT('',(0.,0.,0.));
#30765=CARTESIAN_POINT('Origin',(0.75,1.2,0.));
#30766=CARTESIAN_POINT('',(0.880582193778639,1.2,0.16));
#30767=CARTESIAN_POINT('',(0.880582193778639,1.2,-0.16));
#30768=CARTESIAN_POINT('Origin',(0.,1.2,0.));
#30769=CARTESIAN_POINT('',(0.583459510163302,1.2,0.16));
#30770=CARTESIAN_POINT('',(0.57,1.2,0.16));
#30771=CARTESIAN_POINT('',(0.583459510163302,1.2,-0.16));
#30772=CARTESIAN_POINT('Origin',(0.,1.2,0.));
#30773=CARTESIAN_POINT('',(0.93,1.2,-0.16));
#30774=CARTESIAN_POINT('Origin',(0.93,0.,-0.16));
#30775=CARTESIAN_POINT('',(0.880582193778639,-1.2,-0.16));
#30776=CARTESIAN_POINT('',(0.880582193778639,0.,-0.16));
#30777=CARTESIAN_POINT('',(0.583459510163302,-1.2,-0.16));
#30778=CARTESIAN_POINT('',(0.583459510163302,0.,-0.16));
#30779=CARTESIAN_POINT('',(0.93,-1.2,-0.16));
#30780=CARTESIAN_POINT('Origin',(0.75,-1.2,0.));
#30781=CARTESIAN_POINT('',(0.880582193778639,-1.2,0.16));
#30782=CARTESIAN_POINT('Origin',(0.,-1.2,0.));
#30783=CARTESIAN_POINT('',(0.583459510163302,-1.2,0.16));
#30784=CARTESIAN_POINT('Origin',(0.,-1.2,0.));
#30785=CARTESIAN_POINT('',(0.57,-1.2,0.16));
#30786=CARTESIAN_POINT('Origin',(0.57,0.,0.16));
#30787=CARTESIAN_POINT('',(0.880582193778639,0.,0.16));
#30788=CARTESIAN_POINT('',(0.583459510163302,0.,0.16));
#30789=CARTESIAN_POINT('Origin',(0.895,1.35,0.));
#30790=CARTESIAN_POINT('',(-0.895,1.35,-1.09605888523688E-16));
#30791=CARTESIAN_POINT('Origin',(0.,1.35,0.));
#30792=CARTESIAN_POINT('',(-0.605,1.35,-7.40911313484149E-17));
#30793=CARTESIAN_POINT('Origin',(0.,1.35,0.));
#30794=CARTESIAN_POINT('Origin',(0.,0.,0.));
#30795=CARTESIAN_POINT('',(-0.895,-1.35,-1.09605888523688E-16));
#30796=CARTESIAN_POINT('Origin',(0.,-1.35,0.));
#30797=CARTESIAN_POINT('',(-0.895,0.,-1.09605888523688E-16));
#30798=CARTESIAN_POINT('Origin',(0.605,-1.35,0.));
#30799=CARTESIAN_POINT('',(-0.605,-1.35,-7.40911313484149E-17));
#30800=CARTESIAN_POINT('Origin',(0.,-1.35,0.));
#30801=CARTESIAN_POINT('Origin',(0.,0.,0.));
#30802=CARTESIAN_POINT('',(-0.605,0.,-7.40911313484149E-17));
#30803=CARTESIAN_POINT('',(0.,0.,0.));
#30804=CARTESIAN_POINT('',(0.,0.,0.));
#30805=CARTESIAN_POINT('',(0.,0.,0.));
#30806=CARTESIAN_POINT('Origin',(12.5,0.,4.));
#30807=CARTESIAN_POINT('',(12.7800042915148,-1.13874042544416E-5,4.45787212683272));
#30808=CARTESIAN_POINT('',(12.6699957084852,1.09516003635735E-5,4.45788309353564));
#30809=CARTESIAN_POINT('',(12.5,-5.60735153159594E-17,4.457875));
#30810=CARTESIAN_POINT('',(12.5,-0.186196943290586,3.58169363627331));
#30811=CARTESIAN_POINT('Ctrl Pts',(12.6699957084852,1.09516003635735E-5,
4.45788309353564));
#30812=CARTESIAN_POINT('Ctrl Pts',(12.6684300766731,0.0150239422001319,
4.45789815019349));
#30813=CARTESIAN_POINT('Ctrl Pts',(12.6668644448611,0.0300354905662504,
4.45717403092565));
#30814=CARTESIAN_POINT('Ctrl Pts',(12.6652988130491,0.0449730203321769,
4.45569984746698));
#30815=CARTESIAN_POINT('Ctrl Pts',(12.6574274409991,0.120072959788606,4.44828824124903));
#30816=CARTESIAN_POINT('Ctrl Pts',(12.6495560689492,0.193301947984492,4.42191743369942));
#30817=CARTESIAN_POINT('Ctrl Pts',(12.6416846968992,0.255884660534875,4.37974732787395));
#30818=CARTESIAN_POINT('Ctrl Pts',(12.6338133248492,0.318467373085258,4.33757722204849));
#30819=CARTESIAN_POINT('Ctrl Pts',(12.6259419527993,0.370403809990138,4.27960781794716));
#30820=CARTESIAN_POINT('Ctrl Pts',(12.6180705807493,0.405471379329245,4.2127856577826));
#30821=CARTESIAN_POINT('Ctrl Pts',(12.6101992086994,0.440538948668352,4.14596349761803));
#30822=CARTESIAN_POINT('Ctrl Pts',(12.6023278366494,0.458737650441686,4.07028858139023));
#30823=CARTESIAN_POINT('Ctrl Pts',(12.5944564645995,0.457884906392306,3.99482861029462));
#30824=CARTESIAN_POINT('Ctrl Pts',(12.5865850925495,0.457032162342926,3.91936863919901));
#30825=CARTESIAN_POINT('Ctrl Pts',(12.5787137204996,0.437127972470831,3.84412361323559));
#30826=CARTESIAN_POINT('Ctrl Pts',(12.5708423484496,0.400561475243013,3.77811083326841));
#30827=CARTESIAN_POINT('Ctrl Pts',(12.5629709763996,0.363994978015195,3.71209805330123));
#30828=CARTESIAN_POINT('Ctrl Pts',(12.5550996043497,0.310766173431653,3.6553175193303));
#30829=CARTESIAN_POINT('Ctrl Pts',(12.5472282322997,0.247245050961511,3.61457214242492));
#30830=CARTESIAN_POINT('Ctrl Pts',(12.5393568602498,0.183723928491369,3.57382676551955));
#30831=CARTESIAN_POINT('Ctrl Pts',(12.5314854881998,0.109910488134627,3.54911654567973));
#30832=CARTESIAN_POINT('Ctrl Pts',(12.5236141161499,0.034670519197381,3.5434092666393));
#30833=CARTESIAN_POINT('Ctrl Pts',(12.5157427440999,-0.0405694497398647,
3.53770198759887));
#30834=CARTESIAN_POINT('Ctrl Pts',(12.50787137205,-0.117235947257613,3.55099764935784));
#30835=CARTESIAN_POINT('Ctrl Pts',(12.5,-0.186196943290592,3.58169363627332));
#30836=CARTESIAN_POINT('',(12.5,-0.186217277007329,4.41832740439831));
#30837=CARTESIAN_POINT('Origin',(12.5,0.,4.));
#30838=CARTESIAN_POINT('Ctrl Pts',(12.5,-0.186217277007329,4.41832740439831));
#30839=CARTESIAN_POINT('Ctrl Pts',(12.5008157411716,-0.193365324225124,
4.41515241707318));
#30840=CARTESIAN_POINT('Ctrl Pts',(12.5016314823431,-0.200430783441492,
4.4117927098014));
#30841=CARTESIAN_POINT('Ctrl Pts',(12.5024472235147,-0.207403505574881,
4.40825058102053));
#30842=CARTESIAN_POINT('Ctrl Pts',(12.5103185955646,-0.274685741688951,
4.37407134077235));
#30843=CARTESIAN_POINT('Ctrl Pts',(12.5181899676146,-0.333333232193243,
4.32290684204764));
#30844=CARTESIAN_POINT('Ctrl Pts',(12.5260613396645,-0.376326743005614,
4.26088786252735));
#30845=CARTESIAN_POINT('Ctrl Pts',(12.5339327117145,-0.419320253817985,
4.19886888300706));
#30846=CARTESIAN_POINT('Ctrl Pts',(12.5418040837645,-0.446659784938435,
4.12599542269119));
#30847=CARTESIAN_POINT('Ctrl Pts',(12.5496754558144,-0.455065168373522,
4.05100019606997));
#30848=CARTESIAN_POINT('Ctrl Pts',(12.5575468278644,-0.463470551808608,
3.97600496944875));
#30849=CARTESIAN_POINT('Ctrl Pts',(12.5654181999143,-0.452941787558331,
3.89888797652218));
#30850=CARTESIAN_POINT('Ctrl Pts',(12.5732895719643,-0.424742400952558,
3.82888990513641));
#30851=CARTESIAN_POINT('Ctrl Pts',(12.5811609440142,-0.396543014346786,
3.75889183375065));
#30852=CARTESIAN_POINT('Ctrl Pts',(12.5890323160642,-0.350673005385519,
3.69601268390568));
#30853=CARTESIAN_POINT('Ctrl Pts',(12.5969036881141,-0.292628022669152,
3.64778723809593));
#30854=CARTESIAN_POINT('Ctrl Pts',(12.6047750601641,-0.234583039952784,
3.59956179228618));
#30855=CARTESIAN_POINT('Ctrl Pts',(12.6126464322141,-0.164363083481316,
3.56599005051166));
#30856=CARTESIAN_POINT('Ctrl Pts',(12.620517804264,-0.0903829156297007,
3.55109483330951));
#30857=CARTESIAN_POINT('Ctrl Pts',(12.628389176314,-0.0164027477780855,
3.53619961610736));
#30858=CARTESIAN_POINT('Ctrl Pts',(12.6362605483639,0.0613376314536766,
3.53998092347757));
#30859=CARTESIAN_POINT('Ctrl Pts',(12.6441319204139,0.13352290298843,3.56198566164487));
#30860=CARTESIAN_POINT('Ctrl Pts',(12.6520032924638,0.205708174523184,3.58399039981218));
#30861=CARTESIAN_POINT('Ctrl Pts',(12.6598746645138,0.272338338360929,3.62421856877658));
#30862=CARTESIAN_POINT('Ctrl Pts',(12.6677460365637,0.325429113408527,3.67784968145944));
#30863=CARTESIAN_POINT('Ctrl Pts',(12.6756174086137,0.378519888456125,3.7314807941423));
#30864=CARTESIAN_POINT('Ctrl Pts',(12.6834887806637,0.418071274713577,3.79851485054363));
#30865=CARTESIAN_POINT('Ctrl Pts',(12.6913601527136,0.439343931585728,3.87091926467948));
#30866=CARTESIAN_POINT('Ctrl Pts',(12.6992315247636,0.460616588457879,3.94332367881533));
#30867=CARTESIAN_POINT('Ctrl Pts',(12.7071028968135,0.46361051594473,4.02109845068571));
#30868=CARTESIAN_POINT('Ctrl Pts',(12.7149742688635,0.447966936692366,4.09492394607626));
#30869=CARTESIAN_POINT('Ctrl Pts',(12.7228456409134,0.432323357440003,4.16874944146681));
#30870=CARTESIAN_POINT('Ctrl Pts',(12.7307170129634,0.398042271448426,4.23862566037754));
#30871=CARTESIAN_POINT('Ctrl Pts',(12.7385883850133,0.349231538304918,4.29617944234672));
#30872=CARTESIAN_POINT('Ctrl Pts',(12.7464597570633,0.300420805161409,4.35373322431589));
#30873=CARTESIAN_POINT('Ctrl Pts',(12.7543311291133,0.237080424865968,4.39896456934351));
#30874=CARTESIAN_POINT('Ctrl Pts',(12.7622025011632,0.166800374688878,4.42645347375649));
#30875=CARTESIAN_POINT('Ctrl Pts',(12.7681364312804,0.113818899065861,4.4471763206439));
#30876=CARTESIAN_POINT('Ctrl Pts',(12.7740703613976,0.056893551674301,4.45781599184163));
#30877=CARTESIAN_POINT('Ctrl Pts',(12.7800042915148,-1.13874042544416E-5,
4.45787212683272));
#30878=CARTESIAN_POINT('Origin',(12.5,0.,4.));
#30879=CARTESIAN_POINT('',(13.0800042915148,2.8196954984682E-6,4.45783894202495));
#30880=CARTESIAN_POINT('',(12.9699957084852,-6.90274666573233E-6,4.45790451736119));
#30881=CARTESIAN_POINT('',(12.5,-5.60735153159594E-17,4.457875));
#30882=CARTESIAN_POINT('Ctrl Pts',(12.9699957084852,-6.90274666573233E-6,
4.45790451736119));
#30883=CARTESIAN_POINT('Ctrl Pts',(12.9628865412726,0.0681543496286777,
4.45785453236543));
#30884=CARTESIAN_POINT('Ctrl Pts',(12.95577737406,0.136337475731944,4.44242789501186));
#30885=CARTESIAN_POINT('Ctrl Pts',(12.9486682068475,0.197807532932104,4.41298560914613));
#30886=CARTESIAN_POINT('Ctrl Pts',(12.9407968347975,0.265868063186489,4.38038668734267));
#30887=CARTESIAN_POINT('Ctrl Pts',(12.9329254627476,0.325698883531032,4.33060565060516));
#30888=CARTESIAN_POINT('Ctrl Pts',(12.9250540906976,0.370130557623211,4.26960768492436));
#30889=CARTESIAN_POINT('Ctrl Pts',(12.9171827186476,0.41456223171539,4.20860971924356));
#30890=CARTESIAN_POINT('Ctrl Pts',(12.9093113465977,0.443594759555206,4.13639482461947));
#30891=CARTESIAN_POINT('Ctrl Pts',(12.9014399745477,0.453749217534713,4.06161640217293));
#30892=CARTESIAN_POINT('Ctrl Pts',(12.8935686024978,0.463903675514219,3.9868379797264));
#30893=CARTESIAN_POINT('Ctrl Pts',(12.8856972304478,0.455180063633418,3.90949602945742));
#30894=CARTESIAN_POINT('Ctrl Pts',(12.8778258583979,0.428623718850503,3.83885831972366));
#30895=CARTESIAN_POINT('Ctrl Pts',(12.8699544863479,0.402067374067587,3.7682206099899));
#30896=CARTESIAN_POINT('Ctrl Pts',(12.862083114298,0.357678296382559,3.70428714079136));
#30897=CARTESIAN_POINT('Ctrl Pts',(12.854211742248,0.300775561959983,3.65471896268111));
#30898=CARTESIAN_POINT('Ctrl Pts',(12.846340370198,0.243872827537407,3.60515078457087));
#30899=CARTESIAN_POINT('Ctrl Pts',(12.8384689981481,0.174456436377283,3.56994789754891));
#30900=CARTESIAN_POINT('Ctrl Pts',(12.8305976260981,0.100844448250471,3.55332860992135));
#30901=CARTESIAN_POINT('Ctrl Pts',(12.8227262540482,0.0272324601236582,
3.53670932229378));
#30902=CARTESIAN_POINT('Ctrl Pts',(12.8148548819982,-0.0505751249698428,
3.53867363406062));
#30903=CARTESIAN_POINT('Ctrl Pts',(12.8069835099483,-0.123254740362562,
3.558986165072));
#30904=CARTESIAN_POINT('Ctrl Pts',(12.7991121378983,-0.195934355755281,
3.57929869608338));
#30905=CARTESIAN_POINT('Ctrl Pts',(12.7912407658484,-0.263486001447217,
3.6179594463393));
#30906=CARTESIAN_POINT('Ctrl Pts',(12.7833693937984,-0.317815070570116,
3.67033575613656));
#30907=CARTESIAN_POINT('Ctrl Pts',(12.7754980217484,-0.372144139693014,
3.72271206593382));
#30908=CARTESIAN_POINT('Ctrl Pts',(12.7676266496985,-0.413250632246875,
3.78880393527241));
#30909=CARTESIAN_POINT('Ctrl Pts',(12.7597552776485,-0.43620881068128,3.86069167744737));
#30910=CARTESIAN_POINT('Ctrl Pts',(12.7518839055986,-0.459166989115684,
3.93257941962233));
#30911=CARTESIAN_POINT('Ctrl Pts',(12.7440125335486,-0.463976853430633,
4.01026303463365));
#30912=CARTESIAN_POINT('Ctrl Pts',(12.7361411614987,-0.450062064178823,
4.08443380953254));
#30913=CARTESIAN_POINT('Ctrl Pts',(12.7282697894487,-0.436147274927012,
4.15860458443143));
#30914=CARTESIAN_POINT('Ctrl Pts',(12.7203984173988,-0.403507832108441,
4.22926251921788));
#30915=CARTESIAN_POINT('Ctrl Pts',(12.7125270453488,-0.356054829243877,
4.28794078818664));
#30916=CARTESIAN_POINT('Ctrl Pts',(12.7046556732988,-0.308601826379312,
4.3466190571554));
#30917=CARTESIAN_POINT('Ctrl Pts',(12.6967843012489,-0.246335263468753,
4.39331766030646));
#30918=CARTESIAN_POINT('Ctrl Pts',(12.6889129291989,-0.176716536654988,
4.42244075943884));
#30919=CARTESIAN_POINT('Ctrl Pts',(12.682607188961,-0.120945115332726,4.44577121528397));
#30920=CARTESIAN_POINT('Ctrl Pts',(12.6763014487231,-0.0604553842193124,
4.45782245132557));
#30921=CARTESIAN_POINT('Ctrl Pts',(12.6699957084852,1.09516003635735E-5,
4.45788309353564));
#30922=CARTESIAN_POINT('Ctrl Pts',(12.7800042915148,-1.13874042544416E-5,
4.45787212683272));
#30923=CARTESIAN_POINT('Ctrl Pts',(12.7819417334476,-0.0185909818676029,
4.45789045503738));
#30924=CARTESIAN_POINT('Ctrl Pts',(12.7838791753803,-0.0371684007279871,
4.45678053845584));
#30925=CARTESIAN_POINT('Ctrl Pts',(12.7858166173131,-0.0556056617636943,
4.45452496135198));
#30926=CARTESIAN_POINT('Ctrl Pts',(12.793687989363,-0.130511927980435,4.44536108073615));
#30927=CARTESIAN_POINT('Ctrl Pts',(12.801559361413,-0.203104740355178,4.41728685570614));
#30928=CARTESIAN_POINT('Ctrl Pts',(12.8094307334629,-0.264685413403174,
4.37366637792357));
#30929=CARTESIAN_POINT('Ctrl Pts',(12.8173021055129,-0.32626608645117,4.33004590014099));
#30930=CARTESIAN_POINT('Ctrl Pts',(12.8251734775629,-0.37683462017242,4.27087916960585));
#30931=CARTESIAN_POINT('Ctrl Pts',(12.8330448496128,-0.410331463567461,
4.20325604577686));
#30932=CARTESIAN_POINT('Ctrl Pts',(12.8409162216628,-0.443828306962503,
4.13563292194788));
#30933=CARTESIAN_POINT('Ctrl Pts',(12.8487875937127,-0.460253460031337,
4.05955340482505));
#30934=CARTESIAN_POINT('Ctrl Pts',(12.8566589657627,-0.457638721839564,
3.98413398734005));
#30935=CARTESIAN_POINT('Ctrl Pts',(12.8645303378126,-0.45502398364779,3.90871456985506));
#30936=CARTESIAN_POINT('Ctrl Pts',(12.8724017098626,-0.433369354195409,
3.8339552520079));
#30937=CARTESIAN_POINT('Ctrl Pts',(12.8802730819125,-0.395269674734573,
3.76881432927916));
#30938=CARTESIAN_POINT('Ctrl Pts',(12.8881444539625,-0.357169995273737,
3.70367340655041));
#30939=CARTESIAN_POINT('Ctrl Pts',(12.8960158260125,-0.302625265804445,
3.64815087894007));
#30940=CARTESIAN_POINT('Ctrl Pts',(12.9038871980624,-0.238171498431664,
3.6088999265713));
#30941=CARTESIAN_POINT('Ctrl Pts',(12.9117585701124,-0.173717731058884,
3.56964897420252));
#30942=CARTESIAN_POINT('Ctrl Pts',(12.9196299421623,-0.0993549257826154,
3.5466695970753));
#30943=CARTESIAN_POINT('Ctrl Pts',(12.9275013142123,-0.023993864556795,
3.54271537903906));
#30944=CARTESIAN_POINT('Ctrl Pts',(12.9353726862622,0.0513671966690251,
3.53876116100282));
#30945=CARTESIAN_POINT('Ctrl Pts',(12.9432440583122,0.127726513844396,3.55383210205756));
#30946=CARTESIAN_POINT('Ctrl Pts',(12.9511154303621,0.195934065997641,3.58612227423372));
#30947=CARTESIAN_POINT('Ctrl Pts',(12.9589868024121,0.264141618150887,3.61841244640988));
#30948=CARTESIAN_POINT('Ctrl Pts',(12.9668581744621,0.324197405282005,3.66792184970745));
#30949=CARTESIAN_POINT('Ctrl Pts',(12.974729546512,0.368905033668178,3.72871784755079));
#30950=CARTESIAN_POINT('Ctrl Pts',(12.982600918562,0.41361266205435,3.78951384539413));
#30951=CARTESIAN_POINT('Ctrl Pts',(12.9904722906119,0.442972131695578,3.86159643778324));
#30952=CARTESIAN_POINT('Ctrl Pts',(12.9983436626619,0.453465341949404,3.93632807718928));
#30953=CARTESIAN_POINT('Ctrl Pts',(13.0062150347118,0.46395855220323,4.01105971659532));
#30954=CARTESIAN_POINT('Ctrl Pts',(13.0140864067618,0.455585503069655,4.0884404030183));
#30955=CARTESIAN_POINT('Ctrl Pts',(13.0219577788117,0.429349524305901,4.15919772637108));
#30956=CARTESIAN_POINT('Ctrl Pts',(13.0298291508617,0.403113545542148,4.22995504972387));
#30957=CARTESIAN_POINT('Ctrl Pts',(13.0377005229117,0.359014637148215,4.29408901000646));
#30958=CARTESIAN_POINT('Ctrl Pts',(13.0455718949616,0.302337104315659,4.34391453219887));
#30959=CARTESIAN_POINT('Ctrl Pts',(13.0534432670116,0.245659571483104,4.39374005439127));
#30960=CARTESIAN_POINT('Ctrl Pts',(13.0613146390615,0.176403414211925,4.4292571384935));
#30961=CARTESIAN_POINT('Ctrl Pts',(13.0691860111115,0.102867492605122,4.44620982627979));
#30962=CARTESIAN_POINT('Ctrl Pts',(13.0727921045793,0.0691786509558273,
4.45397632191734));
#30963=CARTESIAN_POINT('Ctrl Pts',(13.076398198047,0.0345915681853763,4.45784650391406));
#30964=CARTESIAN_POINT('Ctrl Pts',(13.0800042915148,2.8196954984682E-6,
4.45783894202495));
#30965=CARTESIAN_POINT('Origin',(12.5,0.,4.));
#30966=CARTESIAN_POINT('',(13.3800042915148,1.00338821889499E-5,4.45789143379912));
#30967=CARTESIAN_POINT('',(13.2699957084852,-6.83105689078257E-6,4.45784477598907));
#30968=CARTESIAN_POINT('',(12.5,-5.60735153159594E-17,4.457875));
#30969=CARTESIAN_POINT('Ctrl Pts',(13.2699957084852,-6.83105689078257E-6,
4.45784477598907));
#30970=CARTESIAN_POINT('Ctrl Pts',(13.265214377922,0.0458528260712244,4.45782008288951));
#30971=CARTESIAN_POINT('Ctrl Pts',(13.2604330473589,0.091719698604501,4.45096974854549));
#30972=CARTESIAN_POINT('Ctrl Pts',(13.2556517167957,0.135506404234727,4.43740478719402));
#30973=CARTESIAN_POINT('Ctrl Pts',(13.2477803447458,0.207591244700251,4.41507316710824));
#30974=CARTESIAN_POINT('Ctrl Pts',(13.2399089726958,0.274038390871736,4.37454348113122));
#30975=CARTESIAN_POINT('Ctrl Pts',(13.2320376006459,0.326885582178656,4.32067233995558));
#30976=CARTESIAN_POINT('Ctrl Pts',(13.2241662285959,0.379732773485576,4.26680119877995));
#30977=CARTESIAN_POINT('Ctrl Pts',(13.2162948565459,0.418980009927931,4.19958860240569));
#30978=CARTESIAN_POINT('Ctrl Pts',(13.208423484496,0.439924354792367,4.12708853413817));
#30979=CARTESIAN_POINT('Ctrl Pts',(13.200552112446,0.460868699656804,4.05458846587065));
#30980=CARTESIAN_POINT('Ctrl Pts',(13.1926807403961,0.463510152943321,3.97680092570987));
#30981=CARTESIAN_POINT('Ctrl Pts',(13.1848093683461,0.447532193317848,3.90304707640827));
#30982=CARTESIAN_POINT('Ctrl Pts',(13.1769379962962,0.431554233692375,3.82929322710668));
#30983=CARTESIAN_POINT('Ctrl Pts',(13.1690666242462,0.396956861154912,3.75957306866428));
#30984=CARTESIAN_POINT('Ctrl Pts',(13.1611952521963,0.347885826291745,3.70224106173923));
#30985=CARTESIAN_POINT('Ctrl Pts',(13.1533238801463,0.298814791428577,3.64490905481418));
#30986=CARTESIAN_POINT('Ctrl Pts',(13.1454525080963,0.235270094239705,3.59996519940648));
#30987=CARTESIAN_POINT('Ctrl Pts',(13.1375811360464,0.164866199243897,3.57279504942506));
#30988=CARTESIAN_POINT('Ctrl Pts',(13.1297097639964,0.0944623042480882,
3.54562489944363));
#30989=CARTESIAN_POINT('Ctrl Pts',(13.1218383919465,0.0171992114453437,
3.53622845488849));
#30990=CARTESIAN_POINT('Ctrl Pts',(13.1139670198965,-0.0576647601420857,
3.54573167743434));
#30991=CARTESIAN_POINT('Ctrl Pts',(13.1060956478466,-0.132528731729515,
3.55523489998019));
#30992=CARTESIAN_POINT('Ctrl Pts',(13.0982242757966,-0.204993582101629,
3.58363778962703));
#30993=CARTESIAN_POINT('Ctrl Pts',(13.0903529037467,-0.266375958336211,
3.62753687126191));
#30994=CARTESIAN_POINT('Ctrl Pts',(13.0824815316967,-0.327758334570793,
3.67143595289679));
#30995=CARTESIAN_POINT('Ctrl Pts',(13.0746101596467,-0.378058236667844,
3.73083122651971));
#30996=CARTESIAN_POINT('Ctrl Pts',(13.0667387875968,-0.411248303781717,
3.79860544673343));
#30997=CARTESIAN_POINT('Ctrl Pts',(13.0588674155468,-0.444438370895591,
3.86637966694714));
#30998=CARTESIAN_POINT('Ctrl Pts',(13.0509960434969,-0.460518603026287,
3.94253283375165));
#30999=CARTESIAN_POINT('Ctrl Pts',(13.0431246714469,-0.457562130387816,
4.0179396288708));
#31000=CARTESIAN_POINT('Ctrl Pts',(13.035253299397,-0.454605657749345,4.09334642398995));
#31001=CARTESIAN_POINT('Ctrl Pts',(13.027381927347,-0.432612480341706,4.16800684742375));
#31002=CARTESIAN_POINT('Ctrl Pts',(13.0195105552971,-0.394218007200806,
4.23297445406563));
#31003=CARTESIAN_POINT('Ctrl Pts',(13.0116391832471,-0.355823534059905,
4.29794206070751));
#31004=CARTESIAN_POINT('Ctrl Pts',(13.0037678111972,-0.301027765185743,
4.35321685055749));
#31005=CARTESIAN_POINT('Ctrl Pts',(12.9958964391472,-0.236396794305188,
4.39217532952931));
#31006=CARTESIAN_POINT('Ctrl Pts',(12.9880250670972,-0.171765823424632,
4.43113380850113));
#31007=CARTESIAN_POINT('Ctrl Pts',(12.9801536950473,-0.0972996505376846,
4.45377597659478));
#31008=CARTESIAN_POINT('Ctrl Pts',(12.9722823229973,-0.0219214440120968,
4.4573886572069));
#31009=CARTESIAN_POINT('Ctrl Pts',(12.9715201181599,-0.014622381881285,
4.45773848219561));
#31010=CARTESIAN_POINT('Ctrl Pts',(12.9707579133226,-0.00731476803234869,
4.45790987647069));
#31011=CARTESIAN_POINT('Ctrl Pts',(12.9699957084852,-6.90274666573233E-6,
4.45790451736119));
#31012=CARTESIAN_POINT('Ctrl Pts',(13.0800042915148,2.8196954984682E-6,
4.45783894202495));
#31013=CARTESIAN_POINT('Ctrl Pts',(13.084269570097,-0.0409086678841046,
4.4578299978409));
#31014=CARTESIAN_POINT('Ctrl Pts',(13.0885348486792,-0.0818224858219862,
4.45239605085009));
#31015=CARTESIAN_POINT('Ctrl Pts',(13.0928001272613,-0.121255029803553,
4.44156782927524));
#31016=CARTESIAN_POINT('Ctrl Pts',(13.1006714993113,-0.194025944662995,
4.42158485301405));
#31017=CARTESIAN_POINT('Ctrl Pts',(13.1085428713613,-0.261752088439453,
4.3832306090213));
#31018=CARTESIAN_POINT('Ctrl Pts',(13.1164142434112,-0.31631794022257,4.33110102808186));
#31019=CARTESIAN_POINT('Ctrl Pts',(13.1242856154612,-0.370883792005687,
4.27897144714243));
#31020=CARTESIAN_POINT('Ctrl Pts',(13.1321569875111,-0.412289351795463,
4.21306652925631));
#31021=CARTESIAN_POINT('Ctrl Pts',(13.1400283595611,-0.435573054271055,
4.14128356060242));
#31022=CARTESIAN_POINT('Ctrl Pts',(13.147899731611,-0.458856756746647,4.06950059194853));
#31023=CARTESIAN_POINT('Ctrl Pts',(13.155771103661,-0.464018601908056,3.99183957252686));
#31024=CARTESIAN_POINT('Ctrl Pts',(13.1636424757109,-0.45044005369213,3.91760650430194));
#31025=CARTESIAN_POINT('Ctrl Pts',(13.1715138477609,-0.436861505476204,
3.84337343607703));
#31026=CARTESIAN_POINT('Ctrl Pts',(13.1793852198109,-0.404542563882944,
3.77256831904885));
#31027=CARTESIAN_POINT('Ctrl Pts',(13.1872565918608,-0.357355958580309,
3.7136756228145));
#31028=CARTESIAN_POINT('Ctrl Pts',(13.1951279639108,-0.310169353277673,
3.65478292658016));
#31029=CARTESIAN_POINT('Ctrl Pts',(13.2029993359607,-0.248115084265664,
3.60780265113964));
#31030=CARTESIAN_POINT('Ctrl Pts',(13.2108707080107,-0.178629020319019,
3.57836437152041));
#31031=CARTESIAN_POINT('Ctrl Pts',(13.2187420800606,-0.109142956372374,
3.54892609190117));
#31032=CARTESIAN_POINT('Ctrl Pts',(13.2266134521106,-0.0322250974910928,
3.53702980810322));
#31033=CARTESIAN_POINT('Ctrl Pts',(13.2344848241605,0.0429076061587562,
3.54410103373967));
#31034=CARTESIAN_POINT('Ctrl Pts',(13.2423561962105,0.118040309808605,3.55117225937612));
#31035=CARTESIAN_POINT('Ctrl Pts',(13.2502275682605,0.191387858227023,3.57721099444696));
#31036=CARTESIAN_POINT('Ctrl Pts',(13.2580989403104,0.254161126126225,3.61909705689013));
#31037=CARTESIAN_POINT('Ctrl Pts',(13.2659703123604,0.316934394025428,3.66098311933329));
#31038=CARTESIAN_POINT('Ctrl Pts',(13.2738416844103,0.369133381405416,3.71871650914877));
#31039=CARTESIAN_POINT('Ctrl Pts',(13.2817130564603,0.404503162915977,3.78537912195109));
#31040=CARTESIAN_POINT('Ctrl Pts',(13.2895844285102,0.43987294442654,3.85204173475342));
#31041=CARTESIAN_POINT('Ctrl Pts',(13.2974558005602,0.458413520067676,3.92763357054259));
#31042=CARTESIAN_POINT('Ctrl Pts',(13.3053271726101,0.457903200829578,4.00309657448501));
#31043=CARTESIAN_POINT('Ctrl Pts',(13.3131985446601,0.457392881591479,4.07855957842742));
#31044=CARTESIAN_POINT('Ctrl Pts',(13.3210699167101,0.437831667474148,4.15389375052308));
#31045=CARTESIAN_POINT('Ctrl Pts',(13.32894128876,0.401563549045306,4.22007191138728));
#31046=CARTESIAN_POINT('Ctrl Pts',(13.33681266081,0.365295430616463,4.28625007225149));
#31047=CARTESIAN_POINT('Ctrl Pts',(13.3446840328599,0.31232040787611,4.34327222188425));
#31048=CARTESIAN_POINT('Ctrl Pts',(13.3525554049099,0.248986397312635,4.38430548273058));
#31049=CARTESIAN_POINT('Ctrl Pts',(13.3604267769598,0.185652386749161,4.42533874357692));
#31050=CARTESIAN_POINT('Ctrl Pts',(13.3682981490098,0.111959388362564,4.45038311563682));
#31051=CARTESIAN_POINT('Ctrl Pts',(13.3761695210597,0.0367379221854645,
4.45643756985705));
#31052=CARTESIAN_POINT('Ctrl Pts',(13.3774477778781,0.024522472144774,4.45742077168506));
#31053=CARTESIAN_POINT('Ctrl Pts',(13.3787260346965,0.0122667140672706,
4.45790318029249));
#31054=CARTESIAN_POINT('Ctrl Pts',(13.3800042915148,1.00338821889499E-5,
4.45789143379912));
#31055=CARTESIAN_POINT('Origin',(12.5,0.,4.));
#31056=CARTESIAN_POINT('',(13.6800042915148,-8.85210990424201E-6,4.45789764648838));
#31057=CARTESIAN_POINT('',(13.5699957084852,1.03170790782398E-5,4.4578580083501));
#31058=CARTESIAN_POINT('',(12.5,-5.60735153159594E-17,4.457875));
#31059=CARTESIAN_POINT('Ctrl Pts',(13.5699957084852,1.03170790782398E-5,
4.4578580083501));
#31060=CARTESIAN_POINT('Ctrl Pts',(13.5675422145714,0.0235408097699949,
4.45787795556699));
#31061=CARTESIAN_POINT('Ctrl Pts',(13.5650887206577,0.0470683081483061,
4.45609516914004));
#31062=CARTESIAN_POINT('Ctrl Pts',(13.562635226744,0.0703115975725277,4.45248338388903));
#31063=CARTESIAN_POINT('Ctrl Pts',(13.554763854694,0.144881409096958,4.44089594716616));
#31064=CARTESIAN_POINT('Ctrl Pts',(13.5468924826441,0.21652593236894,4.41048310506186));
#31065=CARTESIAN_POINT('Ctrl Pts',(13.5390211105941,0.276660113016528,4.36488918223832));
#31066=CARTESIAN_POINT('Ctrl Pts',(13.5311497385442,0.336794293664116,4.31929525941478));
#31067=CARTESIAN_POINT('Ctrl Pts',(13.5232783664942,0.385418131687311,4.25852025587201));
#31068=CARTESIAN_POINT('Ctrl Pts',(13.5154069944443,0.416705106451492,4.18984674794718));
#31069=CARTESIAN_POINT('Ctrl Pts',(13.5075356223943,0.447992081215673,4.12117324002235));
#31070=CARTESIAN_POINT('Ctrl Pts',(13.4996642503443,0.461942192720839,4.04460122771548));
#31071=CARTESIAN_POINT('Ctrl Pts',(13.4917928782944,0.456883820300162,3.96930621892307));
#31072=CARTESIAN_POINT('Ctrl Pts',(13.4839215062444,0.451825447879485,3.89401121013066));
#31073=CARTESIAN_POINT('Ctrl Pts',(13.4760501341945,0.427758591532965,3.81999320485271));
#31074=CARTESIAN_POINT('Ctrl Pts',(13.4681787621445,0.387567146091087,3.75612166820384));
#31075=CARTESIAN_POINT('Ctrl Pts',(13.4603073900946,0.347375700649209,3.69225013155497));
#31076=CARTESIAN_POINT('Ctrl Pts',(13.4524360180446,0.291059666111973,3.63852506353517));
#31077=CARTESIAN_POINT('Ctrl Pts',(13.4445646459947,0.225367307335285,3.60138425741911));
#31078=CARTESIAN_POINT('Ctrl Pts',(13.4366932739447,0.159674948558598,3.56424345130305));
#31079=CARTESIAN_POINT('Ctrl Pts',(13.4288219018947,0.0846062655424597,
3.54368690709073));
#31080=CARTESIAN_POINT('Ctrl Pts',(13.4209505298448,0.00915662451852634,
3.54217788424291));
#31081=CARTESIAN_POINT('Ctrl Pts',(13.4130791577948,-0.0662930165054059,
3.54066886139509));
#31082=CARTESIAN_POINT('Ctrl Pts',(13.4052077857449,-0.142123615537132,
3.55820735991178));
#31083=CARTESIAN_POINT('Ctrl Pts',(13.3973364136949,-0.209248507106454,
3.5926917681625));
#31084=CARTESIAN_POINT('Ctrl Pts',(13.389465041645,-0.276373398675776,3.62717617641322));
#31085=CARTESIAN_POINT('Ctrl Pts',(13.381593669595,-0.334792582782693,3.67860649439798));
#31086=CARTESIAN_POINT('Ctrl Pts',(13.3737222975451,-0.377505777353741,
3.74081990525232));
#31087=CARTESIAN_POINT('Ctrl Pts',(13.3658509254951,-0.420218971924789,
3.80303331610666));
#31088=CARTESIAN_POINT('Ctrl Pts',(13.3579795534451,-0.44722617695997,3.87602981983059));
#31089=CARTESIAN_POINT('Ctrl Pts',(13.3501081813952,-0.455291160112798,
3.95106235628872));
#31090=CARTESIAN_POINT('Ctrl Pts',(13.3422368093452,-0.463356143265626,
4.02609489274685));
#31091=CARTESIAN_POINT('Ctrl Pts',(13.3343654372953,-0.452478904536101,
4.10316346193917));
#31092=CARTESIAN_POINT('Ctrl Pts',(13.3264940652453,-0.423962846915058,
4.17303305431203));
#31093=CARTESIAN_POINT('Ctrl Pts',(13.3186226931954,-0.395446789294015,
4.24290264668488));
#31094=CARTESIAN_POINT('Ctrl Pts',(13.3107513211454,-0.349291912781453,
4.30557326223827));
#31095=CARTESIAN_POINT('Ctrl Pts',(13.3028799490955,-0.291028886105345,
4.35353517632783));
#31096=CARTESIAN_POINT('Ctrl Pts',(13.2950085770455,-0.232765859429236,
4.4014970904174));
#31097=CARTESIAN_POINT('Ctrl Pts',(13.2871372049956,-0.162394682589579,
4.43475030304313));
#31098=CARTESIAN_POINT('Ctrl Pts',(13.2792658329456,-0.0883478267899694,
4.44931013225873));
#31099=CARTESIAN_POINT('Ctrl Pts',(13.2761757914588,-0.059279469337623,
4.4550258417985));
#31100=CARTESIAN_POINT('Ctrl Pts',(13.273085749972,-0.0296446570187532,
4.45786073445524));
#31101=CARTESIAN_POINT('Ctrl Pts',(13.2699957084852,-6.83105689078257E-6,
4.45784477598907));
#31102=CARTESIAN_POINT('Ctrl Pts',(13.3800042915148,1.00338821889499E-5,
4.45789143379912));
#31103=CARTESIAN_POINT('Ctrl Pts',(13.3865974067464,-0.0632086430349686,
4.45783084661254));
#31104=CARTESIAN_POINT('Ctrl Pts',(13.393190521978,-0.12645185159805,4.44462381290384));
#31105=CARTESIAN_POINT('Ctrl Pts',(13.3997836372096,-0.184315051738561,
4.41918121595096));
#31106=CARTESIAN_POINT('Ctrl Pts',(13.4076550092596,-0.253396625517876,
4.3888058714441));
#31107=CARTESIAN_POINT('Ctrl Pts',(13.4155263813095,-0.314809839108902,
4.34099064604983));
#31108=CARTESIAN_POINT('Ctrl Pts',(13.4233977533595,-0.361195640434018,
4.28146516557999));
#31109=CARTESIAN_POINT('Ctrl Pts',(13.4312691254094,-0.407581441759134,
4.22193968511016));
#31110=CARTESIAN_POINT('Ctrl Pts',(13.4391404974594,-0.438939830818339,
4.15070394956476));
#31111=CARTESIAN_POINT('Ctrl Pts',(13.4470118695093,-0.451513179494438,
4.07629402890356));
#31112=CARTESIAN_POINT('Ctrl Pts',(13.4548832415593,-0.464086528170537,
4.00188410824235));
#31113=CARTESIAN_POINT('Ctrl Pts',(13.4627546136093,-0.457874836463529,
3.92430000246534));
#31114=CARTESIAN_POINT('Ctrl Pts',(13.4706259856592,-0.433622441953051,
3.85283849709185));
#31115=CARTESIAN_POINT('Ctrl Pts',(13.4784973577092,-0.409370047442573,
3.78137699171835));
#31116=CARTESIAN_POINT('Ctrl Pts',(13.4863687297591,-0.367076950128625,
3.71603808674838));
#31117=CARTESIAN_POINT('Ctrl Pts',(13.4942401018091,-0.311811067605128,
3.66465124389307));
#31118=CARTESIAN_POINT('Ctrl Pts',(13.502111473859,-0.25654518508163,3.61326440103776));
#31119=CARTESIAN_POINT('Ctrl Pts',(13.509982845909,-0.188306517348584,3.5758296202971));
#31120=CARTESIAN_POINT('Ctrl Pts',(13.5178542179589,-0.115272000283325,
3.55683265457144));
#31121=CARTESIAN_POINT('Ctrl Pts',(13.5257255900089,-0.0422374832180674,
3.53783568884578));
#31122=CARTESIAN_POINT('Ctrl Pts',(13.5335969620589,0.035592883179403,3.53727653813511));
#31123=CARTESIAN_POINT('Ctrl Pts',(13.5414683341088,0.108892804353757,3.55522220461956));
#31124=CARTESIAN_POINT('Ctrl Pts',(13.5493397061588,0.182192725528112,3.573167871104));
#31125=CARTESIAN_POINT('Ctrl Pts',(13.5572110782087,0.250962201479351,3.60961835478357));
#31126=CARTESIAN_POINT('Ctrl Pts',(13.5650824502587,0.306960690387823,3.66020584957927));
#31127=CARTESIAN_POINT('Ctrl Pts',(13.5729538223086,0.362959179296295,3.71079334437498));
#31128=CARTESIAN_POINT('Ctrl Pts',(13.5808251943586,0.406186681162,3.77551785028682));
#31129=CARTESIAN_POINT('Ctrl Pts',(13.5886965664085,0.431463310113251,3.84662352810933));
#31130=CARTESIAN_POINT('Ctrl Pts',(13.5965679384585,0.456739939064502,3.91772920593184));
#31131=CARTESIAN_POINT('Ctrl Pts',(13.6044393105085,0.464065695101298,3.99521605566501));
#31132=CARTESIAN_POINT('Ctrl Pts',(13.6123106825584,0.452562744007997,4.06979894583348));
#31133=CARTESIAN_POINT('Ctrl Pts',(13.6201820546084,0.441059792914696,4.14438183600196));
#31134=CARTESIAN_POINT('Ctrl Pts',(13.6280534266583,0.410728134691299,4.21606076660573));
#31135=CARTESIAN_POINT('Ctrl Pts',(13.6359247987083,0.365202365858889,4.27624656029457));
#31136=CARTESIAN_POINT('Ctrl Pts',(13.6437961707582,0.319676597026479,4.33643235398341));
#31137=CARTESIAN_POINT('Ctrl Pts',(13.6516675428082,0.258956717585058,4.38512501075732));
#31138=CARTESIAN_POINT('Ctrl Pts',(13.6595389148581,0.190318698434502,4.41648976353532));
#31139=CARTESIAN_POINT('Ctrl Pts',(13.666360707077,0.130832969391341,4.44367229602021));
#31140=CARTESIAN_POINT('Ctrl Pts',(13.6731824992959,0.065399948454096,4.45783988979956));
#31141=CARTESIAN_POINT('Ctrl Pts',(13.6800042915148,-8.85210990424201E-6,
4.45789764648838));
#31142=CARTESIAN_POINT('Origin',(12.5,0.,4.));
#31143=CARTESIAN_POINT('',(13.9800042915148,-4.68615130337092E-6,4.45784092071359));
#31144=CARTESIAN_POINT('',(13.8699957084852,1.23414887176878E-6,4.4579133809027));
#31145=CARTESIAN_POINT('',(12.5,-5.60735153159594E-17,4.457875));
#31146=CARTESIAN_POINT('Ctrl Pts',(13.8699957084852,1.23414887176878E-6,
4.4579133809027));
#31147=CARTESIAN_POINT('Ctrl Pts',(13.8698700512209,0.00120594270822336,
4.45791357044259));
#31148=CARTESIAN_POINT('Ctrl Pts',(13.8697443939566,0.00241064979645091,
4.45790891401425));
#31149=CARTESIAN_POINT('Ctrl Pts',(13.8696187366923,0.00361531855258033,
4.45789940262096));
#31150=CARTESIAN_POINT('Ctrl Pts',(13.8617473646423,0.0790776965455978,
4.45730359373015));
#31151=CARTESIAN_POINT('Ctrl Pts',(13.8538759925924,0.154389660535011,4.43765704798318));
#31152=CARTESIAN_POINT('Ctrl Pts',(13.8460046205424,0.22052669229976,4.40131398110731));
#31153=CARTESIAN_POINT('Ctrl Pts',(13.8381332484924,0.286663724064511,4.36497091423144));
#31154=CARTESIAN_POINT('Ctrl Pts',(13.8302618764425,0.343625823604597,4.31193132622667));
#31155=CARTESIAN_POINT('Ctrl Pts',(13.8223905043925,0.384587309076409,4.24855087033892));
#31156=CARTESIAN_POINT('Ctrl Pts',(13.8145191323426,0.42554879454822,4.18517041445118));
#31157=CARTESIAN_POINT('Ctrl Pts',(13.8066477602926,0.450509665951756,4.11144909068046));
#31158=CARTESIAN_POINT('Ctrl Pts',(13.7987763882427,0.456478899990553,4.03622081324714));
#31159=CARTESIAN_POINT('Ctrl Pts',(13.7909050161927,0.46244813402935,3.96099253581381));
#31160=CARTESIAN_POINT('Ctrl Pts',(13.7830336441427,0.449425730703409,3.88425730471787));
#31161=CARTESIAN_POINT('Ctrl Pts',(13.7751622720928,0.418972144817937,3.81521018611534));
#31162=CARTESIAN_POINT('Ctrl Pts',(13.7672909000428,0.388518558932466,3.74616306751281));
#31163=CARTESIAN_POINT('Ctrl Pts',(13.7594195279929,0.340633790487464,3.68480406140369));
#31164=CARTESIAN_POINT('Ctrl Pts',(13.7515481559429,0.281055798532888,3.6384857242654));
#31165=CARTESIAN_POINT('Ctrl Pts',(13.743676783893,0.221477806578313,3.59216738712712));
#31166=CARTESIAN_POINT('Ctrl Pts',(13.735805411843,0.150206591114165,3.56088971895966));
#31167=CARTESIAN_POINT('Ctrl Pts',(13.7279340397931,0.0757824736049535,
3.54840067521841));
#31168=CARTESIAN_POINT('Ctrl Pts',(13.7200626677431,0.00135835609574232,
3.53591163147717));
#31169=CARTESIAN_POINT('Ctrl Pts',(13.7121912956931,-0.0762186634585312,
3.54221121216214));
#31170=CARTESIAN_POINT('Ctrl Pts',(13.7043199236432,-0.14765264866984,3.56654454809098));
#31171=CARTESIAN_POINT('Ctrl Pts',(13.6964485515932,-0.219086633881149,
3.59087788401983));
#31172=CARTESIAN_POINT('Ctrl Pts',(13.6885771795433,-0.284377584749494,
3.63324497519255));
#31173=CARTESIAN_POINT('Ctrl Pts',(13.6807058074933,-0.335701785830877,
3.68856903744356));
#31174=CARTESIAN_POINT('Ctrl Pts',(13.6728344354434,-0.38702598691226,3.74389309969457));
#31175=CARTESIAN_POINT('Ctrl Pts',(13.6649630633934,-0.424383438206683,
3.81217413302386));
#31176=CARTESIAN_POINT('Ctrl Pts',(13.6570916913435,-0.443297653083863,
3.88523012494906));
#31177=CARTESIAN_POINT('Ctrl Pts',(13.6492203192935,-0.462211867961044,
3.95828611687427));
#31178=CARTESIAN_POINT('Ctrl Pts',(13.6413489472436,-0.462682846420982,
4.03611706739538));
#31179=CARTESIAN_POINT('Ctrl Pts',(13.6334775751936,-0.444654151830396,
4.10939661196244));
#31180=CARTESIAN_POINT('Ctrl Pts',(13.6256062031436,-0.42662545723981,4.18267615652949));
#31181=CARTESIAN_POINT('Ctrl Pts',(13.6177348310937,-0.3900970895987,4.25140429514248));
#31182=CARTESIAN_POINT('Ctrl Pts',(13.6098634590437,-0.339446187702822,
4.3073454393722));
#31183=CARTESIAN_POINT('Ctrl Pts',(13.6019920869938,-0.288795285806945,
4.36328658360191));
#31184=CARTESIAN_POINT('Ctrl Pts',(13.5941207149438,-0.224021849656302,
4.40644073344835));
#31185=CARTESIAN_POINT('Ctrl Pts',(13.5862493428939,-0.152887581692542,
4.43163679270085));
#31186=CARTESIAN_POINT('Ctrl Pts',(13.5808314647576,-0.103925749791867,
4.44897928111035));
#31187=CARTESIAN_POINT('Ctrl Pts',(13.5754135866214,-0.0519504158054226,
4.45781396031326));
#31188=CARTESIAN_POINT('Ctrl Pts',(13.5699957084852,1.03170790782398E-5,
4.4578580083501));
#31189=CARTESIAN_POINT('Ctrl Pts',(13.6800042915148,-8.85210990424201E-6,
4.45789764648838));
#31190=CARTESIAN_POINT('Ctrl Pts',(13.6810538713459,-0.010072447664127,
4.45790653275371));
#31191=CARTESIAN_POINT('Ctrl Pts',(13.6821034511769,-0.0201354698749596,
4.45758141170421));
#31192=CARTESIAN_POINT('Ctrl Pts',(13.683153031008,-0.0301761699425476,
4.45691829561871));
#31193=CARTESIAN_POINT('Ctrl Pts',(13.691024403058,-0.105476860309351,4.45194522614199));
#31194=CARTESIAN_POINT('Ctrl Pts',(13.6988957751079,-0.179522082183268,
4.42796223840642));
#31195=CARTESIAN_POINT('Ctrl Pts',(13.7067671471579,-0.24343910912634,4.38784317739428));
#31196=CARTESIAN_POINT('Ctrl Pts',(13.7146385192078,-0.307356136069411,
4.34772411638213));
#31197=CARTESIAN_POINT('Ctrl Pts',(13.7225098912578,-0.361144968081636,
4.2914689820934));
#31198=CARTESIAN_POINT('Ctrl Pts',(13.7303812633077,-0.398360171146024,
4.22581874179975));
#31199=CARTESIAN_POINT('Ctrl Pts',(13.7382526353577,-0.435575374210412,
4.1601685015061));
#31200=CARTESIAN_POINT('Ctrl Pts',(13.7461240074077,-0.456216948326962,
4.08512315520753));
#31201=CARTESIAN_POINT('Ctrl Pts',(13.7539953794576,-0.457811445030669,
4.00967527273228));
#31202=CARTESIAN_POINT('Ctrl Pts',(13.7618667515076,-0.459405941734377,
3.93422739025703));
#31203=CARTESIAN_POINT('Ctrl Pts',(13.7697381235575,-0.441953361025241,
3.85837697160509));
#31204=CARTESIAN_POINT('Ctrl Pts',(13.7776094956075,-0.407545019133394,
3.79121305720166));
#31205=CARTESIAN_POINT('Ctrl Pts',(13.7854808676574,-0.373136677241547,
3.72404914279823));
#31206=CARTESIAN_POINT('Ctrl Pts',(13.7933522397074,-0.321772574166988,
3.6655717326433));
#31207=CARTESIAN_POINT('Ctrl Pts',(13.8012236117573,-0.259607592342073,
3.6227880859492));
#31208=CARTESIAN_POINT('Ctrl Pts',(13.8090949838073,-0.19744261051716,3.5800044392551));
#31209=CARTESIAN_POINT('Ctrl Pts',(13.8169663558573,-0.124476749941891,
3.55291455602183));
#31210=CARTESIAN_POINT('Ctrl Pts',(13.8248377279072,-0.0494533988297167,
3.54476457579874));
#31211=CARTESIAN_POINT('Ctrl Pts',(13.8327090999572,0.0255699522824598,
3.53661459557564));
#31212=CARTESIAN_POINT('Ctrl Pts',(13.8405804720071,0.102650793931542,3.54740451836272));
#31213=CARTESIAN_POINT('Ctrl Pts',(13.8484518440571,0.172552645974024,3.57584140410587));
#31214=CARTESIAN_POINT('Ctrl Pts',(13.856323216107,0.242454498016503,3.60427828984902));
#31215=CARTESIAN_POINT('Ctrl Pts',(13.864194588157,0.305177360452382,3.65036213854823));
#31216=CARTESIAN_POINT('Ctrl Pts',(13.8720659602069,0.353205247972751,3.70857079263049));
#31217=CARTESIAN_POINT('Ctrl Pts',(13.8799373322569,0.40123313549312,3.76677944671275));
#31218=CARTESIAN_POINT('Ctrl Pts',(13.8878087043068,0.434566048097978,3.83711290617806));
#31219=CARTESIAN_POINT('Ctrl Pts',(13.8956800763568,0.44920975351361,3.9111432194385));
#31220=CARTESIAN_POINT('Ctrl Pts',(13.9035514484068,0.463853458929242,3.98517353269893));
#31221=CARTESIAN_POINT('Ctrl Pts',(13.9114228204567,0.459807957155645,4.06290069975448));
#31222=CARTESIAN_POINT('Ctrl Pts',(13.9192941925067,0.437558014523894,4.13501079227018));
#31223=CARTESIAN_POINT('Ctrl Pts',(13.9271655645566,0.415308071892144,4.20712088478587));
#31224=CARTESIAN_POINT('Ctrl Pts',(13.9350369366066,0.374853688402242,4.27361390276169));
#31225=CARTESIAN_POINT('Ctrl Pts',(13.9429083086565,0.321042451364188,4.32652208887851));
#31226=CARTESIAN_POINT('Ctrl Pts',(13.9507796807065,0.267231214326134,4.37943027499533));
#31227=CARTESIAN_POINT('Ctrl Pts',(13.9586510527564,0.200063123739928,4.41875362925314));
#31228=CARTESIAN_POINT('Ctrl Pts',(13.9665224248064,0.127586829849962,4.43978009385641));
#31229=CARTESIAN_POINT('Ctrl Pts',(13.9710163803759,0.086208370984788,4.45178460807712));
#31230=CARTESIAN_POINT('Ctrl Pts',(13.9755103359454,0.0430996806131821,
4.45782517307841));
#31231=CARTESIAN_POINT('Ctrl Pts',(13.9800042915148,-4.68615130337092E-6,
4.45784092071359));
#31232=CARTESIAN_POINT('Origin',(12.5,0.,4.));
#31233=CARTESIAN_POINT('',(14.2800042915148,1.11332528513013E-5,4.45786561359635));
#31234=CARTESIAN_POINT('',(14.1699957084852,-1.10604184835328E-5,4.4578646218584));
#31235=CARTESIAN_POINT('',(12.5,-5.60735153159594E-17,4.457875));
#31236=CARTESIAN_POINT('Ctrl Pts',(14.1699957084852,-1.10604184835328E-5,
4.4578646218584));
#31237=CARTESIAN_POINT('Ctrl Pts',(14.1643265158203,0.0543576752587709,
4.45781404039958));
#31238=CARTESIAN_POINT('Ctrl Pts',(14.1586573231555,0.108743966382031,4.44812254260427));
#31239=CARTESIAN_POINT('Ctrl Pts',(14.1529881304907,0.159684023833442,4.42916890146099));
#31240=CARTESIAN_POINT('Ctrl Pts',(14.1451167584407,0.230411580321883,4.40285278028461));
#31241=CARTESIAN_POINT('Ctrl Pts',(14.1372453863907,0.294495541512382,4.358681244225));
#31242=CARTESIAN_POINT('Ctrl Pts',(14.1293740143408,0.344256823700223,4.30194730133701));
#31243=CARTESIAN_POINT('Ctrl Pts',(14.1215026422908,0.394018105888063,4.24521335844902));
#31244=CARTESIAN_POINT('Ctrl Pts',(14.1136312702409,0.429456709073245,4.17591700873265));
#31245=CARTESIAN_POINT('Ctrl Pts',(14.1057598981909,0.446326079279053,4.10236192849032));
#31246=CARTESIAN_POINT('Ctrl Pts',(14.097888526141,0.46319544948486,4.02880684824799));
#31247=CARTESIAN_POINT('Ctrl Pts',(14.090017154091,0.461495586711293,3.95099303747972));
#31248=CARTESIAN_POINT('Ctrl Pts',(14.0821457820411,0.441430182931853,3.87824480690492));
#31249=CARTESIAN_POINT('Ctrl Pts',(14.0742744099911,0.421364779152413,3.80549657633012));
#31250=CARTESIAN_POINT('Ctrl Pts',(14.0664030379411,0.3829338343671,3.73781392594881));
#31251=CARTESIAN_POINT('Ctrl Pts',(14.0585316658912,0.330742470300218,3.68330716492384));
#31252=CARTESIAN_POINT('Ctrl Pts',(14.0506602938412,0.278551106233337,3.62880040389886));
#31253=CARTESIAN_POINT('Ctrl Pts',(14.0427889217913,0.212599322884887,3.58746953223022));
#31254=CARTESIAN_POINT('Ctrl Pts',(14.0349175497413,0.140790022250932,3.5642671654747));
#31255=CARTESIAN_POINT('Ctrl Pts',(14.0270461776914,0.0689807216169763,
3.54106479871918));
#31256=CARTESIAN_POINT('Ctrl Pts',(14.0191748056414,-0.00868609630248519,
3.53599093687678));
#31257=CARTESIAN_POINT('Ctrl Pts',(14.0113034335915,-0.0829037347177578,
3.5496535731032));
#31258=CARTESIAN_POINT('Ctrl Pts',(14.0034320615415,-0.15712137313303,3.56331620932962));
#31259=CARTESIAN_POINT('Ctrl Pts',(13.9955606894916,-0.227889832044114,
3.59571534362485));
#31260=CARTESIAN_POINT('Ctrl Pts',(13.9876893174416,-0.286729034540398,
3.64296863695132));
#31261=CARTESIAN_POINT('Ctrl Pts',(13.9798179453916,-0.345568237036683,
3.69022193027778));
#31262=CARTESIAN_POINT('Ctrl Pts',(13.9719465733417,-0.392478183118168,
3.75232938263547));
#31263=CARTESIAN_POINT('Ctrl Pts',(13.9640752012917,-0.421837725217638,
3.82184875237013));
#31264=CARTESIAN_POINT('Ctrl Pts',(13.9562038292418,-0.451197267317109,
3.8913681221048));
#31265=CARTESIAN_POINT('Ctrl Pts',(13.9483324571918,-0.463006405434566,
3.96829940921644));
#31266=CARTESIAN_POINT('Ctrl Pts',(13.9404610851419,-0.455850068491383,
4.04342405445454));
#31267=CARTESIAN_POINT('Ctrl Pts',(13.9325897130919,-0.448693731548199,
4.11854869969265));
#31268=CARTESIAN_POINT('Ctrl Pts',(13.924718341042,-0.422571919544373,4.19186670305722));
#31269=CARTESIAN_POINT('Ctrl Pts',(13.916846968992,-0.38061476952465,4.25459247959939));
#31270=CARTESIAN_POINT('Ctrl Pts',(13.908975596942,-0.338657619504927,4.31731825614156));
#31271=CARTESIAN_POINT('Ctrl Pts',(13.9011042248921,-0.280865131469307,
4.36945180586132));
#31272=CARTESIAN_POINT('Ctrl Pts',(13.8932328528421,-0.214162491453186,
4.40474604470388));
#31273=CARTESIAN_POINT('Ctrl Pts',(13.8854871380565,-0.148524681204106,
4.43947685223224));
#31274=CARTESIAN_POINT('Ctrl Pts',(13.8777414232708,-0.0742589286223064,
4.45790169736071));
#31275=CARTESIAN_POINT('Ctrl Pts',(13.8699957084852,1.23414887176878E-6,
4.4579133809027));
#31276=CARTESIAN_POINT('Ctrl Pts',(13.9800042915148,-4.68615130337092E-6,
4.45784092071359));
#31277=CARTESIAN_POINT('Ctrl Pts',(13.9833817079953,-0.0323996211791616,
4.45785275579335));
#31278=CARTESIAN_POINT('Ctrl Pts',(13.9867591244758,-0.064792114138131,
4.45446164082457));
#31279=CARTESIAN_POINT('Ctrl Pts',(13.9901365409563,-0.0964458636128916,
4.44764173788363));
#31280=CARTESIAN_POINT('Ctrl Pts',(13.9980079130062,-0.170217765992045,
4.43174734235885));
#31281=CARTESIAN_POINT('Ctrl Pts',(14.0058792850562,-0.239977073556624,
4.39722897636055));
#31282=CARTESIAN_POINT('Ctrl Pts',(14.0137506571061,-0.297364634468633,
4.34822292324149));
#31283=CARTESIAN_POINT('Ctrl Pts',(14.0216220291561,-0.354752195380644,
4.29921687012243));
#31284=CARTESIAN_POINT('Ctrl Pts',(14.0294934012061,-0.399768009640084,
4.23572312988262));
#31285=CARTESIAN_POINT('Ctrl Pts',(14.037364773256,-0.427017900618165,4.16535006094698));
#31286=CARTESIAN_POINT('Ctrl Pts',(14.045236145306,-0.454267791596245,4.09497699201134));
#31287=CARTESIAN_POINT('Ctrl Pts',(14.0531075173559,-0.463751759292965,
4.01772459437987));
#31288=CARTESIAN_POINT('Ctrl Pts',(14.0609788894059,-0.45433335426851,3.94284990548881));
#31289=CARTESIAN_POINT('Ctrl Pts',(14.0688502614558,-0.444914949244056,
3.86797521659775));
#31290=CARTESIAN_POINT('Ctrl Pts',(14.0767216335058,-0.416594171498428,
3.7954782364471));
#31291=CARTESIAN_POINT('Ctrl Pts',(14.0845930055557,-0.372764656800254,
3.7340461680214));
#31292=CARTESIAN_POINT('Ctrl Pts',(14.0924643776057,-0.328935142102078,
3.67261409959569));
#31293=CARTESIAN_POINT('Ctrl Pts',(14.1003357496557,-0.269596890451354,
3.62224694289495));
#31294=CARTESIAN_POINT('Ctrl Pts',(14.1082071217056,-0.201860314388951,
3.58898011778223));
#31295=CARTESIAN_POINT('Ctrl Pts',(14.1160784937556,-0.134123738326549,
3.55571329266952));
#31296=CARTESIAN_POINT('Ctrl Pts',(14.1239498658055,-0.0579888378524715,
3.53954679914483));
#31297=CARTESIAN_POINT('Ctrl Pts',(14.1318212378555,0.0174212575835846,
3.54241784356498));
#31298=CARTESIAN_POINT('Ctrl Pts',(14.1396926099054,0.0928313530196406,
3.54528888798513));
#31299=CARTESIAN_POINT('Ctrl Pts',(14.1475639819554,0.167516643417675,3.56719747035013));
#31300=CARTESIAN_POINT('Ctrl Pts',(14.1554353540053,0.232527703900953,3.60551831852155));
#31301=CARTESIAN_POINT('Ctrl Pts',(14.1633067260553,0.297538764384231,3.64383916669297));
#31302=CARTESIAN_POINT('Ctrl Pts',(14.1711780981053,0.352875594952755,3.69857228067082));
#31303=CARTESIAN_POINT('Ctrl Pts',(14.1790494701552,0.391907267274456,3.76315907456484));
#31304=CARTESIAN_POINT('Ctrl Pts',(14.1869208422052,0.430938939596158,3.82774586845886));
#31305=CARTESIAN_POINT('Ctrl Pts',(14.1947922142551,0.453665453671035,3.90218634226906));
#31306=CARTESIAN_POINT('Ctrl Pts',(14.2026635863051,0.45736352584659,3.97756040711846));
#31307=CARTESIAN_POINT('Ctrl Pts',(14.210534958355,0.461061598022145,4.05293447196787));
#31308=CARTESIAN_POINT('Ctrl Pts',(14.218406330405,0.445731228298378,4.12924212785648));
#31309=CARTESIAN_POINT('Ctrl Pts',(14.2262777024549,0.413209431587385,4.19733954431574));
#31310=CARTESIAN_POINT('Ctrl Pts',(14.2341490745049,0.380687634876391,4.265436960775));
#31311=CARTESIAN_POINT('Ctrl Pts',(14.2420204465549,0.330974411178171,4.32532413780492));
#31312=CARTESIAN_POINT('Ctrl Pts',(14.2498918186048,0.270026820557645,4.36982488597043));
#31313=CARTESIAN_POINT('Ctrl Pts',(14.2577631906548,0.209079229937118,4.41432563413594));
#31314=CARTESIAN_POINT('Ctrl Pts',(14.2656345627047,0.136897272394287,4.44343995343705));
#31315=CARTESIAN_POINT('Ctrl Pts',(14.2735059347547,0.0621304022332317,
4.45367911922619));
#31316=CARTESIAN_POINT('Ctrl Pts',(14.2756720536747,0.0415553447945806,
4.4564968301158));
#31317=CARTESIAN_POINT('Ctrl Pts',(14.2778381725948,0.020784533837212,4.45788513960506));
#31318=CARTESIAN_POINT('Ctrl Pts',(14.2800042915148,1.11332528513013E-5,
4.45786561359635));
#31319=CARTESIAN_POINT('Origin',(12.5,0.,4.));
#31320=CARTESIAN_POINT('',(14.5800042915148,-1.58578451148518E-6,4.45791318879952));
#31321=CARTESIAN_POINT('',(14.4699957084852,4.96934848862042E-6,4.4578413260902));
#31322=CARTESIAN_POINT('',(12.5,-5.60735153159594E-17,4.457875));
#31323=CARTESIAN_POINT('Ctrl Pts',(14.4699957084852,4.96934848862042E-6,
4.4578413260902));
#31324=CARTESIAN_POINT('Ctrl Pts',(14.4666543524698,0.0320539454002899,
4.45785375637851));
#31325=CARTESIAN_POINT('Ctrl Pts',(14.4633129964543,0.0641003838712636,
4.45453523052653));
#31326=CARTESIAN_POINT('Ctrl Pts',(14.4599716404389,0.0954313752779353,
4.44785911407655));
#31327=CARTESIAN_POINT('Ctrl Pts',(14.452100268389,0.169239101517837,4.43213190746217));
#31328=CARTESIAN_POINT('Ctrl Pts',(14.444228896339,0.2390764403586,4.39777168651743));
#31329=CARTESIAN_POINT('Ctrl Pts',(14.4363575242891,0.296574889592956,4.34889578431359));
#31330=CARTESIAN_POINT('Ctrl Pts',(14.4284861522391,0.354073338827311,4.30001988210975));
#31331=CARTESIAN_POINT('Ctrl Pts',(14.4206147801891,0.39923289845526,4.2366282986468));
#31332=CARTESIAN_POINT('Ctrl Pts',(14.4127434081392,0.4266421670589,4.16631715105832));
#31333=CARTESIAN_POINT('Ctrl Pts',(14.4048720360892,0.454051435662541,4.09600600346984));
#31334=CARTESIAN_POINT('Ctrl Pts',(14.3970006640393,0.463710413241873,4.01877529175582));
#31335=CARTESIAN_POINT('Ctrl Pts',(14.3891292919893,0.454461679188747,3.94387945476197));
#31336=CARTESIAN_POINT('Ctrl Pts',(14.3812579199394,0.445212945135621,3.86898361776811));
#31337=CARTESIAN_POINT('Ctrl Pts',(14.3733865478894,0.417056499450037,3.79642265549441));
#31338=CARTESIAN_POINT('Ctrl Pts',(14.3655151758395,0.373366286239542,3.73489143780602));
#31339=CARTESIAN_POINT('Ctrl Pts',(14.3576438037895,0.329676073029047,3.67336022011762));
#31340=CARTESIAN_POINT('Ctrl Pts',(14.3497724317395,0.270452092293641,3.62285874701452));
#31341=CARTESIAN_POINT('Ctrl Pts',(14.3419010596896,0.202791063664024,3.58943853329022));
#31342=CARTESIAN_POINT('Ctrl Pts',(14.3340296876396,0.135130035034407,3.55601831956592));
#31343=CARTESIAN_POINT('Ctrl Pts',(14.3261583155897,0.0590319585105798,
3.53967936522043));
#31344=CARTESIAN_POINT('Ctrl Pts',(14.3182869435397,-0.0163844490157649,
3.54237954232867));
#31345=CARTESIAN_POINT('Ctrl Pts',(14.3104155714898,-0.0918008565421096,
3.54507971943691));
#31346=CARTESIAN_POINT('Ctrl Pts',(14.3025441994398,-0.166535595070972,
3.56681902799889));
#31347=CARTESIAN_POINT('Ctrl Pts',(14.2946728273899,-0.231633314431234,
3.60499247969884));
#31348=CARTESIAN_POINT('Ctrl Pts',(14.2868014553399,-0.296731033791496,
3.64316593139879));
#31349=CARTESIAN_POINT('Ctrl Pts',(14.2789300832899,-0.352191733983158,
3.6977735262367));
#31350=CARTESIAN_POINT('Ctrl Pts',(14.27105871124,-0.391369643565407,3.76227171909014));
#31351=CARTESIAN_POINT('Ctrl Pts',(14.26318733919,-0.430547553147657,3.82676991194359));
#31352=CARTESIAN_POINT('Ctrl Pts',(14.2553159671401,-0.453442672120494,
3.90115870281258));
#31353=CARTESIAN_POINT('Ctrl Pts',(14.2474445950901,-0.457311513162664,
3.97652419590847));
#31354=CARTESIAN_POINT('Ctrl Pts',(14.2395732230402,-0.461180354204834,
4.05188968900435));
#31355=CARTESIAN_POINT('Ctrl Pts',(14.2317018509902,-0.446022917316338,
4.12823188432714));
#31356=CARTESIAN_POINT('Ctrl Pts',(14.2238304789403,-0.413655495130362,
4.19640281260034));
#31357=CARTESIAN_POINT('Ctrl Pts',(14.2159591068903,-0.381288072944386,
4.26457374087354));
#31358=CARTESIAN_POINT('Ctrl Pts',(14.2080877348403,-0.33171066546093,4.32457340209717));
#31359=CARTESIAN_POINT('Ctrl Pts',(14.2002163627904,-0.270864058094251,
4.36921212802613));
#31360=CARTESIAN_POINT('Ctrl Pts',(14.1923449907404,-0.210017450727571,
4.41385085395509));
#31361=CARTESIAN_POINT('Ctrl Pts',(14.1844736186905,-0.137901643477669,
4.44312864458938));
#31362=CARTESIAN_POINT('Ctrl Pts',(14.1766022466405,-0.0631581639595259,
4.45353718675995));
#31363=CARTESIAN_POINT('Ctrl Pts',(14.1744000672554,-0.0422471272657682,
4.45644919204336));
#31364=CARTESIAN_POINT('Ctrl Pts',(14.1721978878703,-0.021130418320356,
4.45788427006097));
#31365=CARTESIAN_POINT('Ctrl Pts',(14.1699957084852,-1.10604184835328E-5,
4.4578646218584));
#31366=CARTESIAN_POINT('Ctrl Pts',(14.2800042915148,1.11332528513013E-5,
4.45786561359635));
#31367=CARTESIAN_POINT('Ctrl Pts',(14.2857095446447,-0.0547030874695854,
4.45781418483069));
#31368=CARTESIAN_POINT('Ctrl Pts',(14.2914147977746,-0.109435272994953,
4.44799629651036));
#31369=CARTESIAN_POINT('Ctrl Pts',(14.2971200509045,-0.16065599949712,4.42880599334559));
#31370=CARTESIAN_POINT('Ctrl Pts',(14.3049914229545,-0.231323748287136,
4.40232968939868));
#31371=CARTESIAN_POINT('Ctrl Pts',(14.3128627950045,-0.295307463087888,
4.35801306922771));
#31372=CARTESIAN_POINT('Ctrl Pts',(14.3207341670544,-0.344940072567234,
4.30116652609615));
#31373=CARTESIAN_POINT('Ctrl Pts',(14.3286055391044,-0.394572682046581,
4.24431998296459));
#31374=CARTESIAN_POINT('Ctrl Pts',(14.3364769111543,-0.429854186204522,
4.17494351687244));
#31375=CARTESIAN_POINT('Ctrl Pts',(14.3443482832043,-0.446556856002091,
4.10135040434572));
#31376=CARTESIAN_POINT('Ctrl Pts',(14.3522196552542,-0.46325952579966,4.027757291819));
#31377=CARTESIAN_POINT('Ctrl Pts',(14.3600910273042,-0.461383361236856,
3.9499475328577));
#31378=CARTESIAN_POINT('Ctrl Pts',(14.3679623993541,-0.441153180262727,
3.87724495265939));
#31379=CARTESIAN_POINT('Ctrl Pts',(14.3758337714041,-0.420922999288597,
3.80454237246108));
#31380=CARTESIAN_POINT('Ctrl Pts',(14.383705143454,-0.382338801903142,3.73694697102576));
#31381=CARTESIAN_POINT('Ctrl Pts',(14.391576515504,-0.330024073856894,3.68255860260764));
#31382=CARTESIAN_POINT('Ctrl Pts',(14.399447887554,-0.277709345810648,3.62817023418952));
#31383=CARTESIAN_POINT('Ctrl Pts',(14.4073192596039,-0.21166408710361,3.58698889878861));
#31384=CARTESIAN_POINT('Ctrl Pts',(14.4151906316539,-0.139802400742051,
3.56394929325792));
#31385=CARTESIAN_POINT('Ctrl Pts',(14.4230620037038,-0.0679407143804897,
3.54090968772722));
#31386=CARTESIAN_POINT('Ctrl Pts',(14.4309333757538,0.00973739963559066,
3.53601181206673));
#31387=CARTESIAN_POINT('Ctrl Pts',(14.4388047478037,0.0839238909224197,
3.54984257127538));
#31388=CARTESIAN_POINT('Ctrl Pts',(14.4466761198537,0.158110382209248,3.56367333048403));
#31389=CARTESIAN_POINT('Ctrl Pts',(14.4545474919037,0.228805250766822,3.59623272456181));
#31390=CARTESIAN_POINT('Ctrl Pts',(14.4624188639536,0.287537237904754,3.64361921078484));
#31391=CARTESIAN_POINT('Ctrl Pts',(14.4702902360036,0.346269225042686,3.69100569700788));
#31392=CARTESIAN_POINT('Ctrl Pts',(14.4781616080535,0.393038330760977,3.75321927537615));
#31393=CARTESIAN_POINT('Ctrl Pts',(14.4860329801035,0.422240284179214,3.8228049873169));
#31394=CARTESIAN_POINT('Ctrl Pts',(14.4939043521534,0.451442237597453,3.89239069925764));
#31395=CARTESIAN_POINT('Ctrl Pts',(14.5017757242034,0.463077038715637,3.96934854477086));
#31396=CARTESIAN_POINT('Ctrl Pts',(14.5096470962533,0.45575050699275,4.04445678215295));
#31397=CARTESIAN_POINT('Ctrl Pts',(14.5175184683033,0.448423975269863,4.11956501953505));
#31398=CARTESIAN_POINT('Ctrl Pts',(14.5253898403532,0.422136110705906,4.19282364878603));
#31399=CARTESIAN_POINT('Ctrl Pts',(14.5332612124032,0.380036948171907,4.2554541996672));
#31400=CARTESIAN_POINT('Ctrl Pts',(14.5411325844532,0.337937785637909,4.31808475054837));
#31401=CARTESIAN_POINT('Ctrl Pts',(14.5490039565031,0.28002732513387,4.37008722305972));
#31402=CARTESIAN_POINT('Ctrl Pts',(14.5568753285531,0.213244889156206,4.40523023992844));
#31403=CARTESIAN_POINT('Ctrl Pts',(14.5645849828737,0.147834501639678,4.43965124177167));
#31404=CARTESIAN_POINT('Ctrl Pts',(14.5722946371942,0.0739129441497101,
4.45789842831743));
#31405=CARTESIAN_POINT('Ctrl Pts',(14.5800042915148,-1.58578451148518E-6,
4.45791318879952));
#31406=CARTESIAN_POINT('Origin',(12.5,0.,4.));
#31407=CARTESIAN_POINT('',(14.8800042915148,-1.01702808208336E-5,4.45785711824254));
#31408=CARTESIAN_POINT('',(14.7699957084852,8.6346448269735E-6,4.45789857801605));
#31409=CARTESIAN_POINT('',(12.5,-5.60735153159594E-17,4.457875));
#31410=CARTESIAN_POINT('Ctrl Pts',(14.7699957084852,8.6346448269735E-6,
4.45789857801605));
#31411=CARTESIAN_POINT('Ctrl Pts',(14.7689821891192,0.00972641784825355,
4.45790700998655));
#31412=CARTESIAN_POINT('Ctrl Pts',(14.7679686697532,0.01944367562558,4.45760386164098));
#31413=CARTESIAN_POINT('Ctrl Pts',(14.7669551503872,0.0291408329004781,
4.45698549795522));
#31414=CARTESIAN_POINT('Ctrl Pts',(14.7590837783372,0.104452598317788,4.45218305332902));
#31415=CARTESIAN_POINT('Ctrl Pts',(14.7512124062873,0.178551969979598,4.4283678943965));
#31416=CARTESIAN_POINT('Ctrl Pts',(14.7433410342373,0.242559732875008,4.38839375563686));
#31417=CARTESIAN_POINT('Ctrl Pts',(14.7354696621874,0.30656749577042,4.34841961687722));
#31418=CARTESIAN_POINT('Ctrl Pts',(14.7275982901374,0.360483649899433,4.29228649829047));
#31419=CARTESIAN_POINT('Ctrl Pts',(14.7197269180875,0.397847504376097,4.22672074611392));
#31420=CARTESIAN_POINT('Ctrl Pts',(14.7118555460375,0.435211358852761,4.16115499393738));
#31421=CARTESIAN_POINT('Ctrl Pts',(14.7039841739875,0.456022913677073,4.08615660817103));
#31422=CARTESIAN_POINT('Ctrl Pts',(14.6961128019376,0.457788351878884,4.01071253147039));
#31423=CARTESIAN_POINT('Ctrl Pts',(14.6882414298876,0.459553790080695,3.93526845476975));
#31424=CARTESIAN_POINT('Ctrl Pts',(14.6803700578377,0.442273111660005,3.85937868713481));
#31425=CARTESIAN_POINT('Ctrl Pts',(14.6724986857877,0.408017034045316,3.79213698410258));
#31426=CARTESIAN_POINT('Ctrl Pts',(14.6646273137378,0.373760956430627,3.72489528107034));
#31427=CARTESIAN_POINT('Ctrl Pts',(14.6567559416878,0.32252947962194,3.6663016426408));
#31428=CARTESIAN_POINT('Ctrl Pts',(14.6488845696379,0.260461593653079,3.6233772554918));
#31429=CARTESIAN_POINT('Ctrl Pts',(14.6410131975879,0.198393707684219,3.5804528683428));
#31430=CARTESIAN_POINT('Ctrl Pts',(14.6331418255379,0.125489412555185,3.55319773247434));
#31431=CARTESIAN_POINT('Ctrl Pts',(14.625270453488,0.0504847191830214,3.54487778940425));
#31432=CARTESIAN_POINT('Ctrl Pts',(14.617399081438,-0.0245199741891427,
3.53655784633416));
#31433=CARTESIAN_POINT('Ctrl Pts',(14.6095277093881,-0.101625065804437,
3.54717309606245));
#31434=CARTESIAN_POINT('Ctrl Pts',(14.6016563373381,-0.171591169681571,
3.57545152934398));
#31435=CARTESIAN_POINT('Ctrl Pts',(14.5937849652882,-0.241557273558703,
3.6037299626255));
#31436=CARTESIAN_POINT('Ctrl Pts',(14.5859135932382,-0.304384389697674,
3.64967157946028));
#31437=CARTESIAN_POINT('Ctrl Pts',(14.5780422211883,-0.352544040227279,
3.70777126570269));
#31438=CARTESIAN_POINT('Ctrl Pts',(14.5701708491383,-0.400703690756885,
3.7658709519451));
#31439=CARTESIAN_POINT('Ctrl Pts',(14.5622994770883,-0.434195875677124,
3.83612870759516));
#31440=CARTESIAN_POINT('Ctrl Pts',(14.5544281050384,-0.449007277354457,
3.91012565253846));
#31441=CARTESIAN_POINT('Ctrl Pts',(14.5465567329884,-0.46381867903179,3.98412259748177));
#31442=CARTESIAN_POINT('Ctrl Pts',(14.5386853609385,-0.459949297466218,
4.06185873171832));
#31443=CARTESIAN_POINT('Ctrl Pts',(14.5308139888885,-0.437862794771992,
4.13401905238929));
#31444=CARTESIAN_POINT('Ctrl Pts',(14.5229426168386,-0.415776292077766,
4.20617937306026));
#31445=CARTESIAN_POINT('Ctrl Pts',(14.5150712447886,-0.375472668254887,
4.27276388016565));
#31446=CARTESIAN_POINT('Ctrl Pts',(14.5071998727387,-0.321781445311454,
4.32579385338299));
#31447=CARTESIAN_POINT('Ctrl Pts',(14.4993285006887,-0.26809022236802,4.37882382660034));
#31448=CARTESIAN_POINT('Ctrl Pts',(14.4914571286387,-0.201011400304033,
4.41829926592964));
#31449=CARTESIAN_POINT('Ctrl Pts',(14.4835857565888,-0.128582932452519,
4.43948988945229));
#31450=CARTESIAN_POINT('Ctrl Pts',(14.4790557405542,-0.0868999680795747,
4.45168520479633));
#31451=CARTESIAN_POINT('Ctrl Pts',(14.4745257245197,-0.0434451672832877,
4.45782447382869));
#31452=CARTESIAN_POINT('Ctrl Pts',(14.4699957084852,4.96934848862042E-6,
4.4578413260902));
#31453=CARTESIAN_POINT('Ctrl Pts',(14.5800042915148,-1.58578451148518E-6,
4.45791318879952));
#31454=CARTESIAN_POINT('Ctrl Pts',(14.5801660092442,-0.00155201715944126,
4.45791349841543));
#31455=CARTESIAN_POINT('Ctrl Pts',(14.5803277269736,-0.00310244544229786,
4.45790578589721));
#31456=CARTESIAN_POINT('Ctrl Pts',(14.5804894447029,-0.0046527920161852,
4.45789003224535));
#31457=CARTESIAN_POINT('Ctrl Pts',(14.5883608167529,-0.0801136257596197,
4.45712324646747));
#31458=CARTESIAN_POINT('Ctrl Pts',(14.5962321888029,-0.155380881795201,
4.43730611368561));
#31459=CARTESIAN_POINT('Ctrl Pts',(14.6041035608528,-0.22143539919095,4.4008132908088));
#31460=CARTESIAN_POINT('Ctrl Pts',(14.6119749329028,-0.287489916586699,
4.36432046793199));
#31461=CARTESIAN_POINT('Ctrl Pts',(14.6198463049527,-0.344331695342615,
4.31115195496024));
#31462=CARTESIAN_POINT('Ctrl Pts',(14.6277176770027,-0.38514947146564,4.24767885402976));
#31463=CARTESIAN_POINT('Ctrl Pts',(14.6355890490526,-0.425967247588666,
4.18420575309928));
#31464=CARTESIAN_POINT('Ctrl Pts',(14.6434604211026,-0.4507610210788,4.11042806421008));
#31465=CARTESIAN_POINT('Ctrl Pts',(14.6513317931525,-0.45655979174196,4.03518645571321));
#31466=CARTESIAN_POINT('Ctrl Pts',(14.6592031652025,-0.462358562405121,
3.95994484721634));
#31467=CARTESIAN_POINT('Ctrl Pts',(14.6670745372524,-0.449162330241309,
3.8832393191118));
#31468=CARTESIAN_POINT('Ctrl Pts',(14.6749459093024,-0.41855237967279,3.81426137832517));
#31469=CARTESIAN_POINT('Ctrl Pts',(14.6828172813524,-0.387942429104271,
3.74528343753854));
#31470=CARTESIAN_POINT('Ctrl Pts',(14.6906886534023,-0.339918760131043,
3.68403308406983));
#31471=CARTESIAN_POINT('Ctrl Pts',(14.6985600254523,-0.280235976103336,
3.63784985464301));
#31472=CARTESIAN_POINT('Ctrl Pts',(14.7064313975022,-0.220553192075631,
3.5916666252162));
#31473=CARTESIAN_POINT('Ctrl Pts',(14.7143027695522,-0.149211292993445,
3.5605505198313));
#31474=CARTESIAN_POINT('Ctrl Pts',(14.7221741416021,-0.0747590701011626,
3.54823013427646));
#31475=CARTESIAN_POINT('Ctrl Pts',(14.7300455136521,-0.000306847208877067,
3.53590974872161));
#31476=CARTESIAN_POINT('Ctrl Pts',(14.737916885702,0.0772556994935079,3.54238508299684));
#31477=CARTESIAN_POINT('Ctrl Pts',(14.745788257752,0.148634367597872,3.5668802073009));
#31478=CARTESIAN_POINT('Ctrl Pts',(14.753659629802,0.220013035702235,3.59137533160497));
#31479=CARTESIAN_POINT('Ctrl Pts',(14.7615310018519,0.285207825208577,3.63389024593787));
#31480=CARTESIAN_POINT('Ctrl Pts',(14.7694023739019,0.336406544142474,3.68933045342307));
#31481=CARTESIAN_POINT('Ctrl Pts',(14.7772737459518,0.387605263076371,3.74477066090827));
#31482=CARTESIAN_POINT('Ctrl Pts',(14.7851451180018,0.424807911437823,3.81313616154577));
#31483=CARTESIAN_POINT('Ctrl Pts',(14.7930164900517,0.443556551112275,3.88623481973509));
#31484=CARTESIAN_POINT('Ctrl Pts',(14.8008878621017,0.462305190786727,3.9593334779244));
#31485=CARTESIAN_POINT('Ctrl Pts',(14.8087592341516,0.462599821774179,4.03716529366552));
#31486=CARTESIAN_POINT('Ctrl Pts',(14.8166306062016,0.444405141642572,4.11040380200553));
#31487=CARTESIAN_POINT('Ctrl Pts',(14.8245019782516,0.426210461510966,4.18364231034555));
#31488=CARTESIAN_POINT('Ctrl Pts',(14.8323733503015,0.389526470260302,4.25228751128446));
#31489=CARTESIAN_POINT('Ctrl Pts',(14.8402447223515,0.338748948932789,4.3081137476731));
#31490=CARTESIAN_POINT('Ctrl Pts',(14.8481160944014,0.287971427605278,4.36393998406173));
#31491=CARTESIAN_POINT('Ctrl Pts',(14.8559874664514,0.22310037620092,4.40694725590009));
#31492=CARTESIAN_POINT('Ctrl Pts',(14.8638588385013,0.151909206873508,4.43198208217373));
#31493=CARTESIAN_POINT('Ctrl Pts',(14.8692406561725,0.103234351881841,4.44909890368578));
#31494=CARTESIAN_POINT('Ctrl Pts',(14.8746224738437,0.0516050086776526,
4.45781408155485));
#31495=CARTESIAN_POINT('Ctrl Pts',(14.8800042915148,-1.01702808208336E-5,
4.45785711824254));
#31496=CARTESIAN_POINT('Origin',(12.5,0.,4.));
#31497=CARTESIAN_POINT('',(15.1,-5.60735153159594E-17,4.457875));
#31498=CARTESIAN_POINT('',(15.0699957084852,-1.05870731373636E-5,4.45788944868556));
#31499=CARTESIAN_POINT('',(12.5,-5.60735153159594E-17,4.457875));
#31500=CARTESIAN_POINT('',(15.1,-0.269165465906718,4.37040446485999));
#31501=CARTESIAN_POINT('Origin',(15.1,0.,4.));
#31502=CARTESIAN_POINT('Ctrl Pts',(15.1,-0.269173508333955,4.37043259773194));
#31503=CARTESIAN_POINT('Ctrl Pts',(15.0991842588284,-0.262849866117432,
4.37503549456412));
#31504=CARTESIAN_POINT('Ctrl Pts',(15.0983685176569,-0.256407545646713,
4.37947450812006));
#31505=CARTESIAN_POINT('Ctrl Pts',(15.0975527764853,-0.249853611926923,
4.38374199825787));
#31506=CARTESIAN_POINT('Ctrl Pts',(15.0896814044354,-0.186612411779406,
4.42492050409441));
#31507=CARTESIAN_POINT('Ctrl Pts',(15.0818100323854,-0.112978907049287,
4.45012847221118));
#31508=CARTESIAN_POINT('Ctrl Pts',(15.0739386603355,-0.0377721395608013,
4.45635245505497));
#31509=CARTESIAN_POINT('Ctrl Pts',(15.072624343052,-0.0252145379490987,
4.45739170058566));
#31510=CARTESIAN_POINT('Ctrl Pts',(15.0713100257686,-0.0126130730861363,
4.45790166433459));
#31511=CARTESIAN_POINT('Ctrl Pts',(15.0699957084852,-1.05870731373636E-5,
4.45788944868556));
#31512=CARTESIAN_POINT('Origin',(11.8752146997001,0.,4.));
#31513=CARTESIAN_POINT('',(14.9247853002999,-1.38824472118437E-5,4.62497559137666));
#31514=CARTESIAN_POINT('',(15.0252146997001,-1.44513692928093E-5,4.62501972247551));
#31515=CARTESIAN_POINT('',(11.8752146997001,-1.68747709936658E-14,4.625));
#31516=CARTESIAN_POINT('',(15.1,-0.624993681275899,4.00281040303151));
#31517=CARTESIAN_POINT('Ctrl Pts',(15.0252146997001,-1.44513692928189E-5,
4.62501972247551));
#31518=CARTESIAN_POINT('Ctrl Pts',(15.0265290169835,-0.017216861979444,
4.62503639685311));
#31519=CARTESIAN_POINT('Ctrl Pts',(15.0357147063169,-0.137433797398843,
4.62017138475037));
#31520=CARTESIAN_POINT('Ctrl Pts',(15.0527717677003,-0.355236031271534,
4.54560815721762));
#31521=CARTESIAN_POINT('Ctrl Pts',(15.0763858838501,-0.571652475026301,
4.31158258982903));
#31522=CARTESIAN_POINT('Ctrl Pts',(15.09212862795,-0.624530364890795,4.10584538053252));
#31523=CARTESIAN_POINT('Ctrl Pts',(15.1,-0.624993681275899,4.00281040303152));
#31524=CARTESIAN_POINT('',(15.1,0.314930721058197,3.46014479632612));
#31525=CARTESIAN_POINT('Origin',(15.1,0.,4.));
#31526=CARTESIAN_POINT('Ctrl Pts',(14.9247853002999,-1.38824472118368E-5,
4.62497559137666));
#31527=CARTESIAN_POINT('Ctrl Pts',(14.9272748546787,-0.0326052931943186,
4.62500276606431));
#31528=CARTESIAN_POINT('Ctrl Pts',(14.9376357811074,-0.168225686180582,
4.61457389311938));
#31529=CARTESIAN_POINT('Ctrl Pts',(14.9558680795861,-0.394527586443172,
4.517903766532));
#31530=CARTESIAN_POINT('Ctrl Pts',(14.979482195736,-0.593077772790822,4.26857965265179));
#31531=CARTESIAN_POINT('Ctrl Pts',(15.0030963118859,-0.649493436571599,
3.95488773069898));
#31532=CARTESIAN_POINT('Ctrl Pts',(15.0267104280357,-0.550252000240565,
3.65200904506483));
#31533=CARTESIAN_POINT('Ctrl Pts',(15.0503245441856,-0.319142060764588,
3.43252503194012));
#31534=CARTESIAN_POINT('Ctrl Pts',(15.0739386603355,-0.0115409051696555,
3.34904846156061));
#31535=CARTESIAN_POINT('Ctrl Pts',(15.0904971456069,0.20608092381284,3.39989411918499));
#31536=CARTESIAN_POINT('Ctrl Pts',(15.0991842588284,0.305720220830039,3.45471854406458));
#31537=CARTESIAN_POINT('Ctrl Pts',(15.1,0.314937815442301,3.46010549098218));
#31538=CARTESIAN_POINT('Origin',(11.8752146997001,0.,4.));
#31539=CARTESIAN_POINT('',(14.6247853002999,-2.16459804047719E-6,4.62505212776347));
#31540=CARTESIAN_POINT('',(14.7252146997001,1.17863019661874E-5,4.62503218402409));
#31541=CARTESIAN_POINT('',(11.8752146997001,-1.68747709936658E-14,4.625));
#31542=CARTESIAN_POINT('Ctrl Pts',(14.7252146997001,1.17863019662174E-5,
4.62503218402409));
#31543=CARTESIAN_POINT('Ctrl Pts',(14.7320725523841,-0.0897427467603322,
4.62495430540108));
#31544=CARTESIAN_POINT('Ctrl Pts',(14.746801777118,-0.282587126126967,4.58296482291278));
#31545=CARTESIAN_POINT('Ctrl Pts',(14.7694023739019,-0.520130285395982,
4.39158760667368));
#31546=CARTESIAN_POINT('Ctrl Pts',(14.7930164900517,-0.64367318065081,4.09778141619902));
#31547=CARTESIAN_POINT('Ctrl Pts',(14.8166306062016,-0.612955311082805,
3.78054123783642));
#31548=CARTESIAN_POINT('Ctrl Pts',(14.8402447223515,-0.435338447621071,
3.51589585985611));
#31549=CARTESIAN_POINT('Ctrl Pts',(14.8638588385013,-0.153389665944836,
3.36726945127358));
#31550=CARTESIAN_POINT('Ctrl Pts',(14.8874729546512,0.165319955489652,3.37028123293502));
#31551=CARTESIAN_POINT('Ctrl Pts',(14.9110870708011,0.444409630539555,3.52420969451069));
#31552=CARTESIAN_POINT('Ctrl Pts',(14.9347011869509,0.616993161964042,3.79216419995926));
#31553=CARTESIAN_POINT('Ctrl Pts',(14.9583153031008,0.641710593195818,4.10992889087348));
#31554=CARTESIAN_POINT('Ctrl Pts',(14.9819294192507,0.512636325700993,4.40134645341462));
#31555=CARTESIAN_POINT('Ctrl Pts',(15.0042292181171,0.274729866520086,4.58571614948967));
#31556=CARTESIAN_POINT('Ctrl Pts',(15.0186576449336,0.0858074045169303,
4.62493653494651));
#31557=CARTESIAN_POINT('Ctrl Pts',(15.0252146997001,-1.44513692928189E-5,
4.62501972247551));
#31558=CARTESIAN_POINT('Ctrl Pts',(14.6247853002999,-2.16459804049194E-6,
4.62505212776347));
#31559=CARTESIAN_POINT('Ctrl Pts',(14.6249470180292,-0.00211850554115318,
4.62505255038961));
#31560=CARTESIAN_POINT('Ctrl Pts',(14.6329801078086,-0.107244412024774,
4.62452960748548));
#31561=CARTESIAN_POINT('Ctrl Pts',(14.6488845696379,-0.314835022974042,
4.56987302880665));
#31562=CARTESIAN_POINT('Ctrl Pts',(14.6724986857877,-0.547602339746838,
4.35214775046202));
#31563=CARTESIAN_POINT('Ctrl Pts',(14.6961128019376,-0.649132943719538,
4.05002781234082));
#31564=CARTESIAN_POINT('Ctrl Pts',(14.7197269180875,-0.595094318970103,
3.73591836064326));
#31565=CARTESIAN_POINT('Ctrl Pts',(14.7433410342373,-0.398437197867616,
3.48509791236843));
#31566=CARTESIAN_POINT('Ctrl Pts',(14.7669551503872,-0.1062918289807,3.35767733339665));
#31567=CARTESIAN_POINT('Ctrl Pts',(14.7905692665371,0.211327117384507,3.38419385377023));
#31568=CARTESIAN_POINT('Ctrl Pts',(14.8141833826869,0.478300047385911,3.5582926020622));
#31569=CARTESIAN_POINT('Ctrl Pts',(14.8377974988368,0.630645044771057,3.83824960712979));
#31570=CARTESIAN_POINT('Ctrl Pts',(14.8614116149867,0.631851559871185,4.15697121131127));
#31571=CARTESIAN_POINT('Ctrl Pts',(14.8850257311365,0.481630465478622,4.4380735902585));
#31572=CARTESIAN_POINT('Ctrl Pts',(14.9061502929076,0.243989509668873,4.59562135563586));
#31573=CARTESIAN_POINT('Ctrl Pts',(14.9194034826287,0.0704409072858971,
4.62491684623921));
#31574=CARTESIAN_POINT('Ctrl Pts',(14.9247853002999,-1.38824472118368E-5,
4.62497559137666));
#31575=CARTESIAN_POINT('Origin',(11.8752146997001,0.,4.));
#31576=CARTESIAN_POINT('',(14.3247853002999,1.51969053300144E-5,4.6249871875462));
#31577=CARTESIAN_POINT('',(14.4252146997001,6.78316748347314E-6,4.62495403506715));
#31578=CARTESIAN_POINT('',(11.8752146997001,-1.68747709936658E-14,4.625));
#31579=CARTESIAN_POINT('Ctrl Pts',(14.4252146997001,6.78316748347826E-6,
4.62495403506715));
#31580=CARTESIAN_POINT('Ctrl Pts',(14.4297447157347,-0.0593027126443913,
4.62493103170719));
#31581=CARTESIAN_POINT('Ctrl Pts',(14.4421461038192,-0.221686029527806,
4.60198961095629));
#31582=CARTESIAN_POINT('Ctrl Pts',(14.4624188639536,-0.457506203155893,
4.46321101183598));
#31583=CARTESIAN_POINT('Ctrl Pts',(14.4860329801035,-0.622549707754089,
4.19054718257559));
#31584=CARTESIAN_POINT('Ctrl Pts',(14.5096470962533,-0.63839484111024,3.87221739454711));
#31585=CARTESIAN_POINT('Ctrl Pts',(14.5332612124032,-0.501244206711231,
3.58451159745434));
#31586=CARTESIAN_POINT('Ctrl Pts',(14.5568753285531,-0.243966908844842,
3.39638048838484));
#31587=CARTESIAN_POINT('Ctrl Pts',(14.5804894447029,0.0717787570654544,
3.35291099727801));
#31588=CARTESIAN_POINT('Ctrl Pts',(14.6041035608528,0.370322144162233,3.46452089026927));
#31589=CARTESIAN_POINT('Ctrl Pts',(14.6277176770027,0.580115251486915,3.70446207957941));
#31590=CARTESIAN_POINT('Ctrl Pts',(14.6513317931525,0.650879700384091,4.0152309888134));
#31591=CARTESIAN_POINT('Ctrl Pts',(14.6749459093024,0.565656298155129,4.32234968564526));
#31592=CARTESIAN_POINT('Ctrl Pts',(14.6985600254523,0.344869426209941,4.55221503612336));
#31593=CARTESIAN_POINT('Ctrl Pts',(14.7153162889182,0.129554394067723,4.62141618582314));
#31594=CARTESIAN_POINT('Ctrl Pts',(14.7242011803341,0.0132765736394338,
4.62504369367533));
#31595=CARTESIAN_POINT('Ctrl Pts',(14.7252146997001,1.17863019662174E-5,
4.62503218402409));
#31596=CARTESIAN_POINT('Ctrl Pts',(14.3247853002999,1.51969053300109E-5,
4.6249871875462));
#31597=CARTESIAN_POINT('Ctrl Pts',(14.3304905534298,-0.0746697890657793,
4.62491698721088));
#31598=CARTESIAN_POINT('Ctrl Pts',(14.3440671786096,-0.252453835406249,
4.59302599116618));
#31599=CARTESIAN_POINT('Ctrl Pts',(14.3655151758395,-0.490432948250941,
4.42819608115853));
#31600=CARTESIAN_POINT('Ctrl Pts',(14.3891292919893,-0.634910852255616,
4.14409916841427));
#31601=CARTESIAN_POINT('Ctrl Pts',(14.4127434081392,-0.627227950688033,
3.82546788683648));
#31602=CARTESIAN_POINT('Ctrl Pts',(14.4363575242891,-0.469225504392149,
3.54866444115539));
#31603=CARTESIAN_POINT('Ctrl Pts',(14.4599716404389,-0.198769899531221,
3.38002670405092));
#31604=CARTESIAN_POINT('Ctrl Pts',(14.4835857565888,0.11932229545683,3.35996988316441));
#31605=CARTESIAN_POINT('Ctrl Pts',(14.5071998727387,0.408818071695872,3.49330073524378));
#31606=CARTESIAN_POINT('Ctrl Pts',(14.5308139888885,0.600337751131954,3.74806559342675));
#31607=CARTESIAN_POINT('Ctrl Pts',(14.5544281050384,0.647982309355475,4.06320828594604));
#31608=CARTESIAN_POINT('Ctrl Pts',(14.5780422211883,0.540333396317157,4.36320267272319));
#31609=CARTESIAN_POINT('Ctrl Pts',(14.6014946196088,0.304813865567294,4.57469465218781));
#31610=CARTESIAN_POINT('Ctrl Pts',(14.6170756459793,0.100891269655612,4.62503197968527));
#31611=CARTESIAN_POINT('Ctrl Pts',(14.6247853002999,-2.16459804049194E-6,
4.62505212776347));
#31612=CARTESIAN_POINT('Origin',(11.8752146997001,0.,4.));
#31613=CARTESIAN_POINT('',(14.0247853002999,-6.3966029390794E-6,4.62495348172753));
#31614=CARTESIAN_POINT('',(14.1252146997001,-1.50974863142078E-5,4.62498583382255));
#31615=CARTESIAN_POINT('',(11.8752146997001,-1.68747709936658E-14,4.625));
#31616=CARTESIAN_POINT('Ctrl Pts',(14.1252146997001,-1.50974863141889E-5,
4.62498583382255));
#31617=CARTESIAN_POINT('Ctrl Pts',(14.1274168790852,-0.0288430498503269,
4.62501265364587));
#31618=CARTESIAN_POINT('Ctrl Pts',(14.1374904305203,-0.160695812902997,
4.61605202430223));
#31619=CARTESIAN_POINT('Ctrl Pts',(14.1554353540053,-0.385112282251534,
4.52494275637564));
#31620=CARTESIAN_POINT('Ctrl Pts',(14.1790494701552,-0.588131968915973,
4.27924389796604));
#31621=CARTESIAN_POINT('Ctrl Pts',(14.2026635863051,-0.65020173504413,3.96662229549764));
#31622=CARTESIAN_POINT('Ctrl Pts',(14.2262777024549,-0.556446129094758,
3.66199989226673));
#31623=CARTESIAN_POINT('Ctrl Pts',(14.2498918186048,-0.329334334698108,
3.43838156778717));
#31624=CARTESIAN_POINT('Ctrl Pts',(14.2735059347547,-0.0232952743833569,
3.34935901020328));
#31625=CARTESIAN_POINT('Ctrl Pts',(14.2971200509045,0.28832666060365,3.41626709515619));
#31626=CARTESIAN_POINT('Ctrl Pts',(14.3207341670544,0.530849104237583,3.62307083431711));
#31627=CARTESIAN_POINT('Ctrl Pts',(14.3443482832043,0.646149864620809,3.92020827196535));
#31628=CARTESIAN_POINT('Ctrl Pts',(14.3679623993541,0.606596311879891,4.2364683526943));
#31629=CARTESIAN_POINT('Ctrl Pts',(14.391576515504,0.42166773027486,4.49605714656388));
#31630=CARTESIAN_POINT('Ctrl Pts',(14.4106606156193,0.190545343529355,4.60977018898031));
#31631=CARTESIAN_POINT('Ctrl Pts',(14.4218733436847,0.0437536792250838,
4.62497100242767));
#31632=CARTESIAN_POINT('Ctrl Pts',(14.4252146997001,6.78316748347826E-6,
4.62495403506715));
#31633=CARTESIAN_POINT('Ctrl Pts',(14.0247853002999,-6.39660293913491E-6,
4.62495348172753));
#31634=CARTESIAN_POINT('Ctrl Pts',(14.0281627167804,-0.0442255271350925,
4.62496963662755));
#31635=CARTESIAN_POINT('Ctrl Pts',(14.0394115053108,-0.191490205391595,
4.6095527480466));
#31636=CARTESIAN_POINT('Ctrl Pts',(14.0585316658912,-0.422790583021024,
4.49510047824495));
#31637=CARTESIAN_POINT('Ctrl Pts',(14.0821457820411,-0.60713052675338,4.23509335195577));
#31638=CARTESIAN_POINT('Ctrl Pts',(14.1057598981909,-0.645967413308333,
3.91874446730605));
#31639=CARTESIAN_POINT('Ctrl Pts',(14.1293740143408,-0.529993712466286,
3.62186903671368));
#31640=CARTESIAN_POINT('Ctrl Pts',(14.1529881304907,-0.287003328966194,
3.41561532377041));
#31641=CARTESIAN_POINT('Ctrl Pts',(14.1766022466405,0.0247694002478971,
3.34941346658496));
#31642=CARTESIAN_POINT('Ctrl Pts',(14.2002163627904,0.330605970264406,3.43912920108534));
#31643=CARTESIAN_POINT('Ctrl Pts',(14.2238304789403,0.557210518047066,3.66326152695696));
#31644=CARTESIAN_POINT('Ctrl Pts',(14.2474445950901,0.650275686248857,3.96809557204375));
#31645=CARTESIAN_POINT('Ctrl Pts',(14.27105871124,0.587497759452106,4.28057573538778));
#31646=CARTESIAN_POINT('Ctrl Pts',(14.2946728273899,0.383921904832036,4.52581397056352));
#31647=CARTESIAN_POINT('Ctrl Pts',(14.3125816904098,0.159750963363977,4.61623247111552));
#31648=CARTESIAN_POINT('Ctrl Pts',(14.3226191813798,0.0283709170587055,
4.62501384057475));
#31649=CARTESIAN_POINT('Ctrl Pts',(14.3247853002999,1.51969053300109E-5,
4.6249871875462));
#31650=CARTESIAN_POINT('Origin',(11.8752146997001,0.,4.));
#31651=CARTESIAN_POINT('',(13.7247853002999,-1.20831421157597E-5,4.62503091248755));
#31652=CARTESIAN_POINT('',(13.8252146997001,1.68461488569462E-6,4.62505238998457));
#31653=CARTESIAN_POINT('',(11.8752146997001,-1.68747709936658E-14,4.625));
#31654=CARTESIAN_POINT('Ctrl Pts',(13.8252146997001,1.68461488569581E-6,
4.62505238998457));
#31655=CARTESIAN_POINT('Ctrl Pts',(13.8329604144858,-0.101363538932993,
4.62503644193381));
#31656=CARTESIAN_POINT('Ctrl Pts',(13.8485775013214,-0.305753798836605,
4.57432856173903));
#31657=CARTESIAN_POINT('Ctrl Pts',(13.8720659602069,-0.541154937947787,
4.36197748624323));
#31658=CARTESIAN_POINT('Ctrl Pts',(13.8956800763568,-0.648123865072376,
4.06173996222779));
#31659=CARTESIAN_POINT('Ctrl Pts',(13.9192941925067,-0.599765396122921,
3.74670602647169));
#31660=CARTESIAN_POINT('Ctrl Pts',(13.9429083086565,-0.407668974822819,
3.49237575473668));
#31661=CARTESIAN_POINT('Ctrl Pts',(13.9665224248064,-0.117871845784803,
3.35970116712309));
#31662=CARTESIAN_POINT('Ctrl Pts',(13.9901365409563,0.200174091641329,3.38047865214521));
#31663=CARTESIAN_POINT('Ctrl Pts',(14.0137506571061,0.470246914526057,3.54972874087838));
#31664=CARTESIAN_POINT('Ctrl Pts',(14.037364773256,0.627621790796785,3.82688947135059));
#31665=CARTESIAN_POINT('Ctrl Pts',(14.0609788894059,0.634582735815489,4.14553734509456));
#31666=CARTESIAN_POINT('Ctrl Pts',(14.0845930055557,0.489461510650943,4.42930618095194));
#31667=CARTESIAN_POINT('Ctrl Pts',(14.1060049423205,0.251510284961593,4.59332024860173));
#31668=CARTESIAN_POINT('Ctrl Pts',(14.1195455070353,0.074198300926532,4.62491679006221));
#31669=CARTESIAN_POINT('Ctrl Pts',(14.1252146997001,-1.50974863141889E-5,
4.62498583382255));
#31670=CARTESIAN_POINT('Ctrl Pts',(13.7247853002999,-1.20831421156938E-5,
4.62503091248755));
#31671=CARTESIAN_POINT('Ctrl Pts',(13.7258348801309,-0.013748904810447,
4.62504304225186));
#31672=CARTESIAN_POINT('Ctrl Pts',(13.734755832012,-0.130498998332177,4.62127102305724));
#31673=CARTESIAN_POINT('Ctrl Pts',(13.7515481559429,-0.346119716157775,
4.55143222859795));
#31674=CARTESIAN_POINT('Ctrl Pts',(13.7751622720928,-0.566385203513325,
4.32106722332061));
#31675=CARTESIAN_POINT('Ctrl Pts',(13.7987763882427,-0.650912534047929,
4.01375622291695));
#31676=CARTESIAN_POINT('Ctrl Pts',(13.8223905043925,-0.57944414457563,3.70314844792952));
#31677=CARTESIAN_POINT('Ctrl Pts',(13.8460046205424,-0.369107932149097,
3.46368321387984));
#31678=CARTESIAN_POINT('Ctrl Pts',(13.8696187366923,-0.0703124342978696,
3.35275003110641));
#31679=CARTESIAN_POINT('Ctrl Pts',(13.8932328528421,0.245333927901481,3.3969348091043));
#31680=CARTESIAN_POINT('Ctrl Pts',(13.916846968992,0.502184306426786,3.58564835824111));
#31681=CARTESIAN_POINT('Ctrl Pts',(13.9404610851419,0.638682720042094,3.87366416276737));
#31682=CARTESIAN_POINT('Ctrl Pts',(13.9640752012917,0.62211637371287,4.19195723015293));
#31683=CARTESIAN_POINT('Ctrl Pts',(13.9876893174416,0.456455507660852,4.46424641105313));
#31684=CARTESIAN_POINT('Ctrl Pts',(14.007926017111,0.220741531225703,4.60224444133776));
#31685=CARTESIAN_POINT('Ctrl Pts',(14.0202913447304,0.058831122868106,4.62493198618401));
#31686=CARTESIAN_POINT('Ctrl Pts',(14.0247853002999,-6.39660293913491E-6,
4.62495348172753));
#31687=CARTESIAN_POINT('Origin',(11.8752146997001,0.,4.));
#31688=CARTESIAN_POINT('',(13.4247853002999,1.36962628664028E-5,4.62502243215823));
#31689=CARTESIAN_POINT('',(13.5252146997001,1.40828270379035E-5,4.62497680637469));
#31690=CARTESIAN_POINT('',(11.8752146997001,-1.68747709936658E-14,4.625));
#31691=CARTESIAN_POINT('Ctrl Pts',(13.5252146997001,1.4082827037902E-5,
4.62497680637469));
#31692=CARTESIAN_POINT('Ctrl Pts',(13.5306325778363,-0.0709123884867814,
4.62491668074428));
#31693=CARTESIAN_POINT('Ctrl Pts',(13.5439218280225,-0.244933372371362,
4.59533688876844));
#31694=CARTESIAN_POINT('Ctrl Pts',(13.5650824502587,-0.482621788093898,
4.43698120905743));
#31695=CARTESIAN_POINT('Ctrl Pts',(13.5886965664085,-0.632205603168059,
4.15553919999523));
#31696=CARTESIAN_POINT('Ctrl Pts',(13.6123106825584,-0.630276944445953,
3.83682113889318));
#31697=CARTESIAN_POINT('Ctrl Pts',(13.6359247987083,-0.477298028416376,
3.55721002779864));
#31698=CARTESIAN_POINT('Ctrl Pts',(13.6595389148582,-0.209931317243796,
3.38371661595291));
#31699=CARTESIAN_POINT('Ctrl Pts',(13.683153031008,0.107746895509167,3.35791980725116));
#31700=CARTESIAN_POINT('Ctrl Pts',(13.7067671471579,0.399602814690774,3.48600198647908));
#31701=CARTESIAN_POINT('Ctrl Pts',(13.7303812633077,0.59569113756138,3.73726736776131));
#31702=CARTESIAN_POINT('Ctrl Pts',(13.7539953794576,0.649017932507905,4.05149845333026));
#31703=CARTESIAN_POINT('Ctrl Pts',(13.7776094956075,0.546803061895555,4.35338757606046));
#31704=CARTESIAN_POINT('Ctrl Pts',(13.8012236117573,0.313543031018869,4.57058490613733));
#31705=CARTESIAN_POINT('Ctrl Pts',(13.8170920131216,0.106300066848774,4.6246481407235));
#31706=CARTESIAN_POINT('Ctrl Pts',(13.8250890424358,0.00164611344283092,
4.62505264870678));
#31707=CARTESIAN_POINT('Ctrl Pts',(13.8252146997001,1.68461488569581E-6,
4.62505238998457));
#31708=CARTESIAN_POINT('Ctrl Pts',(13.4247853002999,1.36962628664097E-5,
4.62502243215823));
#31709=CARTESIAN_POINT('Ctrl Pts',(13.4313784155315,-0.086279884022628,
4.62493973056585));
#31710=CARTESIAN_POINT('Ctrl Pts',(13.445842902813,-0.275670893367246,4.58538934244717));
#31711=CARTESIAN_POINT('Ctrl Pts',(13.4681787621445,-0.513544980480383,
4.40018484937968));
#31712=CARTESIAN_POINT('Ctrl Pts',(13.4917928782944,-0.64195771209056,4.10847422061066));
#31713=CARTESIAN_POINT('Ctrl Pts',(13.5154069944443,-0.616520809113462,
3.79076698974655));
#31714=CARTESIAN_POINT('Ctrl Pts',(13.5390211105941,-0.443330402422436,
3.52320390633144));
#31715=CARTESIAN_POINT('Ctrl Pts',(13.562635226744,-0.163892778617988,3.36990832590288));
#31716=CARTESIAN_POINT('Ctrl Pts',(13.5862493428939,0.154822890495328,3.36761860145296));
#31717=CARTESIAN_POINT('Ctrl Pts',(13.6098634590437,0.43643417612693,3.51688348138565));
#31718=CARTESIAN_POINT('Ctrl Pts',(13.6334775751936,0.613450973283793,3.78193059814177));
#31719=CARTESIAN_POINT('Ctrl Pts',(13.6570916913435,0.643449974253473,4.09923956510808));
#31720=CARTESIAN_POINT('Ctrl Pts',(13.6807058074933,0.519241709620395,4.39276507945606));
#31721=CARTESIAN_POINT('Ctrl Pts',(13.7032703438121,0.281645253009076,4.58329909926801));
#31722=CARTESIAN_POINT('Ctrl Pts',(13.717963508081,0.0892710189108511,4.62495207452848));
#31723=CARTESIAN_POINT('Ctrl Pts',(13.7247853002999,-1.20831421156938E-5,
4.62503091248755));
#31724=CARTESIAN_POINT('Origin',(11.8752146997001,0.,4.));
#31725=CARTESIAN_POINT('',(13.1247853002999,3.84888821539087E-6,4.62495078081483));
#31726=CARTESIAN_POINT('',(13.2252146997001,-9.32440196476731E-6,4.62495874418382));
#31727=CARTESIAN_POINT('',(11.8752146997001,-1.68747709936658E-14,4.625));
#31728=CARTESIAN_POINT('Ctrl Pts',(13.2252146997001,-9.32440196474427E-6,
4.62495874418382));
#31729=CARTESIAN_POINT('Ctrl Pts',(13.2283047411869,-0.040464997295585,
4.62498052751194));
#31730=CARTESIAN_POINT('Ctrl Pts',(13.2392661547237,-0.18396024524725,4.61125364372682));
#31731=CARTESIAN_POINT('Ctrl Pts',(13.2580989403104,-0.413782468289504,
4.50265339583901));
#31732=CARTESIAN_POINT('Ctrl Pts',(13.2817130564603,-0.602786876612853,
4.24601696851145));
#31733=CARTESIAN_POINT('Ctrl Pts',(13.3053271726101,-0.647329213752593,
3.9304208620728));
#31734=CARTESIAN_POINT('Ctrl Pts',(13.32894128876,-0.536734598538914,3.6314998804023));
#31735=CARTESIAN_POINT('Ctrl Pts',(13.3525554049099,-0.297507800394296,
3.42089251764738));
#31736=CARTESIAN_POINT('Ctrl Pts',(13.3761695210598,0.0130188131672444,
3.34907229440132));
#31737=CARTESIAN_POINT('Ctrl Pts',(13.3997836372096,0.320425377524893,3.43325142712992));
#31738=CARTESIAN_POINT('Ctrl Pts',(13.4233977533595,0.551039769569266,3.65325580067535));
#31739=CARTESIAN_POINT('Ctrl Pts',(13.4470118695093,0.649593644862141,3.95635983539258));
#31740=CARTESIAN_POINT('Ctrl Pts',(13.4706259856592,0.592467881122722,4.26992253935193));
#31741=CARTESIAN_POINT('Ctrl Pts',(13.4942401018091,0.393353065302923,4.5187964277335));
#31742=CARTESIAN_POINT('Ctrl Pts',(13.5124363398227,0.1672808180195,4.61476328251587));
#31743=CARTESIAN_POINT('Ctrl Pts',(13.5227612057864,0.0321332374692893,
4.62500403435298));
#31744=CARTESIAN_POINT('Ctrl Pts',(13.5252146997001,1.4082827037902E-5,
4.62497680637469));
#31745=CARTESIAN_POINT('Ctrl Pts',(13.1247853002999,3.84888821536311E-6,
4.62495078081483));
#31746=CARTESIAN_POINT('Ctrl Pts',(13.1290505788821,-0.0558403875021823,
4.6249385719914));
#31747=CARTESIAN_POINT('Ctrl Pts',(13.1411872295142,-0.214751600407627,
4.60383286368317));
#31748=CARTESIAN_POINT('Ctrl Pts',(13.1611952521963,-0.449738236712957,
4.47075670902068));
#31749=CARTESIAN_POINT('Ctrl Pts',(13.1848093683461,-0.619294173608025,
4.2008758003961));
#31750=CARTESIAN_POINT('Ctrl Pts',(13.208423484496,-0.64043195068177,3.88285360784221));
#31751=CARTESIAN_POINT('Ctrl Pts',(13.2320376006459,-0.508085752511173,
3.59290636366459));
#31752=CARTESIAN_POINT('Ctrl Pts',(13.2556517167957,-0.253973266794505,
3.40052194335125));
#31753=CARTESIAN_POINT('Ctrl Pts',(13.2792658329456,0.0610056803032868,
3.3518066124833));
#31754=CARTESIAN_POINT('Ctrl Pts',(13.3028799490955,0.361364191435218,3.45843533922715));
#31755=CARTESIAN_POINT('Ctrl Pts',(13.3264940652453,0.575119258511334,3.69485380694));
#31756=CARTESIAN_POINT('Ctrl Pts',(13.3501081813952,0.65104299168552,4.00440268404554));
#31757=CARTESIAN_POINT('Ctrl Pts',(13.3737222975451,0.570939739771795,4.31289642727099));
#31758=CARTESIAN_POINT('Ctrl Pts',(13.3973364136949,0.354006804717113,4.54640236352309));
#31759=CARTESIAN_POINT('Ctrl Pts',(13.4143574146132,0.136489422610972,4.62032507485564));
#31760=CARTESIAN_POINT('Ctrl Pts',(13.4235070434815,0.0167440814458925,
4.62503846613771));
#31761=CARTESIAN_POINT('Ctrl Pts',(13.4247853002999,1.36962628664097E-5,
4.62502243215823));
#31762=CARTESIAN_POINT('Origin',(11.8752146997001,0.,4.));
#31763=CARTESIAN_POINT('',(12.8247853002999,-1.55438223423121E-5,4.62499607812274));
#31764=CARTESIAN_POINT('',(12.9252146997001,-9.4222586321007E-6,4.62504029123831));
#31765=CARTESIAN_POINT('',(11.8752146997001,-1.68747709936658E-14,4.625));
#31766=CARTESIAN_POINT('Ctrl Pts',(12.9252146997001,-9.42225863212465E-6,
4.62504029123832));
#31767=CARTESIAN_POINT('Ctrl Pts',(12.9259769045375,-0.00998466834883174,
4.6250476064301));
#31768=CARTESIAN_POINT('Ctrl Pts',(12.9346104814248,-0.122971475467856,
4.62239759066569));
#31769=CARTESIAN_POINT('Ctrl Pts',(12.9511154303622,-0.336107011072318,
4.55759164674784));
#31770=CARTESIAN_POINT('Ctrl Pts',(12.974729546512,-0.56049590900091,4.33124115596169));
#31771=CARTESIAN_POINT('Ctrl Pts',(12.9983436626619,-0.650558060547343,
4.02550641626558));
#31772=CARTESIAN_POINT('Ctrl Pts',(13.0219577788117,-0.584709444123524,
3.71365888635357));
#31773=CARTESIAN_POINT('Ctrl Pts',(13.0455718949616,-0.378731139057797,
3.47043499764384));
#31774=CARTESIAN_POINT('Ctrl Pts',(13.0691860111115,-0.0819872800401352,
3.35412504823007));
#31775=CARTESIAN_POINT('Ctrl Pts',(13.0928001272613,0.234405401379786,3.39260352716186));
#31776=CARTESIAN_POINT('Ctrl Pts',(13.1164142434112,0.494621196584012,3.57664879910166));
#31777=CARTESIAN_POINT('Ctrl Pts',(13.1400283595611,0.636297578801308,3.86215313342763));
#31778=CARTESIAN_POINT('Ctrl Pts',(13.1636424757109,0.625480816776257,4.18069342892634));
#31779=CARTESIAN_POINT('Ctrl Pts',(13.1872565918608,0.464763222827219,4.45592928631477));
#31780=CARTESIAN_POINT('Ctrl Pts',(13.2077806665239,0.228267895462889,4.60018049807294));
#31781=CARTESIAN_POINT('Ctrl Pts',(13.220433369137,0.0625891701764018,4.62492503806923));
#31782=CARTESIAN_POINT('Ctrl Pts',(13.2252146997001,-9.32440196474427E-6,
4.62495874418382));
#31783=CARTESIAN_POINT('Ctrl Pts',(12.8247853002999,-1.55438223423052E-5,
4.62499607812274));
#31784=CARTESIAN_POINT('Ctrl Pts',(12.8267227422326,-0.0253767156259869,
4.62502109614712));
#31785=CARTESIAN_POINT('Ctrl Pts',(12.8365315562153,-0.153759343851268,
4.61735081595804));
#31786=CARTESIAN_POINT('Ctrl Pts',(12.854211742248,-0.376327535803878,4.5312757721487));
#31787=CARTESIAN_POINT('Ctrl Pts',(12.8778258583979,-0.583405888470749,
4.28898776831928));
#31788=CARTESIAN_POINT('Ctrl Pts',(12.9014399745477,-0.650666957548692,
3.97744183415536));
#31789=CARTESIAN_POINT('Ctrl Pts',(12.9250540906976,-0.561991161265395,
3.67130212143154));
#31790=CARTESIAN_POINT('Ctrl Pts',(12.9486682068475,-0.338630270727757,
3.44393714350224));
#31791=CARTESIAN_POINT('Ctrl Pts',(12.9722823229973,-0.0341142786054444,
3.34983650006563));
#31792=CARTESIAN_POINT('Ctrl Pts',(12.9958964391472,0.278577437919422,3.41155206540036));
#31793=CARTESIAN_POINT('Ctrl Pts',(13.0195105552971,0.524506132150044,3.61429327464512));
#31794=CARTESIAN_POINT('Ctrl Pts',(13.0431246714469,0.644733280558021,3.90947178565704));
#31795=CARTESIAN_POINT('Ctrl Pts',(13.0667387875968,0.61044561006836,4.22634601343335));
#31796=CARTESIAN_POINT('Ctrl Pts',(13.0903529037467,0.429860399609997,4.4889748434194));
#31797=CARTESIAN_POINT('Ctrl Pts',(13.1097017413144,0.197481915229314,4.60814700801091));
#31798=CARTESIAN_POINT('Ctrl Pts',(13.1211792068321,0.0472175377905832,
4.6249611028038));
#31799=CARTESIAN_POINT('Ctrl Pts',(13.1247853002999,3.84888821536311E-6,
4.62495078081483));
#31800=CARTESIAN_POINT('Origin',(11.8752146997001,0.,4.));
#31801=CARTESIAN_POINT('',(12.5247853002999,3.80998376854277E-6,4.62503871776264));
#31802=CARTESIAN_POINT('',(12.6252146997001,1.49489494596481E-5,4.6250110476872));
#31803=CARTESIAN_POINT('',(11.8752146997001,-1.68747709936658E-14,4.625));
#31804=CARTESIAN_POINT('',(12.5,0.310062960217711,4.54266560670548));
#31805=CARTESIAN_POINT('Ctrl Pts',(12.5,0.310062960217722,4.54266560670548));
#31806=CARTESIAN_POINT('Ctrl Pts',(12.50787137205,0.220600394030941,4.59378185169648));
#31807=CARTESIAN_POINT('Ctrl Pts',(12.5161331388166,0.113220056708515,4.6237347594226));
#31808=CARTESIAN_POINT('Ctrl Pts',(12.5243949055832,0.00511234815255113,
4.6250406321328));
#31809=CARTESIAN_POINT('Ctrl Pts',(12.5247853002999,3.80998376856706E-6,
4.62503871776264));
#31810=CARTESIAN_POINT('',(12.5,0.310062960217774,3.45733439329455));
#31811=CARTESIAN_POINT('Origin',(12.5,0.,4.));
#31812=CARTESIAN_POINT('Ctrl Pts',(12.5,0.310093463203755,3.45730861053195));
#31813=CARTESIAN_POINT('Ctrl Pts',(12.5008157411716,0.319367492808711,3.46259780682489));
#31814=CARTESIAN_POINT('Ctrl Pts',(12.5095028543931,0.416666480413896,3.52147574364868));
#31815=CARTESIAN_POINT('Ctrl Pts',(12.5260613396645,0.569511032758309,3.68451895614546));
#31816=CARTESIAN_POINT('Ctrl Pts',(12.5496754558144,0.651018771792273,3.99264764559437));
#31817=CARTESIAN_POINT('Ctrl Pts',(12.5732895719643,0.576495013506714,4.3025367374363));
#31818=CARTESIAN_POINT('Ctrl Pts',(12.5969036881141,0.363815091701307,4.53992168461618));
#31819=CARTESIAN_POINT('Ctrl Pts',(12.6142120640261,0.144017971622128,4.61907377583531));
#31820=CARTESIAN_POINT('Ctrl Pts',(12.6236490678881,0.0205077016108913,
4.62503160004571));
#31821=CARTESIAN_POINT('Ctrl Pts',(12.6252146997001,1.49489494596471E-5,
4.6250110476872));
#31822=CARTESIAN_POINT('Origin',(11.8752146997001,0.,4.));
#31823=CARTESIAN_POINT('Ctrl Pts',(12.6252146997001,1.49489494596471E-5,
4.6250110476872));
#31824=CARTESIAN_POINT('Ctrl Pts',(12.631520439938,-0.0825216819810338,
4.62492827098767));
#31825=CARTESIAN_POINT('Ctrl Pts',(12.6456975522259,-0.268159494659544,
4.5879440580038));
#31826=CARTESIAN_POINT('Ctrl Pts',(12.6677460365637,-0.506235857616531,
4.40939182910775));
#31827=CARTESIAN_POINT('Ctrl Pts',(12.6913601527136,-0.639894509617229,
4.12004729681268));
#31828=CARTESIAN_POINT('Ctrl Pts',(12.7149742688635,-0.620198095551099,
3.8019325752266));
#31829=CARTESIAN_POINT('Ctrl Pts',(12.7385883850133,-0.451866840211785,
3.53128609963859));
#31830=CARTESIAN_POINT('Ctrl Pts',(12.7622025011632,-0.17524257447904,3.37297016902465));
#31831=CARTESIAN_POINT('Ctrl Pts',(12.7858166173131,0.143379805101228,3.36492630429559));
#31832=CARTESIAN_POINT('Ctrl Pts',(12.809430733463,0.42764021116234,3.50908227080648));
#31833=CARTESIAN_POINT('Ctrl Pts',(12.8330448496128,0.609413666055986,3.77089008898231));
#31834=CARTESIAN_POINT('Ctrl Pts',(12.8566589657627,0.645136892431096,4.08760569204938));
#31835=CARTESIAN_POINT('Ctrl Pts',(12.8802730819125,0.526248572038732,4.38332598125533));
#31836=CARTESIAN_POINT('Ctrl Pts',(12.903124993225,0.289149347937084,4.5805996458561));
#31837=CARTESIAN_POINT('Ctrl Pts',(12.9181055324875,0.0930307802739178,
4.62497206165088));
#31838=CARTESIAN_POINT('Ctrl Pts',(12.9252146997001,-9.42225863212465E-6,
4.62504029123832));
#31839=CARTESIAN_POINT('Ctrl Pts',(12.5247853002999,3.80998376856706E-6,
4.62503871776264));
#31840=CARTESIAN_POINT('Ctrl Pts',(12.5322662776332,-0.0978890574527522,
4.62500203345524));
#31841=CARTESIAN_POINT('Ctrl Pts',(12.5476186270164,-0.298862923743373,
4.57698368148067));
#31842=CARTESIAN_POINT('Ctrl Pts',(12.5708423484496,-0.535054221536356,
4.37092866956447));
#31843=CARTESIAN_POINT('Ctrl Pts',(12.5944564645995,-0.647009713430093,
4.07251155115386));
#31844=CARTESIAN_POINT('Ctrl Pts',(12.6180705807493,-0.603894380709874,
3.75671714932517));
#31845=CARTESIAN_POINT('Ctrl Pts',(12.6416846968992,-0.416056506175611,
3.49922677321964));
#31846=CARTESIAN_POINT('Ctrl Pts',(12.6652988130491,-0.128505496873939,
3.36175035317655));
#31847=CARTESIAN_POINT('Ctrl Pts',(12.6889129291989,0.189841674427298,3.37723482234205));
#31848=CARTESIAN_POINT('Ctrl Pts',(12.7125270453488,0.462692468193658,3.54196933898577));
#31849=CARTESIAN_POINT('Ctrl Pts',(12.7361411614987,0.624655556881011,3.81647407445394));
#31850=CARTESIAN_POINT('Ctrl Pts',(12.7597552776485,0.636915702199809,4.13496208375113));
#31851=CARTESIAN_POINT('Ctrl Pts',(12.7833693937984,0.496534514683115,4.42110548633398));
#31852=CARTESIAN_POINT('Ctrl Pts',(12.8050460680155,0.258436396781676,4.5911312751119));
#31853=CARTESIAN_POINT('Ctrl Pts',(12.8188513701827,0.0776597756952025,
4.62491945378327));
#31854=CARTESIAN_POINT('Ctrl Pts',(12.8247853002999,-1.55438223423052E-5,
4.62499607812274));
#31855=CARTESIAN_POINT('Ctrl Pts',(12.5,-0.186196943290592,3.58169363627332));
#31856=CARTESIAN_POINT('Ctrl Pts',(12.50787137205,-0.117235947257613,3.55099764935784));
#31857=CARTESIAN_POINT('Ctrl Pts',(12.5236141161499,0.0360970477778841,
3.52440632583991));
#31858=CARTESIAN_POINT('Ctrl Pts',(12.5472282322997,0.257537368848111,3.59853698535937));
#31859=CARTESIAN_POINT('Ctrl Pts',(12.5708423484496,0.417223782598737,3.76887858727216));
#31860=CARTESIAN_POINT('Ctrl Pts',(12.5944564645995,0.476936352215019,3.99461366516243));
#31861=CARTESIAN_POINT('Ctrl Pts',(12.6180705807493,0.422340246895018,4.22163841384584));
#31862=CARTESIAN_POINT('Ctrl Pts',(12.6416846968992,0.266530936180377,4.39554662614981));
#31863=CARTESIAN_POINT('Ctrl Pts',(12.6652988130491,0.0468439715927196,
4.47465904879863));
#31864=CARTESIAN_POINT('Ctrl Pts',(12.6889129291989,-0.184068700558194,
4.44001626345752));
#31865=CARTESIAN_POINT('Ctrl Pts',(12.7125270453488,-0.37086838928987,4.29992045400434));
#31866=CARTESIAN_POINT('Ctrl Pts',(12.7361411614987,-0.468786717745582,
4.08794664964497));
#31867=CARTESIAN_POINT('Ctrl Pts',(12.7597552776485,-0.454357124800734,
3.85489580461101));
#31868=CARTESIAN_POINT('Ctrl Pts',(12.7833693937984,-0.331037647139153,
3.65662019659523));
#31869=CARTESIAN_POINT('Ctrl Pts',(12.8069835099483,-0.128382710063344,
3.54063794582746));
#31870=CARTESIAN_POINT('Ctrl Pts',(12.8305976260981,0.10504004521716,3.53474501052695));
#31871=CARTESIAN_POINT('Ctrl Pts',(12.854211742248,0.31328921869753,3.64035367159283));
#31872=CARTESIAN_POINT('Ctrl Pts',(12.8778258583979,0.446456451752615,3.83215407918844));
#31873=CARTESIAN_POINT('Ctrl Pts',(12.9014399745477,0.47262728739502,4.06417992999538));
#31874=CARTESIAN_POINT('Ctrl Pts',(12.9250540906976,0.385529703875575,4.28082461386765));
#31875=CARTESIAN_POINT('Ctrl Pts',(12.9486682068475,0.206037242841946,4.43016772408018));
#31876=CARTESIAN_POINT('Ctrl Pts',(12.9722823229973,-0.0228334776507366,
4.47641814468844));
#31877=CARTESIAN_POINT('Ctrl Pts',(12.9958964391472,-0.24623199631158,4.40849164040747));
#31878=CARTESIAN_POINT('Ctrl Pts',(13.0195105552971,-0.410619302934066,
4.24266727085754));
#31879=CARTESIAN_POINT('Ctrl Pts',(13.0431246714469,-0.476598835156983,
4.01868600055616));
#31880=CARTESIAN_POINT('Ctrl Pts',(13.0667387875968,-0.428358138764893,
3.79022650014263));
#31881=CARTESIAN_POINT('Ctrl Pts',(13.0903529037467,-0.277458432473742,
3.61204067927388));
#31882=CARTESIAN_POINT('Ctrl Pts',(13.1139670198965,-0.060063881357403,
3.52683201033335));
#31883=CARTESIAN_POINT('Ctrl Pts',(13.1375811360464,0.171725397050831,3.55502134399878));
#31884=CARTESIAN_POINT('Ctrl Pts',(13.1611952521963,0.362359488617447,3.68985291022187));
#31885=CARTESIAN_POINT('Ctrl Pts',(13.1848093683461,0.466151606229838,3.89901338554908));
#31886=CARTESIAN_POINT('Ctrl Pts',(13.208423484496,0.458227246370285,4.13237600603144));
#31887=CARTESIAN_POINT('Ctrl Pts',(13.2320376006459,0.34048553704322,4.3340137951542));
#31888=CARTESIAN_POINT('Ctrl Pts',(13.2556517167957,0.141144098528766,4.45560285308526));
#31889=CARTESIAN_POINT('Ctrl Pts',(13.2792658329456,-0.0920235057499227,
4.46800351566886));
#31890=CARTESIAN_POINT('Ctrl Pts',(13.3028799490955,-0.30313703626889,4.36824387779166));
#31891=CARTESIAN_POINT('Ctrl Pts',(13.3264940652453,-0.441601665806575,
4.18023203113149));
#31892=CARTESIAN_POINT('Ctrl Pts',(13.3501081813952,-0.47423338199515,3.94902632355453));
#31893=CARTESIAN_POINT('Ctrl Pts',(13.3737222975451,-0.393211766889608,
3.73003681238273));
#31894=CARTESIAN_POINT('Ctrl Pts',(13.3973364136949,-0.217954214568861,
3.57574585842847));
#31895=CARTESIAN_POINT('Ctrl Pts',(13.4209505298448,0.00953758252632317,
3.52313036287841));
#31896=CARTESIAN_POINT('Ctrl Pts',(13.4445646459947,0.234743631574736,3.58479999551538));
#31897=CARTESIAN_POINT('Ctrl Pts',(13.4681787621445,0.403691735186444,3.74597519957476));
#31898=CARTESIAN_POINT('Ctrl Pts',(13.4917928782944,0.475892304226004,3.96802921540861));
#31899=CARTESIAN_POINT('Ctrl Pts',(13.5154069944443,0.434041969710506,4.19774525232923));
#31900=CARTESIAN_POINT('Ctrl Pts',(13.5390211105941,0.288170455640921,4.38007026295756));
#31901=CARTESIAN_POINT('Ctrl Pts',(13.562635226744,0.0732368858249759,4.47130878927046));
#31902=CARTESIAN_POINT('Ctrl Pts',(13.5862493428939,-0.159248413505658,
4.44959488329479));
#31903=CARTESIAN_POINT('Ctrl Pts',(13.6098634590437,-0.353568721957589,
4.32013243375547));
#31904=CARTESIAN_POINT('Ctrl Pts',(13.6334775751936,-0.46315382488092,4.1139480179165));
#31905=CARTESIAN_POINT('Ctrl Pts',(13.6570916913435,-0.461740889501104,
3.88045516635315));
#31906=CARTESIAN_POINT('Ctrl Pts',(13.6807058074933,-0.349668535617837,
3.67561206636528));
#31907=CARTESIAN_POINT('Ctrl Pts',(13.7043199236432,-0.153795683012805,
3.5485107928471));
#31908=CARTESIAN_POINT('Ctrl Pts',(13.7279340397931,0.0789353756500159,
3.5296120507922));
#31909=CARTESIAN_POINT('Ctrl Pts',(13.7515481559429,0.292749022042461,3.62344505529457));
#31910=CARTESIAN_POINT('Ctrl Pts',(13.7751622720928,0.436403327377467,3.80752207362193));
#31911=CARTESIAN_POINT('Ctrl Pts',(13.7987763882427,0.475470537355291,4.03772776690975));
#31912=CARTESIAN_POINT('Ctrl Pts',(13.8223905043925,0.400587923144683,4.25889173822189));
#31913=CARTESIAN_POINT('Ctrl Pts',(13.8460046205424,0.229701624524423,4.41801050223621));
#31914=CARTESIAN_POINT('Ctrl Pts',(13.8696187366923,0.00376573255618155,
4.47695013947711));
#31915=CARTESIAN_POINT('Ctrl Pts',(13.8932328528421,-0.223072643433687,
4.42158535558109));
#31916=CARTESIAN_POINT('Ctrl Pts',(13.916846968992,-0.396450107540549,4.26518470642179));
#31917=CARTESIAN_POINT('Ctrl Pts',(13.9404610851419,-0.474815543552022,
4.04523069632808));
#31918=CARTESIAN_POINT('Ctrl Pts',(13.9640752012917,-0.439388129199652,
3.81443683499316));
#31919=CARTESIAN_POINT('Ctrl Pts',(13.9876893174416,-0.298658290955197,
3.62811447792009));
#31920=CARTESIAN_POINT('Ctrl Pts',(14.0113034335915,-0.0863529142219465,
3.53091707503438));
#31921=CARTESIAN_POINT('Ctrl Pts',(14.0349175497413,0.146647539536438,3.54613866056158));
#31922=CARTESIAN_POINT('Ctrl Pts',(14.0585316658912,0.344502889581789,3.6701312755675));
#31923=CARTESIAN_POINT('Ctrl Pts',(14.0821457820411,0.459795723937725,3.87317922671144));
#31924=CARTESIAN_POINT('Ctrl Pts',(14.1057598981909,0.464895312258427,4.10662065901627));
#31925=CARTESIAN_POINT('Ctrl Pts',(14.1293740143408,0.358579502702881,4.31450970816539));
#31926=CARTESIAN_POINT('Ctrl Pts',(14.1529881304907,0.166327619131383,4.44702431634421));
#31927=CARTESIAN_POINT('Ctrl Pts',(14.1766022466405,-0.0657858362277661,
4.47240643522367));
#31928=CARTESIAN_POINT('Ctrl Pts',(14.2002163627904,-0.282133257977474,
4.38457306332079));
#31929=CARTESIAN_POINT('Ctrl Pts',(14.2238304789403,-0.430865480427841,
4.20457407964992));
#31930=CARTESIAN_POINT('Ctrl Pts',(14.2474445950901,-0.476337791093329,
3.97554749368157));
#31931=CARTESIAN_POINT('Ctrl Pts',(14.27105871124,-0.407652434174819,3.75238112107461));
#31932=CARTESIAN_POINT('Ctrl Pts',(14.2946728273899,-0.241270333599833,
3.58855833656088));
#31933=CARTESIAN_POINT('Ctrl Pts',(14.3182869435397,-0.0170661180132474,
3.52334041087493));
#31934=CARTESIAN_POINT('Ctrl Pts',(14.3419010596896,0.211228111558234,3.57235727391142));
#31935=CARTESIAN_POINT('Ctrl Pts',(14.3655151758395,0.388900053764453,3.72386169322071));
#31936=CARTESIAN_POINT('Ctrl Pts',(14.3891292919893,0.473369390821204,3.94154458004181));
#31937=CARTESIAN_POINT('Ctrl Pts',(14.4127434081392,0.444392458083208,4.17323671518384));
#31938=CARTESIAN_POINT('Ctrl Pts',(14.4363575242891,0.308913779199362,4.3634114655727));
#31939=CARTESIAN_POINT('Ctrl Pts',(14.4599716404389,0.0994017626770733,
4.46649212840691));
#31940=CARTESIAN_POINT('Ctrl Pts',(14.4835857565888,-0.133932578240045,
4.45777470525894));
#31941=CARTESIAN_POINT('Ctrl Pts',(14.5071998727387,-0.335169044432007,
4.33934838727104));
#31942=CARTESIAN_POINT('Ctrl Pts',(14.5308139888885,-0.456079915900645,
4.13959486595487));
#31943=CARTESIAN_POINT('Ctrl Pts',(14.5544281050384,-0.467688060597361,
3.90638646324521));
#31944=CARTESIAN_POINT('Ctrl Pts',(14.5780422211883,-0.367211505836647,
3.69561319629505));
#31945=CARTESIAN_POINT('Ctrl Pts',(14.6016563373381,-0.178730157419731,
3.55778834579073));
#31946=CARTESIAN_POINT('Ctrl Pts',(14.625270453488,0.0525851174261518,3.52594259660587));
#31947=CARTESIAN_POINT('Ctrl Pts',(14.6488845696379,0.271298002813252,3.60770800421126));
#31948=CARTESIAN_POINT('Ctrl Pts',(14.6724986857877,0.424992433239313,3.78348891949988));
#31949=CARTESIAN_POINT('Ctrl Pts',(14.6961128019376,0.476834468501385,4.01115822240469));
#31950=CARTESIAN_POINT('Ctrl Pts',(14.7197269180875,0.414399804028447,4.23615337970372));
#31951=CARTESIAN_POINT('Ctrl Pts',(14.7433410342373,0.252651341641402,4.40455273546398));
#31952=CARTESIAN_POINT('Ctrl Pts',(14.7669551503872,0.0303532266559796,
4.47599821226155));
#31953=CARTESIAN_POINT('Ctrl Pts',(14.7905692665371,-0.199219250862459,
4.43336740322118));
#31954=CARTESIAN_POINT('Ctrl Pts',(14.8141833826869,-0.381047447081096,
4.28687708064914));
#31955=CARTESIAN_POINT('Ctrl Pts',(14.8377974988368,-0.471554972144783,
4.07163466550741));
#31956=CARTESIAN_POINT('Ctrl Pts',(14.8614116149867,-0.449051060899263,
3.83922451083896));
#31957=CARTESIAN_POINT('Ctrl Pts',(14.8850257311365,-0.318928946727196,
3.64534530693059));
#31958=CARTESIAN_POINT('Ctrl Pts',(14.9086398472864,-0.112373269271187,
3.53646160000302));
#31959=CARTESIAN_POINT('Ctrl Pts',(14.9322539634362,0.121113399391719,3.5386680312482));
#31960=CARTESIAN_POINT('Ctrl Pts',(14.9558680795861,0.325574495333277,3.65143602219853));
#31961=CARTESIAN_POINT('Ctrl Pts',(14.979482195736,0.452009190454857,3.84773949289016));
#31962=CARTESIAN_POINT('Ctrl Pts',(15.0030963118858,0.470117180575255,4.08053390545391));
#31963=CARTESIAN_POINT('Ctrl Pts',(15.0267104280357,0.375557372208547,4.29402641177155));
#31964=CARTESIAN_POINT('Ctrl Pts',(15.0503245441856,0.190994688421392,4.43705643304037));
#31965=CARTESIAN_POINT('Ctrl Pts',(15.0739386603355,-0.0393454023191647,
4.47533644032795));
#31966=CARTESIAN_POINT('Ctrl Pts',(15.0975527764853,-0.260245916509526,
4.39971253597763));
#31967=CARTESIAN_POINT('Ctrl Pts',(15.1211668926352,-0.418792603204267,
4.22826540530875));
#31968=CARTESIAN_POINT('Ctrl Pts',(15.1369096367351,-0.457530945318996,
4.07754232577813));
#31969=CARTESIAN_POINT('Ctrl Pts',(15.1447810087851,-0.457870370902723,
4.00205890126089));
#31970=CARTESIAN_POINT('Ctrl Pts',(12.4850729970717,-0.208850989443975,
3.53079950502365));
#31971=CARTESIAN_POINT('Ctrl Pts',(12.4929443691216,-0.131499707516366,
3.49636882573344));
#31972=CARTESIAN_POINT('Ctrl Pts',(12.5086871132215,0.0404888716816997,
3.46654221242176));
#31973=CARTESIAN_POINT('Ctrl Pts',(12.5323012293714,0.288871199237585,3.54969213591223));
#31974=CARTESIAN_POINT('Ctrl Pts',(12.5559153455212,0.467986199318594,3.74075871022993));
#31975=CARTESIAN_POINT('Ctrl Pts',(12.5795294616711,0.534963825407437,3.99395832530641));
#31976=CARTESIAN_POINT('Ctrl Pts',(12.603143577821,0.473725169098917,4.24860452170932));
#31977=CARTESIAN_POINT('Ctrl Pts',(12.6267576939708,0.298958988020687,4.4436716456386));
#31978=CARTESIAN_POINT('Ctrl Pts',(12.6503718101207,0.0525433427838623,
4.53240944903922));
#31979=CARTESIAN_POINT('Ctrl Pts',(12.6739859262706,-0.206463809544117,
4.49355177571912));
#31980=CARTESIAN_POINT('Ctrl Pts',(12.6976000424205,-0.41599087873209,4.33641091237214));
#31981=CARTESIAN_POINT('Ctrl Pts',(12.7212141585703,-0.525822648369464,
4.09864686536754));
#31982=CARTESIAN_POINT('Ctrl Pts',(12.7448282747202,-0.509637448384189,
3.8372413948162));
#31983=CARTESIAN_POINT('Ctrl Pts',(12.76844239087,-0.37131404483003,3.61484216427635));
#31984=CARTESIAN_POINT('Ctrl Pts',(12.7920565070199,-0.144002664868576,
3.48474868689319));
#31985=CARTESIAN_POINT('Ctrl Pts',(12.8156706231698,0.117819965178516,3.47813877511649));
#31986=CARTESIAN_POINT('Ctrl Pts',(12.8392847393197,0.351406216185799,3.59659653799738));
#31987=CARTESIAN_POINT('Ctrl Pts',(12.8628988554695,0.500775523187073,3.81173274911973));
#31988=CARTESIAN_POINT('Ctrl Pts',(12.8865129716194,0.530130489073712,4.07198851734671));
#31989=CARTESIAN_POINT('Ctrl Pts',(12.9101270877692,0.432435993263294,4.31499173633021));
#31990=CARTESIAN_POINT('Ctrl Pts',(12.9337412039191,0.231105201134755,4.48250499290311));
#31991=CARTESIAN_POINT('Ctrl Pts',(12.957355320069,-0.0256115611541523,
4.53438256906268));
#31992=CARTESIAN_POINT('Ctrl Pts',(12.9809694362189,-0.276190334565159,
4.45819164252092));
#31993=CARTESIAN_POINT('Ctrl Pts',(13.0045835523687,-0.460578171623014,
4.27219189922559));
#31994=CARTESIAN_POINT('Ctrl Pts',(13.0281976685186,-0.534585243620437,
4.0209594724593));
#31995=CARTESIAN_POINT('Ctrl Pts',(13.0518117846684,-0.480475240551103,
3.76470396221295));
#31996=CARTESIAN_POINT('Ctrl Pts',(13.0754259008183,-0.311216001335094,
3.5648387853972));
#31997=CARTESIAN_POINT('Ctrl Pts',(13.0990400169682,-0.0673716809183137,
3.46926302296559));
#31998=CARTESIAN_POINT('Ctrl Pts',(13.122654133118,0.19261873182715,3.50088207171981));
#31999=CARTESIAN_POINT('Ctrl Pts',(13.1462682492679,0.406446724606302,3.65211820651514));
#32000=CARTESIAN_POINT('Ctrl Pts',(13.1698823654178,0.522866930420328,3.88672663484193));
#32001=CARTESIAN_POINT('Ctrl Pts',(13.1934964815676,0.513978436505609,4.14848181366307));
#32002=CARTESIAN_POINT('Ctrl Pts',(13.2171105977175,0.381911432304553,4.37465229220773));
#32003=CARTESIAN_POINT('Ctrl Pts',(13.2407247138674,0.158316694737061,4.51103474084347));
#32004=CARTESIAN_POINT('Ctrl Pts',(13.2643388300172,-0.103219740820234,
4.52494415635039));
#32005=CARTESIAN_POINT('Ctrl Pts',(13.2879529461671,-0.340018846942428,
4.41304705047411));
#32006=CARTESIAN_POINT('Ctrl Pts',(13.311567062317,-0.495330069408668,4.20216034359148));
#32007=CARTESIAN_POINT('Ctrl Pts',(13.3351811784669,-0.531931992580964,
3.94282450306062));
#32008=CARTESIAN_POINT('Ctrl Pts',(13.3587952946167,-0.44105271077271,3.69719116838925));
#32009=CARTESIAN_POINT('Ctrl Pts',(13.3824094107666,-0.244472076510672,
3.5241280781681));
#32010=CARTESIAN_POINT('Ctrl Pts',(13.4060235269164,0.0106979927399635,
3.46511100671938));
#32011=CARTESIAN_POINT('Ctrl Pts',(13.4296376430663,0.263304213558122,3.53428380605355));
#32012=CARTESIAN_POINT('Ctrl Pts',(13.4532517592162,0.452807746647384,3.71506873327496));
#32013=CARTESIAN_POINT('Ctrl Pts',(13.476865875366,0.533792751104717,3.96413942206993));
#32014=CARTESIAN_POINT('Ctrl Pts',(13.5004799915159,0.486850606847911,4.22180434800346));
#32015=CARTESIAN_POINT('Ctrl Pts',(13.5240941076658,0.323231325528255,4.42631231788287));
#32016=CARTESIAN_POINT('Ctrl Pts',(13.5477082238157,0.0821474069231642,
4.52865157307741));
#32017=CARTESIAN_POINT('Ctrl Pts',(13.5713223399655,-0.178623709606947,
4.50429579866153));
#32018=CARTESIAN_POINT('Ctrl Pts',(13.5949364561154,-0.396586410669692,
4.35908202552279));
#32019=CARTESIAN_POINT('Ctrl Pts',(13.6185505722652,-0.519504417643299,
4.12781174527607));
#32020=CARTESIAN_POINT('Ctrl Pts',(13.6421646884151,-0.517919574482721,
3.86591049053316));
#32021=CARTESIAN_POINT('Ctrl Pts',(13.665778804565,-0.392211699884016,3.6361447201764));
#32022=CARTESIAN_POINT('Ctrl Pts',(13.6893929207148,-0.172507561089802,
3.49357940054904));
#32023=CARTESIAN_POINT('Ctrl Pts',(13.7130070368647,0.0885392156030666,
3.47238130294519));
#32024=CARTESIAN_POINT('Ctrl Pts',(13.7366211530146,0.328366952925232,3.57763069902274));
#32025=CARTESIAN_POINT('Ctrl Pts',(13.7602352691644,0.489499264105438,3.78410383833506));
#32026=CARTESIAN_POINT('Ctrl Pts',(13.7838493853143,0.533319669072828,4.04231799571659));
#32027=CARTESIAN_POINT('Ctrl Pts',(13.8074635014642,0.449326302728307,4.29039035083475));
#32028=CARTESIAN_POINT('Ctrl Pts',(13.831077617614,0.257648760022572,4.46886863686992));
#32029=CARTESIAN_POINT('Ctrl Pts',(13.8546917337639,0.00422389839726028,
4.53497929012603));
#32030=CARTESIAN_POINT('Ctrl Pts',(13.8783058499138,-0.25021324988294,4.47287843233165));
#32031=CARTESIAN_POINT('Ctrl Pts',(13.9019199660636,-0.444685051009628,
4.29744896636227));
#32032=CARTESIAN_POINT('Ctrl Pts',(13.9255340822135,-0.532584984058807,
4.05073378496132));
#32033=CARTESIAN_POINT('Ctrl Pts',(13.9491481983634,-0.492847218174075,
3.79185989881933));
#32034=CARTESIAN_POINT('Ctrl Pts',(13.9727623145132,-0.334995185577738,
3.58286823685896));
#32035=CARTESIAN_POINT('Ctrl Pts',(13.9963764306631,-0.0968592247428986,
3.47384510573062));
#32036=CARTESIAN_POINT('Ctrl Pts',(14.019990546813,0.164489723571401,3.49091865775613));
#32037=CARTESIAN_POINT('Ctrl Pts',(14.0436046629628,0.386417564563212,3.62999709733779));
#32038=CARTESIAN_POINT('Ctrl Pts',(14.0672187791127,0.515737746224078,3.85774930825782));
#32039=CARTESIAN_POINT('Ctrl Pts',(14.0908328952626,0.521457786777448,4.11959288770904));
#32040=CARTESIAN_POINT('Ctrl Pts',(14.1144470114124,0.402206838685568,4.35277519909424));
#32041=CARTESIAN_POINT('Ctrl Pts',(14.1380611275623,0.186564221804844,4.50141247822903));
#32042=CARTESIAN_POINT('Ctrl Pts',(14.1616752437122,-0.0737898095680628,
4.52988276645436));
#32043=CARTESIAN_POINT('Ctrl Pts',(14.185289359862,-0.316459599402161,4.43136296100575));
#32044=CARTESIAN_POINT('Ctrl Pts',(14.2089034760119,-0.483287643257218,
4.22946401908862));
#32045=CARTESIAN_POINT('Ctrl Pts',(14.2325175921618,-0.53429243907693,3.97257242762026));
#32046=CARTESIAN_POINT('Ctrl Pts',(14.2561317083116,-0.457250332481466,
3.72225404480531));
#32047=CARTESIAN_POINT('Ctrl Pts',(14.2797458244615,-0.270625000632592,
3.53849941363631));
#32048=CARTESIAN_POINT('Ctrl Pts',(14.3033599406114,-0.0191425034699505,
3.46534661065105));
#32049=CARTESIAN_POINT('Ctrl Pts',(14.3269740567612,0.236927627906706,3.52032721432634));
#32050=CARTESIAN_POINT('Ctrl Pts',(14.3505881729111,0.436216403922163,3.69026474025285));
#32051=CARTESIAN_POINT('Ctrl Pts',(14.374202289061,0.530962882087739,3.93443247734966));
#32052=CARTESIAN_POINT('Ctrl Pts',(14.3978164052108,0.498460409348769,4.19431392768733));
#32053=CARTESIAN_POINT('Ctrl Pts',(14.4214305213607,0.346498429557861,4.40762669256976));
#32054=CARTESIAN_POINT('Ctrl Pts',(14.4450446375106,0.111495689030631,4.52324888295055));
#32055=CARTESIAN_POINT('Ctrl Pts',(14.4686587536604,-0.150227769531968,
4.51347083601981));
#32056=CARTESIAN_POINT('Ctrl Pts',(14.4922728698103,-0.375948097339969,
4.38063592879268));
#32057=CARTESIAN_POINT('Ctrl Pts',(14.5158869859602,-0.51156984651846,4.15657897149511));
#32058=CARTESIAN_POINT('Ctrl Pts',(14.53950110211,-0.52459032076832,3.89499677367918));
#32059=CARTESIAN_POINT('Ctrl Pts',(14.5631152182599,-0.411889072794842,
3.65857933001481));
#32060=CARTESIAN_POINT('Ctrl Pts',(14.5867293344098,-0.200475741228102,
3.50398572665543));
#32061=CARTESIAN_POINT('Ctrl Pts',(14.6103434505596,0.0589829973059192,
3.46826539682992));
#32062=CARTESIAN_POINT('Ctrl Pts',(14.6339575667095,0.304306049929579,3.5599789662306));
#32063=CARTESIAN_POINT('Ctrl Pts',(14.6575716828594,0.476700039321847,3.75714663952638));
#32064=CARTESIAN_POINT('Ctrl Pts',(14.6811857990092,0.53484954579562,4.0125158112076));
#32065=CARTESIAN_POINT('Ctrl Pts',(14.7047999151591,0.464818635404008,4.26488548168423));
#32066=CARTESIAN_POINT('Ctrl Pts',(14.728414031309,0.283390703164248,4.45377350235044));
#32067=CARTESIAN_POINT('Ctrl Pts',(14.7520281474588,0.0340462163765225,
4.5339115446661));
#32068=CARTESIAN_POINT('Ctrl Pts',(14.7756422636087,-0.223457683695575,
4.48609396779546));
#32069=CARTESIAN_POINT('Ctrl Pts',(14.7992563797586,-0.427408393186059,
4.32178058932398));
#32070=CARTESIAN_POINT('Ctrl Pts',(14.8228704959084,-0.528927708313459,
4.08035024907128));
#32071=CARTESIAN_POINT('Ctrl Pts',(14.8464846120583,-0.503685810960444,
3.81966341983811));
#32072=CARTESIAN_POINT('Ctrl Pts',(14.8700987282082,-0.357732113691821,
3.6021954912391));
#32073=CARTESIAN_POINT('Ctrl Pts',(14.893712844358,-0.126045401495737,3.48006421709321));
#32074=CARTESIAN_POINT('Ctrl Pts',(14.9173269605079,0.13584891809103,3.48253909847714));
#32075=CARTESIAN_POINT('Ctrl Pts',(14.9409410766578,0.365186207068703,3.60902724630258));
#32076=CARTESIAN_POINT('Ctrl Pts',(14.9645551928076,0.507003847624586,3.82921439524653));
#32077=CARTESIAN_POINT('Ctrl Pts',(14.9881693089575,0.52731498478211,4.0903322339271));
#32078=CARTESIAN_POINT('Ctrl Pts',(15.0117834251074,0.421250356706029,4.32979975898591));
#32079=CARTESIAN_POINT('Ctrl Pts',(15.0353975412572,0.214232462415332,4.49023183125449));
#32080=CARTESIAN_POINT('Ctrl Pts',(15.0590116574071,-0.0441324441701724,
4.53316925684615));
#32081=CARTESIAN_POINT('Ctrl Pts',(15.082625773557,-0.291909288096862,4.4483444097243));
#32082=CARTESIAN_POINT('Ctrl Pts',(15.1062398897068,-0.469745893811612,
4.25603780014884));
#32083=CARTESIAN_POINT('Ctrl Pts',(15.1219826338067,-0.513197418509596,
4.08697667736293));
#32084=CARTESIAN_POINT('Ctrl Pts',(15.1298540058567,-0.513578141027115,
4.0023094018511));
#32085=CARTESIAN_POINT('Ctrl Pts',(12.4701459941433,-0.231505035597357,
3.47990537377399));
#32086=CARTESIAN_POINT('Ctrl Pts',(12.4780173661933,-0.145763467775118,
3.44174000210903));
#32087=CARTESIAN_POINT('Ctrl Pts',(12.4937601102932,0.0448806955855158,
3.40867809900361));
#32088=CARTESIAN_POINT('Ctrl Pts',(12.517374226443,0.320205029627059,3.5008472864651));
#32089=CARTESIAN_POINT('Ctrl Pts',(12.5409883425929,0.518748616038451,3.71263883318769));
#32090=CARTESIAN_POINT('Ctrl Pts',(12.5646024587428,0.592991298599855,3.99330298545039));
#32091=CARTESIAN_POINT('Ctrl Pts',(12.5882165748926,0.525110091302815,4.27557062957281));
#32092=CARTESIAN_POINT('Ctrl Pts',(12.6118306910425,0.331387039860997,4.49179666512739));
#32093=CARTESIAN_POINT('Ctrl Pts',(12.6354448071924,0.0582427139750047,
4.5901598492798));
#32094=CARTESIAN_POINT('Ctrl Pts',(12.6590589233422,-0.22885891853004,4.54708728798072));
#32095=CARTESIAN_POINT('Ctrl Pts',(12.6826730394921,-0.461113368174311,
4.37290137073994));
#32096=CARTESIAN_POINT('Ctrl Pts',(12.706287155642,-0.582858578993347,4.10934708109011));
#32097=CARTESIAN_POINT('Ctrl Pts',(12.7299012717918,-0.564917771967644,
3.8195869850214));
#32098=CARTESIAN_POINT('Ctrl Pts',(12.7535153879417,-0.411590442520908,
3.57306413195747));
#32099=CARTESIAN_POINT('Ctrl Pts',(12.7771295040916,-0.159622619673808,
3.42885942795892));
#32100=CARTESIAN_POINT('Ctrl Pts',(12.8007436202414,0.130599885139872,3.42153253970604));
#32101=CARTESIAN_POINT('Ctrl Pts',(12.8243577363913,0.38952321367407,3.55283940440193));
#32102=CARTESIAN_POINT('Ctrl Pts',(12.8479718525412,0.555094594621529,3.79131141905102));
#32103=CARTESIAN_POINT('Ctrl Pts',(12.871585968691,0.587633690752404,4.07979710469805));
#32104=CARTESIAN_POINT('Ctrl Pts',(12.8952000848409,0.479342282651013,4.34915885879276));
#32105=CARTESIAN_POINT('Ctrl Pts',(12.9188142009908,0.256173159427565,4.53484226172604));
#32106=CARTESIAN_POINT('Ctrl Pts',(12.9424283171406,-0.0283896446575681,
4.59234699343691));
#32107=CARTESIAN_POINT('Ctrl Pts',(12.9660424332905,-0.306148672818738,
4.50789164463438));
#32108=CARTESIAN_POINT('Ctrl Pts',(12.9896565494404,-0.510537040311962,
4.30171652759364));
#32109=CARTESIAN_POINT('Ctrl Pts',(13.0132706655902,-0.59257165208389,4.02323294436244));
#32110=CARTESIAN_POINT('Ctrl Pts',(13.0368847817401,-0.532592342337314,
3.73918142428326));
#32111=CARTESIAN_POINT('Ctrl Pts',(13.06049889789,-0.344973570196446,3.51763689152052));
#32112=CARTESIAN_POINT('Ctrl Pts',(13.0841130140398,-0.0746794804792245,
3.41169403559782));
#32113=CARTESIAN_POINT('Ctrl Pts',(13.1077271301897,0.213512066603468,3.44674279944083));
#32114=CARTESIAN_POINT('Ctrl Pts',(13.1313412463396,0.450533960595157,3.6143835028084));
#32115=CARTESIAN_POINT('Ctrl Pts',(13.1549553624894,0.579582254610818,3.87443988413478));
#32116=CARTESIAN_POINT('Ctrl Pts',(13.1785694786393,0.569729626640933,4.1645876212947));
#32117=CARTESIAN_POINT('Ctrl Pts',(13.2021835947892,0.423337327565886,4.41529078926125));
#32118=CARTESIAN_POINT('Ctrl Pts',(13.225797710939,0.175489290945357,4.56646662860168));
#32119=CARTESIAN_POINT('Ctrl Pts',(13.2494118270889,-0.114415975890545,
4.58188479703192));
#32120=CARTESIAN_POINT('Ctrl Pts',(13.2730259432388,-0.376900657615966,
4.45785022315656));
#32121=CARTESIAN_POINT('Ctrl Pts',(13.2966400593886,-0.54905847301076,4.22408865605146));
#32122=CARTESIAN_POINT('Ctrl Pts',(13.3202541755385,-0.589630603166779,
3.93662268256671));
#32123=CARTESIAN_POINT('Ctrl Pts',(13.3438682916884,-0.488893654655812,
3.66434552439578));
#32124=CARTESIAN_POINT('Ctrl Pts',(13.3674824078382,-0.270989938452484,
3.47251029790774));
#32125=CARTESIAN_POINT('Ctrl Pts',(13.3910965239881,0.0118584029536041,
3.40709165056035));
#32126=CARTESIAN_POINT('Ctrl Pts',(13.414710640138,0.291864795541507,3.48376761659174));
#32127=CARTESIAN_POINT('Ctrl Pts',(13.4383247562878,0.501923758108325,3.68416226697515));
#32128=CARTESIAN_POINT('Ctrl Pts',(13.4619388724377,0.591693197983429,3.96024962873126));
#32129=CARTESIAN_POINT('Ctrl Pts',(13.4855529885876,0.539659243985316,4.2458634436777));
#32130=CARTESIAN_POINT('Ctrl Pts',(13.5091671047374,0.358292195415589,4.47255437280819));
#32131=CARTESIAN_POINT('Ctrl Pts',(13.5327812208873,0.0910579280213527,
4.58599435688436));
#32132=CARTESIAN_POINT('Ctrl Pts',(13.5563953370372,-0.197999005708236,
4.55899671402827));
#32133=CARTESIAN_POINT('Ctrl Pts',(13.580009453187,-0.439604099381795,4.39803161729011));
#32134=CARTESIAN_POINT('Ctrl Pts',(13.6036235693369,-0.575855010405679,
4.14167547263565));
#32135=CARTESIAN_POINT('Ctrl Pts',(13.6272376854868,-0.574098259464336,
3.85136581471317));
#32136=CARTESIAN_POINT('Ctrl Pts',(13.6508518016366,-0.434754864150196,
3.59667737398752));
#32137=CARTESIAN_POINT('Ctrl Pts',(13.6744659177865,-0.191219439166798,
3.43864800825098));
#32138=CARTESIAN_POINT('Ctrl Pts',(13.6980800339364,0.0981430555561168,
3.41515055509818));
#32139=CARTESIAN_POINT('Ctrl Pts',(13.7216941500862,0.363984883808003,3.53181634275091));
#32140=CARTESIAN_POINT('Ctrl Pts',(13.7453082662361,0.54259520083341,3.76068560304818));
#32141=CARTESIAN_POINT('Ctrl Pts',(13.768922382386,0.591168800790367,4.04690822452342));
#32142=CARTESIAN_POINT('Ctrl Pts',(13.7925364985358,0.498064682311931,4.32188896344761));
#32143=CARTESIAN_POINT('Ctrl Pts',(13.8161506146857,0.28559589552072,4.51972677150362));
#32144=CARTESIAN_POINT('Ctrl Pts',(13.8397647308356,0.00468206423833927,
4.59300844077494));
#32145=CARTESIAN_POINT('Ctrl Pts',(13.8633788469854,-0.277353856332193,
4.52417150908221));
#32146=CARTESIAN_POINT('Ctrl Pts',(13.8869929631353,-0.492919994478707,
4.32971322630275));
#32147=CARTESIAN_POINT('Ctrl Pts',(13.9106070792852,-0.590354424565592,
4.05623687359455));
#32148=CARTESIAN_POINT('Ctrl Pts',(13.934221195435,-0.546306307148498,3.76928296264551));
#32149=CARTESIAN_POINT('Ctrl Pts',(13.9578353115849,-0.371332080200278,
3.53762199579782));
#32150=CARTESIAN_POINT('Ctrl Pts',(13.9814494277348,-0.107365535263851,
3.41677313642685));
#32151=CARTESIAN_POINT('Ctrl Pts',(14.0050635438846,0.182331907606365,3.43569865495067));
#32152=CARTESIAN_POINT('Ctrl Pts',(14.0286776600345,0.428332239544634,3.58986291910809));
#32153=CARTESIAN_POINT('Ctrl Pts',(14.0522917761844,0.571679768510432,3.8423193898042));
#32154=CARTESIAN_POINT('Ctrl Pts',(14.0759058923342,0.578020261296468,4.1325651164018));
#32155=CARTESIAN_POINT('Ctrl Pts',(14.0995200084841,0.445834174668256,4.39104069002309));
#32156=CARTESIAN_POINT('Ctrl Pts',(14.123134124634,0.206800824478305,4.55580064011384));
#32157=CARTESIAN_POINT('Ctrl Pts',(14.1467482407838,-0.0817937829083601,
4.58735909768505));
#32158=CARTESIAN_POINT('Ctrl Pts',(14.1703623569337,-0.350785940826847,
4.4781528586907));
#32159=CARTESIAN_POINT('Ctrl Pts',(14.1939764730836,-0.535709806086595,
4.25435395852733));
#32160=CARTESIAN_POINT('Ctrl Pts',(14.2175905892334,-0.59224708706053,3.96959736155895));
#32161=CARTESIAN_POINT('Ctrl Pts',(14.2412047053833,-0.506848230788112,
3.69212696853602));
#32162=CARTESIAN_POINT('Ctrl Pts',(14.2648188215332,-0.29997966766535,3.48844049071174));
#32163=CARTESIAN_POINT('Ctrl Pts',(14.288432937683,-0.0212188889266537,
3.40735281042717));
#32164=CARTESIAN_POINT('Ctrl Pts',(14.3120470538329,0.262627144255178,3.46829715474127));
#32165=CARTESIAN_POINT('Ctrl Pts',(14.3356611699828,0.483532754079872,3.65666778728498));
#32166=CARTESIAN_POINT('Ctrl Pts',(14.3592752861326,0.588556373354274,3.9273203746575));
#32167=CARTESIAN_POINT('Ctrl Pts',(14.3828894022825,0.55252836061433,4.21539114019081));
#32168=CARTESIAN_POINT('Ctrl Pts',(14.4065035184324,0.384083079916361,4.45184191956682));
#32169=CARTESIAN_POINT('Ctrl Pts',(14.4301176345822,0.123589615384189,4.58000563749418));
#32170=CARTESIAN_POINT('Ctrl Pts',(14.4537317507321,-0.166522960823891,
4.56916696678068));
#32171=CARTESIAN_POINT('Ctrl Pts',(14.477345866882,-0.416727150247931,4.42192347031433));
#32172=CARTESIAN_POINT('Ctrl Pts',(14.5009599830318,-0.567059777136274,
4.17356307703535));
#32173=CARTESIAN_POINT('Ctrl Pts',(14.5245740991817,-0.58149258093928,3.88360708411314));
#32174=CARTESIAN_POINT('Ctrl Pts',(14.5481882153316,-0.456566639753037,
3.62154546373458));
#32175=CARTESIAN_POINT('Ctrl Pts',(14.5718023314814,-0.222221325036472,
3.45018310752014));
#32176=CARTESIAN_POINT('Ctrl Pts',(14.5954164476313,0.0653808771856868,
3.41058819705396));
#32177=CARTESIAN_POINT('Ctrl Pts',(14.6190305637812,0.337314097045906,3.51224992824993));
#32178=CARTESIAN_POINT('Ctrl Pts',(14.642644679931,0.528407645404381,3.73080435955289));
#32179=CARTESIAN_POINT('Ctrl Pts',(14.6662587960809,0.592864623089856,4.0138734000105));
#32180=CARTESIAN_POINT('Ctrl Pts',(14.6898729122308,0.515237466779568,4.29361758366474));
#32181=CARTESIAN_POINT('Ctrl Pts',(14.7134870283806,0.314130064687094,4.5029942692369));
#32182=CARTESIAN_POINT('Ctrl Pts',(14.7371011445305,0.0377392060970651,
4.59182487707066));
#32183=CARTESIAN_POINT('Ctrl Pts',(14.7607152606804,-0.24769611652869,4.53882053236973));
#32184=CARTESIAN_POINT('Ctrl Pts',(14.7843293768302,-0.47376933929102,4.35668409799883));
#32185=CARTESIAN_POINT('Ctrl Pts',(14.8079434929801,-0.586300444482135,
4.08906583263515));
#32186=CARTESIAN_POINT('Ctrl Pts',(14.83155760913,-0.558320561021625,3.80010232883727));
#32187=CARTESIAN_POINT('Ctrl Pts',(14.8551717252798,-0.396535280656446,
3.55904567554761));
#32188=CARTESIAN_POINT('Ctrl Pts',(14.8787858414297,-0.139717533720287,
3.42366683418339));
#32189=CARTESIAN_POINT('Ctrl Pts',(14.9023999575795,0.150584436790342,3.42641016570609));
#32190=CARTESIAN_POINT('Ctrl Pts',(14.9260140737294,0.404797918804129,3.56661847040663));
#32191=CARTESIAN_POINT('Ctrl Pts',(14.9496281898793,0.561998504794314,3.8106892976029));
#32192=CARTESIAN_POINT('Ctrl Pts',(14.9732423060292,0.584512788988964,4.10013056240029));
#32193=CARTESIAN_POINT('Ctrl Pts',(14.996856422179,0.466943341203511,4.36557310620026));
#32194=CARTESIAN_POINT('Ctrl Pts',(15.0204705383289,0.237470236409271,4.54340722946861));
#32195=CARTESIAN_POINT('Ctrl Pts',(15.0440846544788,-0.0489194860211801,
4.59100207336435));
#32196=CARTESIAN_POINT('Ctrl Pts',(15.0676987706286,-0.323572659684198,
4.49697628347096));
#32197=CARTESIAN_POINT('Ctrl Pts',(15.0913128867785,-0.520699184418956,
4.28381019498893));
#32198=CARTESIAN_POINT('Ctrl Pts',(15.1070556308784,-0.568863891700195,
4.09641102894772));
#32199=CARTESIAN_POINT('Ctrl Pts',(15.1149270029284,-0.569285911151507,
4.00255990244131));
#32200=CARTESIAN_POINT('Ctrl Pts',(12.455218991215,-0.25415908175074,3.42901124252432));
#32201=CARTESIAN_POINT('Ctrl Pts',(12.4630903632649,-0.16002722803387,3.38711117848463));
#32202=CARTESIAN_POINT('Ctrl Pts',(12.4788331073648,0.0492725194893315,
3.35081398558546));
#32203=CARTESIAN_POINT('Ctrl Pts',(12.5024472235147,0.351538860016532,3.45200243701797));
#32204=CARTESIAN_POINT('Ctrl Pts',(12.5260613396645,0.569511032758309,3.68451895614546));
#32205=CARTESIAN_POINT('Ctrl Pts',(12.5496754558144,0.651018771792273,3.99264764559437));
#32206=CARTESIAN_POINT('Ctrl Pts',(12.5732895719643,0.576495013506714,4.3025367374363));
#32207=CARTESIAN_POINT('Ctrl Pts',(12.5969036881141,0.363815091701307,4.53992168461618));
#32208=CARTESIAN_POINT('Ctrl Pts',(12.620517804264,0.0639420851661475,4.64791024952038));
#32209=CARTESIAN_POINT('Ctrl Pts',(12.6441319204139,-0.251254027515963,
4.60062280024232));
#32210=CARTESIAN_POINT('Ctrl Pts',(12.6677460365637,-0.506235857616531,
4.40939182910775));
#32211=CARTESIAN_POINT('Ctrl Pts',(12.6913601527136,-0.639894509617229,
4.12004729681268));
#32212=CARTESIAN_POINT('Ctrl Pts',(12.7149742688635,-0.620198095551099,
3.8019325752266));
#32213=CARTESIAN_POINT('Ctrl Pts',(12.7385883850133,-0.451866840211785,
3.53128609963859));
#32214=CARTESIAN_POINT('Ctrl Pts',(12.7622025011632,-0.17524257447904,3.37297016902465));
#32215=CARTESIAN_POINT('Ctrl Pts',(12.7858166173131,0.143379805101228,3.36492630429559));
#32216=CARTESIAN_POINT('Ctrl Pts',(12.809430733463,0.42764021116234,3.50908227080648));
#32217=CARTESIAN_POINT('Ctrl Pts',(12.8330448496128,0.609413666055986,3.77089008898231));
#32218=CARTESIAN_POINT('Ctrl Pts',(12.8566589657627,0.645136892431096,4.08760569204938));
#32219=CARTESIAN_POINT('Ctrl Pts',(12.8802730819125,0.526248572038732,4.38332598125533));
#32220=CARTESIAN_POINT('Ctrl Pts',(12.9038871980624,0.281241117720374,4.58717953054897));
#32221=CARTESIAN_POINT('Ctrl Pts',(12.9275013142123,-0.0311677281609838,
4.65031141781114));
#32222=CARTESIAN_POINT('Ctrl Pts',(12.9511154303622,-0.336107011072318,
4.55759164674784));
#32223=CARTESIAN_POINT('Ctrl Pts',(12.974729546512,-0.56049590900091,4.33124115596169));
#32224=CARTESIAN_POINT('Ctrl Pts',(12.9983436626619,-0.650558060547343,
4.02550641626558));
#32225=CARTESIAN_POINT('Ctrl Pts',(13.0219577788117,-0.584709444123524,
3.71365888635357));
#32226=CARTESIAN_POINT('Ctrl Pts',(13.0455718949616,-0.378731139057797,
3.47043499764384));
#32227=CARTESIAN_POINT('Ctrl Pts',(13.0691860111115,-0.0819872800401352,
3.35412504823007));
#32228=CARTESIAN_POINT('Ctrl Pts',(13.0928001272613,0.234405401379786,3.39260352716186));
#32229=CARTESIAN_POINT('Ctrl Pts',(13.1164142434112,0.494621196584012,3.57664879910166));
#32230=CARTESIAN_POINT('Ctrl Pts',(13.1400283595611,0.636297578801308,3.86215313342763));
#32231=CARTESIAN_POINT('Ctrl Pts',(13.1636424757109,0.625480816776257,4.18069342892634));
#32232=CARTESIAN_POINT('Ctrl Pts',(13.1872565918608,0.464763222827219,4.45592928631477));
#32233=CARTESIAN_POINT('Ctrl Pts',(13.2108707080107,0.192661887153653,4.62189851635989));
#32234=CARTESIAN_POINT('Ctrl Pts',(13.2344848241605,-0.125612210960856,
4.63882543771344));
#32235=CARTESIAN_POINT('Ctrl Pts',(13.2580989403104,-0.413782468289504,
4.50265339583901));
#32236=CARTESIAN_POINT('Ctrl Pts',(13.2817130564603,-0.602786876612853,
4.24601696851145));
#32237=CARTESIAN_POINT('Ctrl Pts',(13.3053271726101,-0.647329213752593,
3.9304208620728));
#32238=CARTESIAN_POINT('Ctrl Pts',(13.32894128876,-0.536734598538914,3.6314998804023));
#32239=CARTESIAN_POINT('Ctrl Pts',(13.3525554049099,-0.297507800394296,
3.42089251764738));
#32240=CARTESIAN_POINT('Ctrl Pts',(13.3761695210598,0.0130188131672444,
3.34907229440132));
#32241=CARTESIAN_POINT('Ctrl Pts',(13.3997836372096,0.320425377524893,3.43325142712992));
#32242=CARTESIAN_POINT('Ctrl Pts',(13.4233977533595,0.551039769569266,3.65325580067535));
#32243=CARTESIAN_POINT('Ctrl Pts',(13.4470118695093,0.649593644862141,3.95635983539258));
#32244=CARTESIAN_POINT('Ctrl Pts',(13.4706259856592,0.592467881122722,4.26992253935193));
#32245=CARTESIAN_POINT('Ctrl Pts',(13.4942401018091,0.393353065302923,4.5187964277335));
#32246=CARTESIAN_POINT('Ctrl Pts',(13.5178542179589,0.0999684491195412,
4.64333714069132));
#32247=CARTESIAN_POINT('Ctrl Pts',(13.5414683341088,-0.217374301809525,
4.61369762939502));
#32248=CARTESIAN_POINT('Ctrl Pts',(13.5650824502587,-0.482621788093898,
4.43698120905743));
#32249=CARTESIAN_POINT('Ctrl Pts',(13.5886965664085,-0.632205603168059,
4.15553919999523));
#32250=CARTESIAN_POINT('Ctrl Pts',(13.6123106825584,-0.630276944445953,
3.83682113889318));
#32251=CARTESIAN_POINT('Ctrl Pts',(13.6359247987083,-0.477298028416376,
3.55721002779864));
#32252=CARTESIAN_POINT('Ctrl Pts',(13.6595389148582,-0.209931317243796,
3.38371661595291));
#32253=CARTESIAN_POINT('Ctrl Pts',(13.683153031008,0.107746895509167,3.35791980725116));
#32254=CARTESIAN_POINT('Ctrl Pts',(13.7067671471579,0.399602814690774,3.48600198647908));
#32255=CARTESIAN_POINT('Ctrl Pts',(13.7303812633077,0.59569113756138,3.73726736776131));
#32256=CARTESIAN_POINT('Ctrl Pts',(13.7539953794576,0.649017932507905,4.05149845333026));
#32257=CARTESIAN_POINT('Ctrl Pts',(13.7776094956075,0.546803061895555,4.35338757606046));
#32258=CARTESIAN_POINT('Ctrl Pts',(13.8012236117573,0.313543031018869,4.57058490613733));
#32259=CARTESIAN_POINT('Ctrl Pts',(13.8248377279072,0.00514023007941788,
4.65103759142385));
#32260=CARTESIAN_POINT('Ctrl Pts',(13.8484518440571,-0.304494462781446,
4.57546458583277));
#32261=CARTESIAN_POINT('Ctrl Pts',(13.8720659602069,-0.541154937947787,
4.36197748624323));
#32262=CARTESIAN_POINT('Ctrl Pts',(13.8956800763568,-0.648123865072376,
4.06173996222779));
#32263=CARTESIAN_POINT('Ctrl Pts',(13.9192941925067,-0.599765396122921,
3.74670602647169));
#32264=CARTESIAN_POINT('Ctrl Pts',(13.9429083086565,-0.407668974822819,
3.49237575473668));
#32265=CARTESIAN_POINT('Ctrl Pts',(13.9665224248064,-0.117871845784803,
3.35970116712309));
#32266=CARTESIAN_POINT('Ctrl Pts',(13.9901365409563,0.200174091641329,3.38047865214521));
#32267=CARTESIAN_POINT('Ctrl Pts',(14.0137506571061,0.470246914526057,3.54972874087838));
#32268=CARTESIAN_POINT('Ctrl Pts',(14.037364773256,0.627621790796785,3.82688947135059));
#32269=CARTESIAN_POINT('Ctrl Pts',(14.0609788894059,0.634582735815489,4.14553734509456));
#32270=CARTESIAN_POINT('Ctrl Pts',(14.0845930055557,0.489461510650943,4.42930618095194));
#32271=CARTESIAN_POINT('Ctrl Pts',(14.1082071217056,0.227037427151766,4.61018880199865));
#32272=CARTESIAN_POINT('Ctrl Pts',(14.1318212378555,-0.0897977562486571,
4.64483542891575));
#32273=CARTESIAN_POINT('Ctrl Pts',(14.1554353540053,-0.385112282251534,
4.52494275637564));
#32274=CARTESIAN_POINT('Ctrl Pts',(14.1790494701552,-0.588131968915973,
4.27924389796604));
#32275=CARTESIAN_POINT('Ctrl Pts',(14.2026635863051,-0.65020173504413,3.96662229549764));
#32276=CARTESIAN_POINT('Ctrl Pts',(14.2262777024549,-0.556446129094758,
3.66199989226673));
#32277=CARTESIAN_POINT('Ctrl Pts',(14.2498918186048,-0.329334334698108,
3.43838156778717));
#32278=CARTESIAN_POINT('Ctrl Pts',(14.2735059347547,-0.0232952743833569,
3.34935901020328));
#32279=CARTESIAN_POINT('Ctrl Pts',(14.2971200509045,0.28832666060365,3.41626709515619));
#32280=CARTESIAN_POINT('Ctrl Pts',(14.3207341670544,0.530849104237583,3.62307083431711));
#32281=CARTESIAN_POINT('Ctrl Pts',(14.3443482832043,0.646149864620809,3.92020827196535));
#32282=CARTESIAN_POINT('Ctrl Pts',(14.3679623993541,0.606596311879891,4.2364683526943));
#32283=CARTESIAN_POINT('Ctrl Pts',(14.391576515504,0.42166773027486,4.49605714656388));
#32284=CARTESIAN_POINT('Ctrl Pts',(14.4151906316539,0.135683541737747,4.63676239203782));
#32285=CARTESIAN_POINT('Ctrl Pts',(14.4388047478037,-0.182818152115814,
4.62486309754155));
#32286=CARTESIAN_POINT('Ctrl Pts',(14.4624188639536,-0.457506203155893,
4.46321101183598));
#32287=CARTESIAN_POINT('Ctrl Pts',(14.4860329801035,-0.622549707754089,
4.19054718257559));
#32288=CARTESIAN_POINT('Ctrl Pts',(14.5096470962533,-0.63839484111024,3.87221739454711));
#32289=CARTESIAN_POINT('Ctrl Pts',(14.5332612124032,-0.501244206711231,
3.58451159745434));
#32290=CARTESIAN_POINT('Ctrl Pts',(14.5568753285531,-0.243966908844842,
3.39638048838484));
#32291=CARTESIAN_POINT('Ctrl Pts',(14.5804894447029,0.0717787570654544,
3.35291099727801));
#32292=CARTESIAN_POINT('Ctrl Pts',(14.6041035608528,0.370322144162233,3.46452089026927));
#32293=CARTESIAN_POINT('Ctrl Pts',(14.6277176770027,0.580115251486915,3.70446207957941));
#32294=CARTESIAN_POINT('Ctrl Pts',(14.6513317931525,0.650879700384091,4.0152309888134));
#32295=CARTESIAN_POINT('Ctrl Pts',(14.6749459093024,0.565656298155129,4.32234968564526));
#32296=CARTESIAN_POINT('Ctrl Pts',(14.6985600254523,0.344869426209941,4.55221503612336));
#32297=CARTESIAN_POINT('Ctrl Pts',(14.7221741416021,0.041432195817608,4.64973820947522));
#32298=CARTESIAN_POINT('Ctrl Pts',(14.745788257752,-0.271934549361806,4.59154709694401));
#32299=CARTESIAN_POINT('Ctrl Pts',(14.7694023739019,-0.520130285395982,
4.39158760667368));
#32300=CARTESIAN_POINT('Ctrl Pts',(14.7930164900517,-0.64367318065081,4.09778141619902));
#32301=CARTESIAN_POINT('Ctrl Pts',(14.8166306062016,-0.612955311082805,
3.78054123783642));
#32302=CARTESIAN_POINT('Ctrl Pts',(14.8402447223515,-0.435338447621071,
3.51589585985611));
#32303=CARTESIAN_POINT('Ctrl Pts',(14.8638588385013,-0.153389665944836,
3.36726945127358));
#32304=CARTESIAN_POINT('Ctrl Pts',(14.8874729546512,0.165319955489652,3.37028123293502));
#32305=CARTESIAN_POINT('Ctrl Pts',(14.9110870708011,0.444409630539555,3.52420969451069));
#32306=CARTESIAN_POINT('Ctrl Pts',(14.9347011869509,0.616993161964042,3.79216419995926));
#32307=CARTESIAN_POINT('Ctrl Pts',(14.9583153031008,0.641710593195818,4.10992889087348));
#32308=CARTESIAN_POINT('Ctrl Pts',(14.9819294192507,0.512636325700993,4.40134645341462));
#32309=CARTESIAN_POINT('Ctrl Pts',(15.0055435354005,0.260708010403211,4.59658262768273));
#32310=CARTESIAN_POINT('Ctrl Pts',(15.0291576515504,-0.0537065278721878,
4.64883488988255));
#32311=CARTESIAN_POINT('Ctrl Pts',(15.0527717677003,-0.355236031271534,
4.54560815721762));
#32312=CARTESIAN_POINT('Ctrl Pts',(15.0763858838501,-0.571652475026301,
4.31158258982903));
#32313=CARTESIAN_POINT('Ctrl Pts',(15.09212862795,-0.624530364890795,4.10584538053252));
#32314=CARTESIAN_POINT('Ctrl Pts',(15.1,-0.624993681275899,4.00281040303152));
#32315=CARTESIAN_POINT('Ctrl Pts',(15.1,-0.624993681275899,4.00281040303152));
#32316=CARTESIAN_POINT('Ctrl Pts',(15.1,-0.617358358083874,4.02914127082806));
#32317=CARTESIAN_POINT('Ctrl Pts',(15.1,-0.607931963506944,4.05484759228836));
#32318=CARTESIAN_POINT('Ctrl Pts',(15.1,-0.596773861259576,4.07974656001827));
#32319=CARTESIAN_POINT('Ctrl Pts',(15.1,-0.585871522029423,4.10407480030985));
#32320=CARTESIAN_POINT('Ctrl Pts',(15.1,-0.573314772633929,4.12763281365198));
#32321=CARTESIAN_POINT('Ctrl Pts',(15.1,-0.559143639302279,4.1502040881484));
#32322=CARTESIAN_POINT('Ctrl Pts',(15.1,-0.549626121151564,4.16536325076984));
#32323=CARTESIAN_POINT('Ctrl Pts',(15.1,-0.539380106047495,4.18007635520315));
#32324=CARTESIAN_POINT('Ctrl Pts',(15.1,-0.528417753985571,4.19426420824267));
#32325=CARTESIAN_POINT('Ctrl Pts',(15.1,-0.523814643226911,4.2002217124899));
#32326=CARTESIAN_POINT('Ctrl Pts',(15.1,-0.519084627089791,4.20608691507751));
#32327=CARTESIAN_POINT('Ctrl Pts',(15.1,-0.514239086396905,4.21184190560023));
#32328=CARTESIAN_POINT('Ctrl Pts',(15.1,-0.50085552272952,4.2277374035328));
#32329=CARTESIAN_POINT('Ctrl Pts',(15.1,-0.486572803760524,4.24281789068328));
#32330=CARTESIAN_POINT('Ctrl Pts',(15.1,-0.4714177983537,4.25697008589974));
#32331=CARTESIAN_POINT('Ctrl Pts',(15.1,-0.457151696655403,4.27029219637033));
#32332=CARTESIAN_POINT('Ctrl Pts',(15.1,-0.442112042545397,4.28279146400573));
#32333=CARTESIAN_POINT('Ctrl Pts',(15.1,-0.426369607892924,4.29437520287289));
#32334=CARTESIAN_POINT('Ctrl Pts',(15.1,-0.419074661497203,4.29974303548351));
#32335=CARTESIAN_POINT('Ctrl Pts',(15.1,-0.411628924918527,4.30491398987477));
#32336=CARTESIAN_POINT('Ctrl Pts',(15.1,-0.404040271526401,4.30987739070861));
#32337=CARTESIAN_POINT('Ctrl Pts',(15.1,-0.398073367501634,4.31378007737535));
#32338=CARTESIAN_POINT('Ctrl Pts',(15.1,-0.392026704362881,4.31754881952869));
#32339=CARTESIAN_POINT('Ctrl Pts',(15.1,-0.385904261325812,4.32117966642505));
#32340=CARTESIAN_POINT('Ctrl Pts',(15.1,-0.366868686798561,4.33246850264191));
#32341=CARTESIAN_POINT('Ctrl Pts',(15.1,-0.347097727375919,4.34242824684389));
#32342=CARTESIAN_POINT('Ctrl Pts',(15.1,-0.326713262272485,4.3509180109496));
#32343=CARTESIAN_POINT('Ctrl Pts',(15.1,-0.308010762698638,4.35870726657947));
#32344=CARTESIAN_POINT('Ctrl Pts',(15.1,-0.288791261952878,4.36525839133365));
#32345=CARTESIAN_POINT('Ctrl Pts',(15.1,-0.269173508333929,4.37043259773196));
#32346=CARTESIAN_POINT('Ctrl Pts',(12.5,-0.186196943290592,3.58169363627332));
#32347=CARTESIAN_POINT('Ctrl Pts',(12.5,-0.170588484282379,3.56594316788148));
#32348=CARTESIAN_POINT('Ctrl Pts',(12.5,-0.153797667832464,3.55144458439849));
#32349=CARTESIAN_POINT('Ctrl Pts',(12.5,-0.136060690067392,3.53823162417247));
#32350=CARTESIAN_POINT('Ctrl Pts',(12.5,-0.117990710310259,3.5247705978929));
#32351=CARTESIAN_POINT('Ctrl Pts',(12.5,-0.0989385549429972,3.51264262455394));
#32352=CARTESIAN_POINT('Ctrl Pts',(12.5,-0.0790990435859813,3.5018744512649));
#32353=CARTESIAN_POINT('Ctrl Pts',(12.5,-0.0668145727052721,3.49520688224936));
#32354=CARTESIAN_POINT('Ctrl Pts',(12.5,-0.054227138249592,3.4890605701039));
#32355=CARTESIAN_POINT('Ctrl Pts',(12.5,-0.0413735013057162,3.4834433907237));
#32356=CARTESIAN_POINT('Ctrl Pts',(12.5,-0.0353493612034326,3.48081077586818));
#32357=CARTESIAN_POINT('Ctrl Pts',(12.5,-0.0292710672153644,3.47829647656688));
#32358=CARTESIAN_POINT('Ctrl Pts',(12.5,-0.0231507758853709,3.47590397706369));
#32359=CARTESIAN_POINT('Ctrl Pts',(12.5,-0.00211397253512804,3.467680423829));
#32360=CARTESIAN_POINT('Ctrl Pts',(12.5,0.0194422610390746,3.46088402724794));
#32361=CARTESIAN_POINT('Ctrl Pts',(12.5,0.0413436963816045,3.45552737346533));
#32362=CARTESIAN_POINT('Ctrl Pts',(12.5,0.0650920698750741,3.44971899548849));
#32363=CARTESIAN_POINT('Ctrl Pts',(12.5,0.089246474293393,3.44560199012534));
#32364=CARTESIAN_POINT('Ctrl Pts',(12.5,0.113633446029948,3.44311473184586));
#32365=CARTESIAN_POINT('Ctrl Pts',(12.5,0.123118497624279,3.44214733936417));
#32366=CARTESIAN_POINT('Ctrl Pts',(12.5,0.132642564327611,3.44142688205345));
#32367=CARTESIAN_POINT('Ctrl Pts',(12.5,0.142169452875131,3.44095138714122));
#32368=CARTESIAN_POINT('Ctrl Pts',(12.5,0.170359862108328,3.43954438042575));
#32369=CARTESIAN_POINT('Ctrl Pts',(12.5,0.19861482332424,3.44027367679077));
#32370=CARTESIAN_POINT('Ctrl Pts',(12.5,0.226679319731597,3.44302987267532));
#32371=CARTESIAN_POINT('Ctrl Pts',(12.5,0.254743816138955,3.44578606855986));
#32372=CARTESIAN_POINT('Ctrl Pts',(12.5,0.282619254593541,3.45056842907764));
#32373=CARTESIAN_POINT('Ctrl Pts',(12.5,0.310093463203745,3.45730861053194));
#32374=CARTESIAN_POINT('Ctrl Pts',(15.0699957084852,-1.05870731373636E-5,
4.45788944868556));
#32375=CARTESIAN_POINT('Ctrl Pts',(15.0634386537186,0.0628625045491076,
4.45782850550181));
#32376=CARTESIAN_POINT('Ctrl Pts',(15.0568815989521,0.125761012144406,4.44477074790967));
#32377=CARTESIAN_POINT('Ctrl Pts',(15.0503245441856,0.183365120595825,4.41959809737683));
#32378=CARTESIAN_POINT('Ctrl Pts',(15.0424531721356,0.252515583017112,4.38937975928409));
#32379=CARTESIAN_POINT('Ctrl Pts',(15.0345818000857,0.314036477612831,4.34170308552782));
#32380=CARTESIAN_POINT('Ctrl Pts',(15.0267104280357,0.360556892971808,4.28228266426341));
#32381=CARTESIAN_POINT('Ctrl Pts',(15.0188390559858,0.407077308330786,4.222862242999));
#32382=CARTESIAN_POINT('Ctrl Pts',(15.0109676839358,0.438597244453022,4.15169807422645));
#32383=CARTESIAN_POINT('Ctrl Pts',(15.0030963118859,0.45133921416074,4.07731692107955));
#32384=CARTESIAN_POINT('Ctrl Pts',(14.9952249398359,0.464081183868457,4.00293576793266));
#32385=CARTESIAN_POINT('Ctrl Pts',(14.9873535677859,0.458045187161657,3.92533763041141));
#32386=CARTESIAN_POINT('Ctrl Pts',(14.979482195736,0.433954739621328,3.85382131653551));
#32387=CARTESIAN_POINT('Ctrl Pts',(14.971610823686,0.409864292080999,3.78230500265962));
#32388=CARTESIAN_POINT('Ctrl Pts',(14.9637394516361,0.367719393707138,3.71687051242907));
#32389=CARTESIAN_POINT('Ctrl Pts',(14.9558680795861,0.312570095196614,3.66535860215541));
#32390=CARTESIAN_POINT('Ctrl Pts',(14.9479967075362,0.257420796686091,3.61384669188175));
#32391=CARTESIAN_POINT('Ctrl Pts',(14.9401253354862,0.189267098038905,3.57625736156498));
#32392=CARTESIAN_POINT('Ctrl Pts',(14.9322539634362,0.116275803938161,3.55709495786573));
#32393=CARTESIAN_POINT('Ctrl Pts',(14.9243825913863,0.0432845098374172,
3.53793255416647));
#32394=CARTESIAN_POINT('Ctrl Pts',(14.9165112193363,-0.0345443797168851,
3.53719707708475));
#32395=CARTESIAN_POINT('Ctrl Pts',(14.9086398472864,-0.107884770736704,
3.55497662303181));
#32396=CARTESIAN_POINT('Ctrl Pts',(14.9007684752364,-0.181225161756525,
3.57275616897888));
#32397=CARTESIAN_POINT('Ctrl Pts',(14.8928971031865,-0.250077054241862,
3.60905073795473));
#32398=CARTESIAN_POINT('Ctrl Pts',(14.8850257311365,-0.306190019513209,
3.65951122309406));
#32399=CARTESIAN_POINT('Ctrl Pts',(14.8771543590866,-0.362302984784554,
3.70997170823338));
#32400=CARTESIAN_POINT('Ctrl Pts',(14.8692829870366,-0.405677022841909,
3.77459810953617));
#32401=CARTESIAN_POINT('Ctrl Pts',(14.8614116149867,-0.431114693744839,
3.84564633596564));
#32402=CARTESIAN_POINT('Ctrl Pts',(14.8535402429367,-0.45655236464777,3.91669456239511));
#32403=CARTESIAN_POINT('Ctrl Pts',(14.8456688708867,-0.464053668396277,
3.99416461395126));
#32404=CARTESIAN_POINT('Ctrl Pts',(14.8377974988368,-0.452719732759917,
4.06877337558629));
#32405=CARTESIAN_POINT('Ctrl Pts',(14.8299261267868,-0.441385797123556,
4.14338213722132));
#32406=CARTESIAN_POINT('Ctrl Pts',(14.8220547547369,-0.411216622102327,
4.21512960893523));
#32407=CARTESIAN_POINT('Ctrl Pts',(14.8141833826869,-0.365827335221939,
4.27541839855419));
#32408=CARTESIAN_POINT('Ctrl Pts',(14.806312010637,-0.32043804834155,4.33570718817315));
#32409=CARTESIAN_POINT('Ctrl Pts',(14.798440638587,-0.259828649602004,4.38453729569717));
#32410=CARTESIAN_POINT('Ctrl Pts',(14.7905692665371,-0.191261870645823,
4.41605748429924));
#32411=CARTESIAN_POINT('Ctrl Pts',(14.7837114138531,-0.131523763221734,
4.44351912740692));
#32412=CARTESIAN_POINT('Ctrl Pts',(14.7768535611691,-0.065745536276614,
4.45784152413683));
#32413=CARTESIAN_POINT('Ctrl Pts',(14.7699957084852,8.6346448269735E-6,
4.45789857801605));
#32414=CARTESIAN_POINT('Ctrl Pts',(12.5,0.310062960217722,4.54266560670548));
#32415=CARTESIAN_POINT('Ctrl Pts',(12.50787137205,0.220600394030941,4.59378185169648));
#32416=CARTESIAN_POINT('Ctrl Pts',(12.5236141161499,0.0159878432799406,
4.65085692712531));
#32417=CARTESIAN_POINT('Ctrl Pts',(12.5472282322997,-0.294892507759568,
4.580447501361));
#32418=CARTESIAN_POINT('Ctrl Pts',(12.5708423484496,-0.535054221536356,
4.37092866956447));
#32419=CARTESIAN_POINT('Ctrl Pts',(12.5944564645995,-0.647009713430093,
4.07251155115386));
#32420=CARTESIAN_POINT('Ctrl Pts',(12.6180705807493,-0.603894380709874,
3.75671714932517));
#32421=CARTESIAN_POINT('Ctrl Pts',(12.6416846968992,-0.416056506175611,
3.49922677321964));
#32422=CARTESIAN_POINT('Ctrl Pts',(12.6652988130491,-0.128505496873939,
3.36175035317655));
#32423=CARTESIAN_POINT('Ctrl Pts',(12.6889129291989,0.189841674427298,3.37723482234205));
#32424=CARTESIAN_POINT('Ctrl Pts',(12.7125270453488,0.462692468193658,3.54196933898577));
#32425=CARTESIAN_POINT('Ctrl Pts',(12.7361411614987,0.624655556881011,3.81647407445394));
#32426=CARTESIAN_POINT('Ctrl Pts',(12.7597552776485,0.636915702199809,4.13496208375113));
#32427=CARTESIAN_POINT('Ctrl Pts',(12.7833693937984,0.496534514683115,4.42110548633398));
#32428=CARTESIAN_POINT('Ctrl Pts',(12.8069835099483,0.237155397994168,4.60632802944461));
#32429=CARTESIAN_POINT('Ctrl Pts',(12.8305976260981,-0.0790596718614395,
4.64623983861064));
#32430=CARTESIAN_POINT('Ctrl Pts',(12.854211742248,-0.376327535803878,4.5312757721487));
#32431=CARTESIAN_POINT('Ctrl Pts',(12.8778258583979,-0.583405888470749,
4.28898776831928));
#32432=CARTESIAN_POINT('Ctrl Pts',(12.9014399745477,-0.650666957548692,
3.97744183415536));
#32433=CARTESIAN_POINT('Ctrl Pts',(12.9250540906976,-0.561991161265395,
3.67130212143154));
#32434=CARTESIAN_POINT('Ctrl Pts',(12.9486682068475,-0.338630270727757,
3.44393714350224));
#32435=CARTESIAN_POINT('Ctrl Pts',(12.9722823229973,-0.0341142786054444,
3.34983650006563));
#32436=CARTESIAN_POINT('Ctrl Pts',(12.9958964391472,0.278577437919422,3.41155206540036));
#32437=CARTESIAN_POINT('Ctrl Pts',(13.0195105552971,0.524506132150044,3.61429327464512));
#32438=CARTESIAN_POINT('Ctrl Pts',(13.0431246714469,0.644733280558021,3.90947178565704));
#32439=CARTESIAN_POINT('Ctrl Pts',(13.0667387875968,0.61044561006836,4.22634601343335));
#32440=CARTESIAN_POINT('Ctrl Pts',(13.0903529037467,0.429860399609997,4.4889748434194));
#32441=CARTESIAN_POINT('Ctrl Pts',(13.1139670198965,0.146256151980267,4.63441744826062));
#32442=CARTESIAN_POINT('Ctrl Pts',(13.1375811360464,-0.172399400609521,
4.62781749523177));
#32443=CARTESIAN_POINT('Ctrl Pts',(13.1611952521963,-0.449738236712957,
4.47075670902068));
#32444=CARTESIAN_POINT('Ctrl Pts',(13.1848093683461,-0.619294173608025,
4.2008758003961));
#32445=CARTESIAN_POINT('Ctrl Pts',(13.208423484496,-0.64043195068177,3.88285360784221));
#32446=CARTESIAN_POINT('Ctrl Pts',(13.2320376006459,-0.508085752511173,
3.59290636366459));
#32447=CARTESIAN_POINT('Ctrl Pts',(13.2556517167957,-0.253973266794505,
3.40052194335125));
#32448=CARTESIAN_POINT('Ctrl Pts',(13.2792658329456,0.0610056803032868,
3.3518066124833));
#32449=CARTESIAN_POINT('Ctrl Pts',(13.3028799490955,0.361364191435218,3.45843533922715));
#32450=CARTESIAN_POINT('Ctrl Pts',(13.3264940652453,0.575119258511334,3.69485380694));
#32451=CARTESIAN_POINT('Ctrl Pts',(13.3501081813952,0.65104299168552,4.00440268404554));
#32452=CARTESIAN_POINT('Ctrl Pts',(13.3737222975451,0.570939739771795,4.31289642727099));
#32453=CARTESIAN_POINT('Ctrl Pts',(13.3973364136949,0.354006804717113,4.54640236352309));
#32454=CARTESIAN_POINT('Ctrl Pts',(13.4209505298448,0.0522336745508671,
4.6489591696652));
#32455=CARTESIAN_POINT('Ctrl Pts',(13.4445646459947,-0.26205761933777,4.59598839317277));
#32456=CARTESIAN_POINT('Ctrl Pts',(13.4681787621445,-0.513544980480383,
4.40018484937968));
#32457=CARTESIAN_POINT('Ctrl Pts',(13.4917928782944,-0.64195771209056,4.10847422061066));
#32458=CARTESIAN_POINT('Ctrl Pts',(13.5154069944443,-0.616520809113462,
3.79076698974655));
#32459=CARTESIAN_POINT('Ctrl Pts',(13.5390211105941,-0.443330402422436,
3.52320390633144));
#32460=CARTESIAN_POINT('Ctrl Pts',(13.562635226744,-0.163892778617988,3.36990832590288));
#32461=CARTESIAN_POINT('Ctrl Pts',(13.5862493428939,0.154822890495328,3.36761860145296));
#32462=CARTESIAN_POINT('Ctrl Pts',(13.6098634590437,0.43643417612693,3.51688348138565));
#32463=CARTESIAN_POINT('Ctrl Pts',(13.6334775751936,0.613450973283793,3.78193059814177));
#32464=CARTESIAN_POINT('Ctrl Pts',(13.6570916913435,0.643449974253473,4.09923956510808));
#32465=CARTESIAN_POINT('Ctrl Pts',(13.6807058074933,0.519241709620395,4.39276507945606));
#32466=CARTESIAN_POINT('Ctrl Pts',(13.7043199236432,0.270593554659618,4.59216170834183));
#32467=CARTESIAN_POINT('Ctrl Pts',(13.7279340397931,-0.0429042293685969,
4.64964266158552));
#32468=CARTESIAN_POINT('Ctrl Pts',(13.7515481559429,-0.346119716157775,
4.55143222859795));
#32469=CARTESIAN_POINT('Ctrl Pts',(13.7751622720928,-0.566385203513325,
4.32106722332061));
#32470=CARTESIAN_POINT('Ctrl Pts',(13.7987763882427,-0.650912534047929,
4.01375622291695));
#32471=CARTESIAN_POINT('Ctrl Pts',(13.8223905043925,-0.57944414457563,3.70314844792952));
#32472=CARTESIAN_POINT('Ctrl Pts',(13.8460046205424,-0.369107932149097,
3.46368321387984));
#32473=CARTESIAN_POINT('Ctrl Pts',(13.8696187366923,-0.0703124342978696,
3.35275003110641));
#32474=CARTESIAN_POINT('Ctrl Pts',(13.8932328528421,0.245333927901481,3.3969348091043));
#32475=CARTESIAN_POINT('Ctrl Pts',(13.916846968992,0.502184306426786,3.58564835824111));
#32476=CARTESIAN_POINT('Ctrl Pts',(13.9404610851419,0.638682720042094,3.87366416276737));
#32477=CARTESIAN_POINT('Ctrl Pts',(13.9640752012917,0.62211637371287,4.19195723015293));
#32478=CARTESIAN_POINT('Ctrl Pts',(13.9876893174416,0.456455507660852,4.46424641105313));
#32479=CARTESIAN_POINT('Ctrl Pts',(14.0113034335915,0.181401901656729,4.62527570776815));
#32480=CARTESIAN_POINT('Ctrl Pts',(14.0349175497413,-0.137125932879425,
4.63645332836083));
#32481=CARTESIAN_POINT('Ctrl Pts',(14.0585316658912,-0.422790583021024,
4.49510047824495));
#32482=CARTESIAN_POINT('Ctrl Pts',(14.0821457820411,-0.60713052675338,4.23509335195577));
#32483=CARTESIAN_POINT('Ctrl Pts',(14.1057598981909,-0.645967413308333,
3.91874446730605));
#32484=CARTESIAN_POINT('Ctrl Pts',(14.1293740143408,-0.529993712466286,
3.62186903671368));
#32485=CARTESIAN_POINT('Ctrl Pts',(14.1529881304907,-0.287003328966194,
3.41561532377041));
#32486=CARTESIAN_POINT('Ctrl Pts',(14.1766022466405,0.0247694002478971,
3.34941346658496));
#32487=CARTESIAN_POINT('Ctrl Pts',(14.2002163627904,0.330605970264406,3.43912920108534));
#32488=CARTESIAN_POINT('Ctrl Pts',(14.2238304789403,0.557210518047066,3.66326152695696));
#32489=CARTESIAN_POINT('Ctrl Pts',(14.2474445950901,0.650275686248857,3.96809557204375));
#32490=CARTESIAN_POINT('Ctrl Pts',(14.27105871124,0.587497759452106,4.28057573538778));
#32491=CARTESIAN_POINT('Ctrl Pts',(14.2946728273899,0.383921904832036,4.52581397056352));
#32492=CARTESIAN_POINT('Ctrl Pts',(14.3182869435397,0.088336493108731,4.64503722732482));
#32493=CARTESIAN_POINT('Ctrl Pts',(14.3419010596896,-0.22841937412829,4.6096728222354));
#32494=CARTESIAN_POINT('Ctrl Pts',(14.3655151758395,-0.490432948250941,
4.42819608115853));
#32495=CARTESIAN_POINT('Ctrl Pts',(14.3891292919893,-0.634910852255616,
4.14409916841427));
#32496=CARTESIAN_POINT('Ctrl Pts',(14.4127434081392,-0.627227950688033,
3.82546788683648));
#32497=CARTESIAN_POINT('Ctrl Pts',(14.4363575242891,-0.469225504392149,
3.54866444115539));
#32498=CARTESIAN_POINT('Ctrl Pts',(14.4599716404389,-0.198769899531221,
3.38002670405092));
#32499=CARTESIAN_POINT('Ctrl Pts',(14.4835857565888,0.11932229545683,3.35996988316441));
#32500=CARTESIAN_POINT('Ctrl Pts',(14.5071998727387,0.408818071695872,3.49330073524378));
#32501=CARTESIAN_POINT('Ctrl Pts',(14.5308139888885,0.600337751131954,3.74806559342675));
#32502=CARTESIAN_POINT('Ctrl Pts',(14.5544281050384,0.647982309355475,4.06320828594604));
#32503=CARTESIAN_POINT('Ctrl Pts',(14.5780422211883,0.540333396317157,4.36320267272319));
#32504=CARTESIAN_POINT('Ctrl Pts',(14.6016563373381,0.303189823409542,4.57615301060753));
#32505=CARTESIAN_POINT('Ctrl Pts',(14.625270453488,-0.00661530128860875,
4.65102426869959));
#32506=CARTESIAN_POINT('Ctrl Pts',(14.6488845696379,-0.314835022974042,
4.56987302880665));
#32507=CARTESIAN_POINT('Ctrl Pts',(14.6724986857877,-0.547602339746838,
4.35214775046202));
#32508=CARTESIAN_POINT('Ctrl Pts',(14.6961128019376,-0.649132943719538,
4.05002781234082));
#32509=CARTESIAN_POINT('Ctrl Pts',(14.7197269180875,-0.595094318970103,
3.73591836064326));
#32510=CARTESIAN_POINT('Ctrl Pts',(14.7433410342373,-0.398437197867616,
3.48509791236843));
#32511=CARTESIAN_POINT('Ctrl Pts',(14.7669551503872,-0.1062918289807,3.35767733339665));
#32512=CARTESIAN_POINT('Ctrl Pts',(14.7905692665371,0.211327117384507,3.38419385377023));
#32513=CARTESIAN_POINT('Ctrl Pts',(14.8141833826869,0.478300047385911,3.5582926020622));
#32514=CARTESIAN_POINT('Ctrl Pts',(14.8377974988368,0.630645044771057,3.83824960712979));
#32515=CARTESIAN_POINT('Ctrl Pts',(14.8614116149867,0.631851559871185,4.15697121131127));
#32516=CARTESIAN_POINT('Ctrl Pts',(14.8850257311365,0.481630465478622,4.4380735902585));
#32517=CARTESIAN_POINT('Ctrl Pts',(14.9086398472864,0.215983244330552,4.61418854455152));
#32518=CARTESIAN_POINT('Ctrl Pts',(14.9322539634363,-0.101425794369151,
4.64310902247508));
#32519=CARTESIAN_POINT('Ctrl Pts',(14.9558680795861,-0.394527586443172,
4.517903766532));
#32520=CARTESIAN_POINT('Ctrl Pts',(14.979482195736,-0.593077772790822,4.26857965265179));
#32521=CARTESIAN_POINT('Ctrl Pts',(15.0030963118859,-0.649493436571599,
3.95488773069898));
#32522=CARTESIAN_POINT('Ctrl Pts',(15.0267104280357,-0.550252000240565,
3.65200904506483));
#32523=CARTESIAN_POINT('Ctrl Pts',(15.0503245441856,-0.319142060764588,
3.43252503194012));
#32524=CARTESIAN_POINT('Ctrl Pts',(15.0739386603355,-0.0115409051696555,
3.34904846156061));
#32525=CARTESIAN_POINT('Ctrl Pts',(15.0975527764853,0.298810377697559,3.42155963907315));
#32526=CARTESIAN_POINT('Ctrl Pts',(15.1211668926352,0.537575400322941,3.63273573589665));
#32527=CARTESIAN_POINT('Ctrl Pts',(15.1369096367351,0.610790903144771,3.83214323401692));
#32528=CARTESIAN_POINT('Ctrl Pts',(15.1447810087851,0.621570310124627,3.93461384266089));
#32529=CARTESIAN_POINT('Ctrl Pts',(12.4850729970716,0.282426015030316,4.49429601229446));
#32530=CARTESIAN_POINT('Ctrl Pts',(12.4929443691216,0.200937545576316,4.54085609598193));
#32531=CARTESIAN_POINT('Ctrl Pts',(12.5086871132215,0.0145627935155885,
4.59284387968754));
#32532=CARTESIAN_POINT('Ctrl Pts',(12.5323012293714,-0.268607755567932,
4.52871028073968));
#32533=CARTESIAN_POINT('Ctrl Pts',(12.5559153455213,-0.487363055256749,
4.3378665608173));
#32534=CARTESIAN_POINT('Ctrl Pts',(12.5795294616711,-0.589339580973024,
4.06604835489435));
#32535=CARTESIAN_POINT('Ctrl Pts',(12.603143577821,-0.550067261575934,3.77840176074865));
#32536=CARTESIAN_POINT('Ctrl Pts',(12.6267576939709,-0.378972002925158,
3.54386236016666));
#32537=CARTESIAN_POINT('Ctrl Pts',(12.6503718101207,-0.117051373585908,
3.41863967169675));
#32538=CARTESIAN_POINT('Ctrl Pts',(12.6739859262706,0.172920453180012,3.43274395851062));
#32539=CARTESIAN_POINT('Ctrl Pts',(12.6976000424204,0.42145114619533,3.58279513857084));
#32540=CARTESIAN_POINT('Ctrl Pts',(12.7212141585703,0.568977924911017,3.83283235195095));
#32541=CARTESIAN_POINT('Ctrl Pts',(12.7448282747202,0.580145282610399,4.12293246335278));
#32542=CARTESIAN_POINT('Ctrl Pts',(12.76844239087,0.45227673827436,4.38357095065208));
#32543=CARTESIAN_POINT('Ctrl Pts',(12.7920565070199,0.216016946852954,4.55228399108678));
#32544=CARTESIAN_POINT('Ctrl Pts',(12.8156706231698,-0.0720128197761896,
4.58863832766248));
#32545=CARTESIAN_POINT('Ctrl Pts',(12.8392847393196,-0.34278420811256,4.48392139165784));
#32546=CARTESIAN_POINT('Ctrl Pts',(12.8628988554695,-0.531404976945056,
4.26322932523642));
#32547=CARTESIAN_POINT('Ctrl Pts',(12.8865129716194,-0.592670842732518,
3.97945251867098));
#32548=CARTESIAN_POINT('Ctrl Pts',(12.9101270877692,-0.51189901575794,3.70060005900794));
#32549=CARTESIAN_POINT('Ctrl Pts',(12.9337412039191,-0.308447025930223,
3.49350087944474));
#32550=CARTESIAN_POINT('Ctrl Pts',(12.957355320069,-0.0310735592390789,
3.40778774002645));
#32551=CARTESIAN_POINT('Ctrl Pts',(12.9809694362188,0.253746902286204,3.46400239130434));
#32552=CARTESIAN_POINT('Ctrl Pts',(13.0045835523687,0.477755152237737,3.64867260076509));
#32553=CARTESIAN_POINT('Ctrl Pts',(13.0281976685186,0.587266054150949,3.91754086716214));
#32554=CARTESIAN_POINT('Ctrl Pts',(13.0518117846685,0.556034558024266,4.20617103876933));
#32555=CARTESIAN_POINT('Ctrl Pts',(13.0754259008183,0.391545509324759,4.44539088570928));
#32556=CARTESIAN_POINT('Ctrl Pts',(13.0990400169682,0.133219853633759,4.57786970637232));
#32557=CARTESIAN_POINT('Ctrl Pts',(13.122654133118,-0.157032867368526,4.57185802915678));
#32558=CARTESIAN_POINT('Ctrl Pts',(13.1462682492679,-0.409651568547275,
4.42879659435664));
#32559=CARTESIAN_POINT('Ctrl Pts',(13.1698823654178,-0.564094419600429,
4.1829710707208));
#32560=CARTESIAN_POINT('Ctrl Pts',(13.1934964815676,-0.583348116144335,
3.89329525626321));
#32561=CARTESIAN_POINT('Ctrl Pts',(13.2171105977175,-0.462798375770677,
3.62919197644995));
#32562=CARTESIAN_POINT('Ctrl Pts',(13.2407247138674,-0.231335782947555,
3.45395542080054));
#32563=CARTESIAN_POINT('Ctrl Pts',(13.2643388300172,0.055568040665587,3.40958224975729));
#32564=CARTESIAN_POINT('Ctrl Pts',(13.2879529461671,0.329154596505292,3.50670680265737));
#32565=CARTESIAN_POINT('Ctrl Pts',(13.311567062317,0.523856961936024,3.72205250428141));
#32566=CARTESIAN_POINT('Ctrl Pts',(13.3351811784668,0.593013359693284,4.00401025814095));
#32567=CARTESIAN_POINT('Ctrl Pts',(13.3587952946167,0.520049977633468,4.28500692572024));
#32568=CARTESIAN_POINT('Ctrl Pts',(13.3824094107666,0.322452998189994,4.49769969952106));
#32569=CARTESIAN_POINT('Ctrl Pts',(13.4060235269164,0.0475779130258999,
4.59111527567571));
#32570=CARTESIAN_POINT('Ctrl Pts',(13.4296376430663,-0.238699550200797,
4.5428659610613));
#32571=CARTESIAN_POINT('Ctrl Pts',(13.4532517592162,-0.467771004553565,
4.36451503980497));
#32572=CARTESIAN_POINT('Ctrl Pts',(13.476865875366,-0.584737881352888,4.09880555174689));
#32573=CARTESIAN_POINT('Ctrl Pts',(13.5004799915159,-0.561568254327815,
3.80941662539381));
#32574=CARTESIAN_POINT('Ctrl Pts',(13.5240941076658,-0.403814885886516,
3.56570233148043));
#32575=CARTESIAN_POINT('Ctrl Pts',(13.5477082238157,-0.149284468950505,
3.42607049712074));
#32576=CARTESIAN_POINT('Ctrl Pts',(13.5713223399655,0.141023010189178,3.42398486344345));
#32577=CARTESIAN_POINT('Ctrl Pts',(13.5949364561154,0.39753334322815,3.55994526707815));
#32578=CARTESIAN_POINT('Ctrl Pts',(13.6185505722652,0.55877204319843,3.8013678508274));
#32579=CARTESIAN_POINT('Ctrl Pts',(13.6421646884151,0.586097133215014,4.09039401187145));
#32580=CARTESIAN_POINT('Ctrl Pts',(13.665778804565,0.47295996523623,4.35775661870721));
#32581=CARTESIAN_POINT('Ctrl Pts',(13.6893929207148,0.24647464915429,4.53938036140496));
#32582=CARTESIAN_POINT('Ctrl Pts',(13.7130070368647,-0.0390800323908759,
4.59173784568287));
#32583=CARTESIAN_POINT('Ctrl Pts',(13.7366211530146,-0.315268912124245,
4.50228123595558));
#32584=CARTESIAN_POINT('Ctrl Pts',(13.7602352691644,-0.515901402373503,
4.29244943148197));
#32585=CARTESIAN_POINT('Ctrl Pts',(13.7838493853143,-0.59289453017979,4.01253008491428));
#32586=CARTESIAN_POINT('Ctrl Pts',(13.8074635014642,-0.527796356489121,
3.72960781627073));
#32587=CARTESIAN_POINT('Ctrl Pts',(13.831077617614,-0.336208111796874,3.51148691674935));
#32588=CARTESIAN_POINT('Ctrl Pts',(13.8546917337639,-0.0640452526541193,
3.4104415783338));
#32589=CARTESIAN_POINT('Ctrl Pts',(13.8783058499138,0.223466497127862,3.45068801978614));
#32590=CARTESIAN_POINT('Ctrl Pts',(13.9019199660636,0.457422945247278,3.62258090124322));
#32591=CARTESIAN_POINT('Ctrl Pts',(13.9255340822135,0.581754800262342,3.88492489705937));
#32592=CARTESIAN_POINT('Ctrl Pts',(13.9491481983634,0.566665067602596,4.17484744237197));
#32593=CARTESIAN_POINT('Ctrl Pts',(13.9727623145132,0.415770106744681,4.42286658094793));
#32594=CARTESIAN_POINT('Ctrl Pts',(13.9963764306631,0.165232945489059,4.56954279968241));
#32595=CARTESIAN_POINT('Ctrl Pts',(14.019990546813,-0.124903441395439,4.57972412169294));
#32596=CARTESIAN_POINT('Ctrl Pts',(14.0436046629628,-0.385105849054417,
4.45097052228405));
#32597=CARTESIAN_POINT('Ctrl Pts',(14.0672187791127,-0.553014959135429,
4.21413869785145));
#32598=CARTESIAN_POINT('Ctrl Pts',(14.0908328952626,-0.58839018453545,3.92598704378684));
#32599=CARTESIAN_POINT('Ctrl Pts',(14.1144470114124,-0.482753606228458,
3.65557310990793));
#32600=CARTESIAN_POINT('Ctrl Pts',(14.1380611275623,-0.261421765577673,
3.46770347791168));
#32601=CARTESIAN_POINT('Ctrl Pts',(14.1616752437122,0.0225616210391343,
3.40740241293002));
#32602=CARTESIAN_POINT('Ctrl Pts',(14.185289359862,0.301137958114838,3.48912148496193));
#32603=CARTESIAN_POINT('Ctrl Pts',(14.2089034760119,0.507544487205137,3.69327614952086));
#32604=CARTESIAN_POINT('Ctrl Pts',(14.2325175921618,0.592314446747875,3.97093932005559));
#32605=CARTESIAN_POINT('Ctrl Pts',(14.2561317083116,0.535132125826274,4.25556708484021));
#32606=CARTESIAN_POINT('Ctrl Pts',(14.2797458244615,0.349701665714674,4.47894641865396));
#32607=CARTESIAN_POINT('Ctrl Pts',(14.3033599406114,0.0804627670229728,
4.58754290912926));
#32608=CARTESIAN_POINT('Ctrl Pts',(14.3269740567612,-0.208059593914322,
4.55533065134682));
#32609=CARTESIAN_POINT('Ctrl Pts',(14.3505881729111,-0.44671902479684,4.39002953712461));
#32610=CARTESIAN_POINT('Ctrl Pts',(14.374202289061,-0.578319131624566,4.13125512920294));
#32611=CARTESIAN_POINT('Ctrl Pts',(14.3978164052108,-0.571321032683373,
3.84102451585645));
#32612=CARTESIAN_POINT('Ctrl Pts',(14.4214305213607,-0.427401871100662,
3.58889348396707));
#32613=CARTESIAN_POINT('Ctrl Pts',(14.4450446375106,-0.181052875819672,
3.43528699049651));
#32614=CARTESIAN_POINT('Ctrl Pts',(14.4686587536604,0.108686701521778,3.41701790091169));
#32615=CARTESIAN_POINT('Ctrl Pts',(14.4922728698103,0.372378754238714,3.53846452970905));
#32616=CARTESIAN_POINT('Ctrl Pts',(14.5158869859602,0.546827646247725,3.77052134686598));
#32617=CARTESIAN_POINT('Ctrl Pts',(14.53950110211,0.59022548618159,4.05757432072539));
#32618=CARTESIAN_POINT('Ctrl Pts',(14.5631152182599,0.492171679592087,4.3308292078278));
#32619=CARTESIAN_POINT('Ctrl Pts',(14.5867293344098,0.276165503816305,4.52479857226205));
#32620=CARTESIAN_POINT('Ctrl Pts',(14.6103434505596,-0.00602565743375084,
4.59299630554951));
#32621=CARTESIAN_POINT('Ctrl Pts',(14.6339575667095,-0.286772727926288,
4.51907834617235));
#32622=CARTESIAN_POINT('Ctrl Pts',(14.6575716828594,-0.49879271786407,4.32075964763751));
#32623=CARTESIAN_POINT('Ctrl Pts',(14.6811857990092,-0.591273560669336,
4.04556866666751));
#32624=CARTESIAN_POINT('Ctrl Pts',(14.7047999151591,-0.542051578672567,
3.75945683743125));
#32625=CARTESIAN_POINT('Ctrl Pts',(14.728414031309,-0.362923162297683,3.53099285177933));
#32626=CARTESIAN_POINT('Ctrl Pts',(14.7520281474588,-0.0968176839575538,
3.41492969374656));
#32627=CARTESIAN_POINT('Ctrl Pts',(14.7756422636087,0.192490826988301,3.43908270827084));
#32628=CARTESIAN_POINT('Ctrl Pts',(14.7992563797586,0.435667569828913,3.59766345479839));
#32629=CARTESIAN_POINT('Ctrl Pts',(14.8228704959084,0.574433549780463,3.85266695881428));
#32630=CARTESIAN_POINT('Ctrl Pts',(14.8464846120583,0.575532524168,4.14297984400973));
#32631=CARTESIAN_POINT('Ctrl Pts',(14.8700987282082,0.438701136655627,4.39902663091346));
#32632=CARTESIAN_POINT('Ctrl Pts',(14.893712844358,0.196731937819222,4.55944387228049));
#32633=CARTESIAN_POINT('Ctrl Pts',(14.9173269605079,-0.0923853752310475,
4.58578657160514));
#32634=CARTESIAN_POINT('Ctrl Pts',(14.9409410766578,-0.359362027571537,
4.47174127747511));
#32635=CARTESIAN_POINT('Ctrl Pts',(14.9645551928076,-0.540214773976066,
4.24464025294543));
#32636=CARTESIAN_POINT('Ctrl Pts',(14.9881693089575,-0.59160192159185,3.95890873763601));
#32637=CARTESIAN_POINT('Ctrl Pts',(15.0117834251074,-0.501206205285789,
3.68302663884805));
#32638=CARTESIAN_POINT('Ctrl Pts',(15.0353975412572,-0.290695865081771,
3.48310596742652));
#32639=CARTESIAN_POINT('Ctrl Pts',(15.0590116574071,-0.0105122258222001,
3.40706994202017));
#32640=CARTESIAN_POINT('Ctrl Pts',(15.082625773557,0.272176412698783,3.47311795657709));
#32641=CARTESIAN_POINT('Ctrl Pts',(15.1062398897068,0.489659512974156,3.66547122397039));
#32642=CARTESIAN_POINT('Ctrl Pts',(15.1219826338067,0.5563490739778,3.84710486709154));
#32643=CARTESIAN_POINT('Ctrl Pts',(15.1298540058567,0.566167676482186,3.94044192881839));
#32644=CARTESIAN_POINT('Ctrl Pts',(12.4701459941433,0.254789069842909,4.44592641788345));
#32645=CARTESIAN_POINT('Ctrl Pts',(12.4780173661933,0.181274697121691,4.48793034026739));
#32646=CARTESIAN_POINT('Ctrl Pts',(12.4937601102932,0.0131377437512366,
4.53483083224977));
#32647=CARTESIAN_POINT('Ctrl Pts',(12.517374226443,-0.242323003376296,4.47697306011837));
#32648=CARTESIAN_POINT('Ctrl Pts',(12.5409883425929,-0.439671888977142,
4.30480445207012));
#32649=CARTESIAN_POINT('Ctrl Pts',(12.5646024587428,-0.531669448515955,
4.05958515863483));
#32650=CARTESIAN_POINT('Ctrl Pts',(12.5882165748926,-0.496240142441994,
3.80008637217214));
#32651=CARTESIAN_POINT('Ctrl Pts',(12.6118306910425,-0.341887499674706,
3.58849794711368));
#32652=CARTESIAN_POINT('Ctrl Pts',(12.6354448071924,-0.105597250297878,
3.47552899021694));
#32653=CARTESIAN_POINT('Ctrl Pts',(12.6590589233422,0.155999231932725,3.4882530946792));
#32654=CARTESIAN_POINT('Ctrl Pts',(12.6826730394921,0.380209824197002,3.62362093815591));
#32655=CARTESIAN_POINT('Ctrl Pts',(12.706287155642,0.513300292941022,3.84919062944795));
#32656=CARTESIAN_POINT('Ctrl Pts',(12.7299012717918,0.52337486302099,4.11090284295443));
#32657=CARTESIAN_POINT('Ctrl Pts',(12.7535153879417,0.408018961865605,4.34603641497018));
#32658=CARTESIAN_POINT('Ctrl Pts',(12.7771295040916,0.194878495711741,4.49823995272895));
#32659=CARTESIAN_POINT('Ctrl Pts',(12.8007436202414,-0.0649659676909401,
4.53103681671432));
#32660=CARTESIAN_POINT('Ctrl Pts',(12.8243577363913,-0.30924088042124,4.43656701116699));
#32661=CARTESIAN_POINT('Ctrl Pts',(12.8479718525412,-0.479404065419363,
4.23747088215356));
#32662=CARTESIAN_POINT('Ctrl Pts',(12.871585968691,-0.534674727916345,3.9814632031866));
#32663=CARTESIAN_POINT('Ctrl Pts',(12.8952000848409,-0.461806870250484,
3.72989799658434));
#32664=CARTESIAN_POINT('Ctrl Pts',(12.9188142009908,-0.278263781132688,
3.54306461538724));
#32665=CARTESIAN_POINT('Ctrl Pts',(12.9424283171406,-0.0280328398727138,
3.46573897998727));
#32666=CARTESIAN_POINT('Ctrl Pts',(12.9660424332905,0.228916366652986,3.51645271720832));
#32667=CARTESIAN_POINT('Ctrl Pts',(12.9896565494404,0.431004172325429,3.68305192688505));
#32668=CARTESIAN_POINT('Ctrl Pts',(13.0132706655902,0.529798827743877,3.92560994866724));
#32669=CARTESIAN_POINT('Ctrl Pts',(13.0368847817401,0.501623505980173,4.1859960641053));
#32670=CARTESIAN_POINT('Ctrl Pts',(13.06049889789,0.353230619039521,4.40180692799916));
#32671=CARTESIAN_POINT('Ctrl Pts',(13.0841130140398,0.120183555287252,4.52132196448402));
#32672=CARTESIAN_POINT('Ctrl Pts',(13.1077271301897,-0.14166633412753,4.51589856308179));
#32673=CARTESIAN_POINT('Ctrl Pts',(13.1313412463396,-0.369564900381594,
4.38683647969259));
#32674=CARTESIAN_POINT('Ctrl Pts',(13.1549553624894,-0.508894665592834,
4.16506634104549));
#32675=CARTESIAN_POINT('Ctrl Pts',(13.1785694786393,-0.5262642816069,3.9037369046842));
#32676=CARTESIAN_POINT('Ctrl Pts',(13.2021835947892,-0.417510999030181,
3.66547758923531));
#32677=CARTESIAN_POINT('Ctrl Pts',(13.225797710939,-0.208698299100604,3.50738889824983));
#32678=CARTESIAN_POINT('Ctrl Pts',(13.2494118270889,0.0501304010278875,
3.46735788703128));
#32679=CARTESIAN_POINT('Ctrl Pts',(13.2730259432388,0.296945001575366,3.55497826608759));
#32680=CARTESIAN_POINT('Ctrl Pts',(13.2966400593886,0.472594665360713,3.74925120162283));
#32681=CARTESIAN_POINT('Ctrl Pts',(13.3202541755385,0.534983727701048,4.00361783223636));
#32682=CARTESIAN_POINT('Ctrl Pts',(13.3438682916884,0.469160215495142,4.25711742416948));
#32683=CARTESIAN_POINT('Ctrl Pts',(13.3674824078382,0.290899191662876,4.44899703551904));
#32684=CARTESIAN_POINT('Ctrl Pts',(13.3910965239881,0.0429221515009326,
4.53327138168622));
#32685=CARTESIAN_POINT('Ctrl Pts',(13.414710640138,-0.215341481063824,4.48974352894983));
#32686=CARTESIAN_POINT('Ctrl Pts',(13.4383247562878,-0.421997028626747,
4.32884523023027));
#32687=CARTESIAN_POINT('Ctrl Pts',(13.4619388724377,-0.527518050615216,
4.08913688288313));
#32688=CARTESIAN_POINT('Ctrl Pts',(13.4855529885876,-0.506615699542168,
3.82806626104107));
#32689=CARTESIAN_POINT('Ctrl Pts',(13.5091671047374,-0.364299369350597,
3.60820075662942));
#32690=CARTESIAN_POINT('Ctrl Pts',(13.5327812208873,-0.134676159283021,
3.48223266833859));
#32691=CARTESIAN_POINT('Ctrl Pts',(13.5563953370372,0.127223129883027,3.48035112543394));
#32692=CARTESIAN_POINT('Ctrl Pts',(13.580009453187,0.35863251032937,3.60300705277064));
#32693=CARTESIAN_POINT('Ctrl Pts',(13.6036235693369,0.504093113113068,3.82080510351303));
#32694=CARTESIAN_POINT('Ctrl Pts',(13.6272376854868,0.528744292176554,4.08154845863482));
#32695=CARTESIAN_POINT('Ctrl Pts',(13.6508518016366,0.426678220852065,4.32274815795836));
#32696=CARTESIAN_POINT('Ctrl Pts',(13.6744659177865,0.222355743648963,4.48659901446809));
#32697=CARTESIAN_POINT('Ctrl Pts',(13.6980800339364,-0.0352558354131549,
4.53383302978021));
#32698=CARTESIAN_POINT('Ctrl Pts',(13.7216941500862,-0.284418108090716,
4.45313024331322));
#32699=CARTESIAN_POINT('Ctrl Pts',(13.7453082662361,-0.465417601233682,
4.26383163964332));
#32700=CARTESIAN_POINT('Ctrl Pts',(13.768922382386,-0.534876526311652,4.01130394691162));
#32701=CARTESIAN_POINT('Ctrl Pts',(13.7925364985358,-0.476148568402614,
3.75606718461195));
#32702=CARTESIAN_POINT('Ctrl Pts',(13.8161506146857,-0.303308291444651,
3.55929061961886));
#32703=CARTESIAN_POINT('Ctrl Pts',(13.8397647308356,-0.0577780710103693,
3.46813312556118));
#32704=CARTESIAN_POINT('Ctrl Pts',(13.8633788469854,0.201599066354243,3.50444123046797));
#32705=CARTESIAN_POINT('Ctrl Pts',(13.8869929631353,0.412661584067771,3.65951344424533));
#32706=CARTESIAN_POINT('Ctrl Pts',(13.9106070792852,0.52482688048259,3.89618563135138));
#32707=CARTESIAN_POINT('Ctrl Pts',(13.934221195435,0.511213761492322,4.157737654591));
#32708=CARTESIAN_POINT('Ctrl Pts',(13.9578353115849,0.375084705828511,4.38148675084272));
#32709=CARTESIAN_POINT('Ctrl Pts',(13.9814494277348,0.149063989321389,4.51380989159668));
#32710=CARTESIAN_POINT('Ctrl Pts',(14.0050635438846,-0.112680949911453,
4.52299491502504));
#32711=CARTESIAN_POINT('Ctrl Pts',(14.0286776600345,-0.347421115087809,
4.40684056632315));
#32712=CARTESIAN_POINT('Ctrl Pts',(14.0522917761844,-0.498899391517477,
4.19318404374712));
#32713=CARTESIAN_POINT('Ctrl Pts',(14.0759058923342,-0.530812955762567,
3.93322962026762));
#32714=CARTESIAN_POINT('Ctrl Pts',(14.0995200084841,-0.435513499990629,
3.68927718310219));
#32715=CARTESIAN_POINT('Ctrl Pts',(14.123134124634,-0.235840202189154,3.51979163205294));
#32716=CARTESIAN_POINT('Ctrl Pts',(14.1467482407838,0.020353841830372,3.46539135927508));
#32717=CARTESIAN_POINT('Ctrl Pts',(14.1703623569337,0.271669945965271,3.53911376883853));
#32718=CARTESIAN_POINT('Ctrl Pts',(14.1939764730836,0.457878456363209,3.72329077208477));
#32719=CARTESIAN_POINT('Ctrl Pts',(14.2175905892334,0.534353207246894,3.97378306806742));
#32720=CARTESIAN_POINT('Ctrl Pts',(14.2412047053833,0.482766492200443,4.23055843429265));
#32721=CARTESIAN_POINT('Ctrl Pts',(14.2648188215332,0.315481426597312,4.4320788667444));
#32722=CARTESIAN_POINT('Ctrl Pts',(14.288432937683,0.0725890409372144,4.53004859093371));
#32723=CARTESIAN_POINT('Ctrl Pts',(14.3120470538329,-0.187699813700353,
4.50098848045824));
#32724=CARTESIAN_POINT('Ctrl Pts',(14.3356611699828,-0.40300510134274,4.35186299309067));
#32725=CARTESIAN_POINT('Ctrl Pts',(14.3592752861326,-0.521727410993515,
4.11841108999162));
#32726=CARTESIAN_POINT('Ctrl Pts',(14.3828894022825,-0.515414114678713,
3.85658114487643));
#32727=CARTESIAN_POINT('Ctrl Pts',(14.4065035184324,-0.385578237809175,
3.62912252677875));
#32728=CARTESIAN_POINT('Ctrl Pts',(14.4301176345822,-0.163335852108122,
3.49054727694211));
#32729=CARTESIAN_POINT('Ctrl Pts',(14.4537317507321,0.0980511075867261,
3.47406591865897));
#32730=CARTESIAN_POINT('Ctrl Pts',(14.477345866882,0.335939436781555,3.58362832417432));
#32731=CARTESIAN_POINT('Ctrl Pts',(14.5009599830318,0.493317541363497,3.79297710030521));
#32732=CARTESIAN_POINT('Ctrl Pts',(14.5245740991817,0.532468663007706,4.05194035550473));
#32733=CARTESIAN_POINT('Ctrl Pts',(14.5481882153316,0.444009962867018,4.2984557429324));
#32734=CARTESIAN_POINT('Ctrl Pts',(14.5718023314814,0.249141184223067,4.47344413391656));
#32735=CARTESIAN_POINT('Ctrl Pts',(14.5954164476313,-0.00543601357889273,
4.53496834239941));
#32736=CARTESIAN_POINT('Ctrl Pts',(14.6190305637812,-0.258710432878536,
4.46828366353805));
#32737=CARTESIAN_POINT('Ctrl Pts',(14.642644679931,-0.449983095981302,4.28937154481299));
#32738=CARTESIAN_POINT('Ctrl Pts',(14.6662587960809,-0.533414177619135,
4.0411095209942));
#32739=CARTESIAN_POINT('Ctrl Pts',(14.6898729122308,-0.489008838375032,
3.78299531421925));
#32740=CARTESIAN_POINT('Ctrl Pts',(14.7134870283806,-0.327409126727749,
3.57688779119022));
#32741=CARTESIAN_POINT('Ctrl Pts',(14.7371011445305,-0.0873435389344073,
3.47218205409647));
#32742=CARTESIAN_POINT('Ctrl Pts',(14.7607152606804,0.173654536592096,3.49397156277145));
#32743=CARTESIAN_POINT('Ctrl Pts',(14.7843293768302,0.393035092271916,3.63703430753458));
#32744=CARTESIAN_POINT('Ctrl Pts',(14.8079434929801,0.518222054789869,3.86708431049878));
#32745=CARTESIAN_POINT('Ctrl Pts',(14.8315576091299,0.519213488464815,4.12898847670818));
#32746=CARTESIAN_POINT('Ctrl Pts',(14.8551717252798,0.395771807832633,4.35997967156842));
#32747=CARTESIAN_POINT('Ctrl Pts',(14.8787858414297,0.177480631307892,4.50469920000947));
#32748=CARTESIAN_POINT('Ctrl Pts',(14.9023999575796,-0.0833449560929437,
4.52846412073519));
#32749=CARTESIAN_POINT('Ctrl Pts',(14.9260140737294,-0.324196468699902,
4.42557878841823));
#32750=CARTESIAN_POINT('Ctrl Pts',(14.9496281898793,-0.487351775161311,
4.22070085323907));
#32751=CARTESIAN_POINT('Ctrl Pts',(14.9732423060292,-0.533710406612102,
3.96292974457304));
#32752=CARTESIAN_POINT('Ctrl Pts',(14.996856422179,-0.452160410331013,3.71404423263127));
#32753=CARTESIAN_POINT('Ctrl Pts',(15.0204705383289,-0.262249669398955,
3.53368690291293));
#32754=CARTESIAN_POINT('Ctrl Pts',(15.0440846544788,-0.0094835464747447,
3.46509142247974));
#32755=CARTESIAN_POINT('Ctrl Pts',(15.0676987706286,0.245542447700007,3.52467627408104));
#32756=CARTESIAN_POINT('Ctrl Pts',(15.0913128867785,0.441743625625371,3.69820671204414));
#32757=CARTESIAN_POINT('Ctrl Pts',(15.1070556308784,0.501907244810829,3.86206650016617));
#32758=CARTESIAN_POINT('Ctrl Pts',(15.1149270029284,0.510765042839744,3.94627001497588));
#32759=CARTESIAN_POINT('Ctrl Pts',(12.4552189912149,0.227152124655503,4.39755682347243));
#32760=CARTESIAN_POINT('Ctrl Pts',(12.4630903632649,0.161611848667067,4.43500458455284));
#32761=CARTESIAN_POINT('Ctrl Pts',(12.4788331073648,0.0117126939868845,
4.476817784812));
#32762=CARTESIAN_POINT('Ctrl Pts',(12.5024472235147,-0.216038251184659,
4.42523583949706));
#32763=CARTESIAN_POINT('Ctrl Pts',(12.5260613396645,-0.391980722697534,
4.27174234332294));
#32764=CARTESIAN_POINT('Ctrl Pts',(12.5496754558144,-0.473999316058885,
4.05312196237532));
#32765=CARTESIAN_POINT('Ctrl Pts',(12.5732895719643,-0.442413023308054,
3.82177098359562));
#32766=CARTESIAN_POINT('Ctrl Pts',(12.5969036881141,-0.304802996424253,
3.6331335340607));
#32767=CARTESIAN_POINT('Ctrl Pts',(12.620517804264,-0.0941431270098475,
3.53241830873714));
#32768=CARTESIAN_POINT('Ctrl Pts',(12.6441319204139,0.139078010685439,3.54376223084778));
#32769=CARTESIAN_POINT('Ctrl Pts',(12.6677460365637,0.338968502198674,3.66444673774097));
#32770=CARTESIAN_POINT('Ctrl Pts',(12.6913601527136,0.457622660971028,3.86554890694496));
#32771=CARTESIAN_POINT('Ctrl Pts',(12.7149742688635,0.46660444343158,4.09887322255608));
#32772=CARTESIAN_POINT('Ctrl Pts',(12.7385883850133,0.36376118545685,4.30850187928827));
#32773=CARTESIAN_POINT('Ctrl Pts',(12.7622025011632,0.173740044570527,4.44419591437112));
#32774=CARTESIAN_POINT('Ctrl Pts',(12.7858166173131,-0.0579191156056905,
4.47343530576616));
#32775=CARTESIAN_POINT('Ctrl Pts',(12.809430733463,-0.275697552729921,4.38921263067613));
#32776=CARTESIAN_POINT('Ctrl Pts',(12.8330448496128,-0.42740315389367,4.2117124390707));
#32777=CARTESIAN_POINT('Ctrl Pts',(12.8566589657627,-0.476678613100171,
3.98347388770222));
#32778=CARTESIAN_POINT('Ctrl Pts',(12.8802730819125,-0.411714724743029,
3.75919593416074));
#32779=CARTESIAN_POINT('Ctrl Pts',(12.9038871980624,-0.248080536335154,
3.59262835132974));
#32780=CARTESIAN_POINT('Ctrl Pts',(12.9275013142123,-0.0249921205063485,
3.52369021994808));
#32781=CARTESIAN_POINT('Ctrl Pts',(12.9511154303621,0.204085831019768,3.5689030431123));
#32782=CARTESIAN_POINT('Ctrl Pts',(12.974729546512,0.384253192413122,3.71743125300502));
#32783=CARTESIAN_POINT('Ctrl Pts',(12.9983436626619,0.472331601336806,3.93367903017235));
#32784=CARTESIAN_POINT('Ctrl Pts',(13.0219577788117,0.44721245393608,4.16582108944128));
#32785=CARTESIAN_POINT('Ctrl Pts',(13.0455718949616,0.314915728754283,4.35822297028905));
#32786=CARTESIAN_POINT('Ctrl Pts',(13.0691860111115,0.107147256940744,4.46477422259573));
#32787=CARTESIAN_POINT('Ctrl Pts',(13.0928001272613,-0.126299800886535,
4.4599390970068));
#32788=CARTESIAN_POINT('Ctrl Pts',(13.1164142434112,-0.329478232215912,
4.34487636502855));
#32789=CARTESIAN_POINT('Ctrl Pts',(13.1400283595611,-0.453694911585238,
4.14716161137019));
#32790=CARTESIAN_POINT('Ctrl Pts',(13.1636424757109,-0.469180447069464,
3.9141785531052));
#32791=CARTESIAN_POINT('Ctrl Pts',(13.1872565918608,-0.372223622289685,
3.70176320202068));
#32792=CARTESIAN_POINT('Ctrl Pts',(13.2108707080107,-0.186060815253654,
3.56082237569912));
#32793=CARTESIAN_POINT('Ctrl Pts',(13.2344848241605,0.0446927613901878,
3.52513352430527));
#32794=CARTESIAN_POINT('Ctrl Pts',(13.2580989403104,0.26473540664544,3.60324972951781));
#32795=CARTESIAN_POINT('Ctrl Pts',(13.2817130564603,0.421332368785403,3.77644989896424));
#32796=CARTESIAN_POINT('Ctrl Pts',(13.3053271726101,0.476954095708811,4.00322540633176));
#32797=CARTESIAN_POINT('Ctrl Pts',(13.32894128876,0.418270453356816,4.22922792261873));
#32798=CARTESIAN_POINT('Ctrl Pts',(13.3525554049099,0.259345385135757,4.40029437151701));
#32799=CARTESIAN_POINT('Ctrl Pts',(13.3761695210597,0.0382663899759653,
4.47542748769673));
#32800=CARTESIAN_POINT('Ctrl Pts',(13.3997836372096,-0.19198341192685,4.43662109683837));
#32801=CARTESIAN_POINT('Ctrl Pts',(13.4233977533595,-0.376223052699929,
4.29317542065556));
#32802=CARTESIAN_POINT('Ctrl Pts',(13.4470118695093,-0.470298219877544,
4.07946821401937));
#32803=CARTESIAN_POINT('Ctrl Pts',(13.4706259856592,-0.451663144756522,
3.84671589668833));
#32804=CARTESIAN_POINT('Ctrl Pts',(13.4942401018091,-0.324783852814677,
3.65069918177841));
#32805=CARTESIAN_POINT('Ctrl Pts',(13.5178542179589,-0.120067849615538,
3.53839483955645));
#32806=CARTESIAN_POINT('Ctrl Pts',(13.5414683341088,0.113423249576877,3.53671738742444));
#32807=CARTESIAN_POINT('Ctrl Pts',(13.5650824502587,0.319731677430589,3.64606883846313));
#32808=CARTESIAN_POINT('Ctrl Pts',(13.5886965664085,0.449414183027706,3.84024235619866));
#32809=CARTESIAN_POINT('Ctrl Pts',(13.6123106825584,0.471391451138094,4.07270290539818));
#32810=CARTESIAN_POINT('Ctrl Pts',(13.6359247987083,0.380396476467901,4.28773969720951));
#32811=CARTESIAN_POINT('Ctrl Pts',(13.6595389148581,0.198236838143636,4.43381766753122));
#32812=CARTESIAN_POINT('Ctrl Pts',(13.683153031008,-0.0314316384354341,
4.47592821387755));
#32813=CARTESIAN_POINT('Ctrl Pts',(13.7067671471579,-0.253567304057185,
4.40397925067086));
#32814=CARTESIAN_POINT('Ctrl Pts',(13.7303812633077,-0.414933800093862,
4.23521384780468));
#32815=CARTESIAN_POINT('Ctrl Pts',(13.7539953794576,-0.476858522443512,
4.01007780890896));
#32816=CARTESIAN_POINT('Ctrl Pts',(13.7776094956075,-0.424500780316106,
3.78252655295316));
#32817=CARTESIAN_POINT('Ctrl Pts',(13.8012236117573,-0.270408471092428,
3.60709432248837));
#32818=CARTESIAN_POINT('Ctrl Pts',(13.8248377279072,-0.0515108893666192,
3.52582467278856));
#32819=CARTESIAN_POINT('Ctrl Pts',(13.8484518440571,0.179731635580624,3.55819444114981));
#32820=CARTESIAN_POINT('Ctrl Pts',(13.8720659602069,0.367900222888263,3.69644598724744));
#32821=CARTESIAN_POINT('Ctrl Pts',(13.8956800763568,0.467898960702838,3.90744636564338));
#32822=CARTESIAN_POINT('Ctrl Pts',(13.9192941925067,0.455762455382048,4.14062786681004));
#32823=CARTESIAN_POINT('Ctrl Pts',(13.9429083086565,0.33439930491234,4.34010692073752));
#32824=CARTESIAN_POINT('Ctrl Pts',(13.9665224248064,0.132895033153719,4.45807698351094));
#32825=CARTESIAN_POINT('Ctrl Pts',(13.9901365409563,-0.100458458427467,
4.46626570835715));
#32826=CARTESIAN_POINT('Ctrl Pts',(14.0137506571061,-0.309736381121202,
4.36271061036225));
#32827=CARTESIAN_POINT('Ctrl Pts',(14.037364773256,-0.444783823899526,4.1722293896428));
#32828=CARTESIAN_POINT('Ctrl Pts',(14.0609788894059,-0.473235726989685,
3.94047219674841));
#32829=CARTESIAN_POINT('Ctrl Pts',(14.0845930055557,-0.388273393752801,
3.72298125629644));
#32830=CARTESIAN_POINT('Ctrl Pts',(14.1082071217056,-0.210258638800633,
3.5718797861942));
#32831=CARTESIAN_POINT('Ctrl Pts',(14.1318212378555,0.0181460626216094,
3.52338030562014));
#32832=CARTESIAN_POINT('Ctrl Pts',(14.1554353540053,0.242201933815703,3.58910605271512));
#32833=CARTESIAN_POINT('Ctrl Pts',(14.1790494701552,0.40821242552128,3.75330539464867));
#32834=CARTESIAN_POINT('Ctrl Pts',(14.2026635863051,0.476391967745912,3.97662681607925));
#32835=CARTESIAN_POINT('Ctrl Pts',(14.2262777024549,0.430400858574612,4.20554978374509));
#32836=CARTESIAN_POINT('Ctrl Pts',(14.2498918186048,0.28126118747995,4.38521131483484));
#32837=CARTESIAN_POINT('Ctrl Pts',(14.2735059347547,0.0647153148514563,
4.47255427273816));
#32838=CARTESIAN_POINT('Ctrl Pts',(14.2971200509045,-0.167340033486385,
4.44664630956965));
#32839=CARTESIAN_POINT('Ctrl Pts',(14.3207341670544,-0.359291177888639,
4.31369644905674));
#32840=CARTESIAN_POINT('Ctrl Pts',(14.3443482832043,-0.465135690362464,
4.10556705078029));
#32841=CARTESIAN_POINT('Ctrl Pts',(14.3679623993541,-0.459507196674052,
3.87213777389641));
#32842=CARTESIAN_POINT('Ctrl Pts',(14.391576515504,-0.343754604517688,3.66935156959044));
#32843=CARTESIAN_POINT('Ctrl Pts',(14.4151906316539,-0.145618828396573,
3.5458075633877));
#32844=CARTESIAN_POINT('Ctrl Pts',(14.4388047478037,0.0874155136516737,
3.53111393640625));
#32845=CARTESIAN_POINT('Ctrl Pts',(14.4624188639536,0.299500119324396,3.6287921186396));
#32846=CARTESIAN_POINT('Ctrl Pts',(14.4860329801035,0.439807436479269,3.81543285374444));
#32847=CARTESIAN_POINT('Ctrl Pts',(14.5096470962533,0.474711839833821,4.04630639028407));
#32848=CARTESIAN_POINT('Ctrl Pts',(14.5332612124032,0.395848246141948,4.26608227803701));
#32849=CARTESIAN_POINT('Ctrl Pts',(14.5568753285531,0.22211686462983,4.42208969557108));
#32850=CARTESIAN_POINT('Ctrl Pts',(14.5804894447029,-0.00484636972403486,
4.47694037924932));
#32851=CARTESIAN_POINT('Ctrl Pts',(14.6041035608528,-0.230648137830783,
4.41748898090375));
#32852=CARTESIAN_POINT('Ctrl Pts',(14.6277176770027,-0.401173474098533,
4.25798344198848));
#32853=CARTESIAN_POINT('Ctrl Pts',(14.6513317931525,-0.475554794568933,
4.03665037532088));
#32854=CARTESIAN_POINT('Ctrl Pts',(14.6749459093024,-0.435966098077497,
3.80653379100725));
#32855=CARTESIAN_POINT('Ctrl Pts',(14.6985600254523,-0.291895091157815,
3.62278273060111));
#32856=CARTESIAN_POINT('Ctrl Pts',(14.7221741416021,-0.077869393911261,
3.52943441444639));
#32857=CARTESIAN_POINT('Ctrl Pts',(14.745788257752,0.15481824619589,3.54886041727207));
#32858=CARTESIAN_POINT('Ctrl Pts',(14.7694023739019,0.350402614714918,3.67640516027076));
#32859=CARTESIAN_POINT('Ctrl Pts',(14.7930164900517,0.462010559799276,3.88150166218328));
#32860=CARTESIAN_POINT('Ctrl Pts',(14.8166306062016,0.46289445276163,4.11499710940664));
#32861=CARTESIAN_POINT('Ctrl Pts',(14.8402447223515,0.352842479009638,4.32093271222338));
#32862=CARTESIAN_POINT('Ctrl Pts',(14.8638588385013,0.158229324796562,4.44995452773844));
#32863=CARTESIAN_POINT('Ctrl Pts',(14.8874729546512,-0.07430453695484,4.47114166986524));
#32864=CARTESIAN_POINT('Ctrl Pts',(14.9110870708011,-0.289030909828268,
4.37941629936134));
#32865=CARTESIAN_POINT('Ctrl Pts',(14.9347011869509,-0.434488776346555,
4.1967614535327));
#32866=CARTESIAN_POINT('Ctrl Pts',(14.9583153031008,-0.475818891632353,
3.96695075151007));
#32867=CARTESIAN_POINT('Ctrl Pts',(14.9819294192507,-0.403114615376237,
3.74506182641449));
#32868=CARTESIAN_POINT('Ctrl Pts',(15.0055435354005,-0.233803473716137,
3.58426783839933));
#32869=CARTESIAN_POINT('Ctrl Pts',(15.0291576515504,-0.00845486712728951,
3.5231129029393));
#32870=CARTESIAN_POINT('Ctrl Pts',(15.0527717677003,0.218908482701231,3.57623459158499));
#32871=CARTESIAN_POINT('Ctrl Pts',(15.0763858838501,0.393827738276586,3.73094220011788));
#32872=CARTESIAN_POINT('Ctrl Pts',(15.09212862795,0.447465415643859,3.87702813324079));
#32873=CARTESIAN_POINT('Ctrl Pts',(15.1,0.455362409197302,3.95209810113337));
#32874=CARTESIAN_POINT('',(15.1,0.455362409197302,3.95209810113338));
#32875=CARTESIAN_POINT('Ctrl Pts',(15.1,0.455362409197302,3.95209810113337));
#32876=CARTESIAN_POINT('Ctrl Pts',(15.1,0.461198486074795,3.93070554260298));
#32877=CARTESIAN_POINT('Ctrl Pts',(15.1,0.46535922191849,3.9089149747703));
#32878=CARTESIAN_POINT('Ctrl Pts',(15.1,0.467933495509747,3.88694781877637));
#32879=CARTESIAN_POINT('Ctrl Pts',(15.1,0.470556099470815,3.86456824322593));
#32880=CARTESIAN_POINT('Ctrl Pts',(15.1,0.471533159003394,3.84200460508655));
#32881=CARTESIAN_POINT('Ctrl Pts',(15.1,0.470938919222204,3.8194389967166));
#32882=CARTESIAN_POINT('Ctrl Pts',(15.1,0.470570970565677,3.80546654730098));
#32883=CARTESIAN_POINT('Ctrl Pts',(15.1,0.469600118414825,3.7914923521806));
#32884=CARTESIAN_POINT('Ctrl Pts',(15.1,0.468037922355437,3.77755218535593));
#32885=CARTESIAN_POINT('Ctrl Pts',(15.1,0.467305764617198,3.77101881782393));
#32886=CARTESIAN_POINT('Ctrl Pts',(15.1,0.466444065557791,3.76449770946228));
#32887=CARTESIAN_POINT('Ctrl Pts',(15.1,0.465455885979624,3.7580011302485));
#32888=CARTESIAN_POINT('Ctrl Pts',(15.1,0.462059294618766,3.73567095330476));
#32889=CARTESIAN_POINT('Ctrl Pts',(15.1,0.45716703427379,3.71360451488159));
#32890=CARTESIAN_POINT('Ctrl Pts',(15.1,0.450855318277529,3.69195899424001));
#32891=CARTESIAN_POINT('Ctrl Pts',(15.1,0.444011336009419,3.66848810937402));
#32892=CARTESIAN_POINT('Ctrl Pts',(15.1,0.435499564516811,3.64551127788848));
#32893=CARTESIAN_POINT('Ctrl Pts',(15.1,0.425460105602329,3.62314791088594));
#32894=CARTESIAN_POINT('Ctrl Pts',(15.1,0.421555366121865,3.61444992000866));
#32895=CARTESIAN_POINT('Ctrl Pts',(15.1,0.417417266816347,3.60584160863805));
#32896=CARTESIAN_POINT('Ctrl Pts',(15.1,0.413065612826793,3.5973533346642));
#32897=CARTESIAN_POINT('Ctrl Pts',(15.1,0.400188909388694,3.57223622128044));
#32898=CARTESIAN_POINT('Ctrl Pts',(15.1,0.385429835973237,3.54813135585314));
#32899=CARTESIAN_POINT('Ctrl Pts',(15.1,0.369010648251791,3.52520488756047));
#32900=CARTESIAN_POINT('Ctrl Pts',(15.1,0.352591460530346,3.50227841926781));
#32901=CARTESIAN_POINT('Ctrl Pts',(15.1,0.334512091502091,3.48052876229398));
#32902=CARTESIAN_POINT('Ctrl Pts',(15.1,0.31493781544227,3.46010549098216));
#32903=CARTESIAN_POINT('Ctrl Pts',(14.8800042915148,-1.01702808208336E-5,
4.45785711824254));
#32904=CARTESIAN_POINT('Ctrl Pts',(14.8824938458936,-0.0238866377941533,
4.45787702641871));
#32905=CARTESIAN_POINT('Ctrl Pts',(14.8849834002724,-0.0477600743578134,
4.45604121816599));
#32906=CARTESIAN_POINT('Ctrl Pts',(14.8874729546512,-0.0713366221418418,
4.45232291776013));
#32907=CARTESIAN_POINT('Ctrl Pts',(14.8953443267012,-0.145879994579315,
4.44056654636394));
#32908=CARTESIAN_POINT('Ctrl Pts',(14.9032156987511,-0.217455452203791,
4.40999142286264));
#32909=CARTESIAN_POINT('Ctrl Pts',(14.9110870708011,-0.277486158769077,
4.36426138680722));
#32910=CARTESIAN_POINT('Ctrl Pts',(14.918958442851,-0.337516865334364,4.31853135075179));
#32911=CARTESIAN_POINT('Ctrl Pts',(14.926829814901,-0.38600282084046,4.25764640214225));
#32912=CARTESIAN_POINT('Ctrl Pts',(14.9347011869509,-0.417134151141141,
4.18890214416703));
#32913=CARTESIAN_POINT('Ctrl Pts',(14.9425725590009,-0.448265481441821,
4.12015788619182));
#32914=CARTESIAN_POINT('Ctrl Pts',(14.9504439310508,-0.462042186537087,
4.04355431885095));
#32915=CARTESIAN_POINT('Ctrl Pts',(14.9583153031008,-0.456813159708701,
3.96827104766458));
#32916=CARTESIAN_POINT('Ctrl Pts',(14.9661866751508,-0.451584132880315,
3.89298777647821));
#32917=CARTESIAN_POINT('Ctrl Pts',(14.9740580472007,-0.427349374128277,
3.81902480144635));
#32918=CARTESIAN_POINT('Ctrl Pts',(14.9819294192507,-0.387013471142241,
3.7552443159279));
#32919=CARTESIAN_POINT('Ctrl Pts',(14.9898007913006,-0.346677568156205,
3.69146383040944));
#32920=CARTESIAN_POINT('Ctrl Pts',(14.9976721633506,-0.290240520936171,
3.63786583440439));
#32921=CARTESIAN_POINT('Ctrl Pts',(15.0055435354005,-0.224463896228013,
3.60087434715852));
#32922=CARTESIAN_POINT('Ctrl Pts',(15.0134149074505,-0.158687271519854,
3.56388285991266));
#32923=CARTESIAN_POINT('Ctrl Pts',(15.0212862795004,-0.0835710693235713,
3.54349788142598));
#32924=CARTESIAN_POINT('Ctrl Pts',(15.0291576515504,-0.00811907658734153,
3.54215900695692));
#32925=CARTESIAN_POINT('Ctrl Pts',(15.0370290236004,0.067332916148885,3.54082013248786));
#32926=CARTESIAN_POINT('Ctrl Pts',(15.0449003956503,0.143120699425059,3.55852736203643));
#32927=CARTESIAN_POINT('Ctrl Pts',(15.0527717677003,0.210167800325704,3.59316557823286));
#32928=CARTESIAN_POINT('Ctrl Pts',(15.0606431397502,0.27721490122635,3.62780379442929));
#32929=CARTESIAN_POINT('Ctrl Pts',(15.0685145118002,0.335521319751467,3.67937299727358));
#32930=CARTESIAN_POINT('Ctrl Pts',(15.0763858838501,0.378083948355844,3.74167908197646));
#32931=CARTESIAN_POINT('Ctrl Pts',(15.0842572559001,0.420646576960222,3.80398516667934));
#32932=CARTESIAN_POINT('Ctrl Pts',(15.09212862795,0.447465415643859,3.87702813324079));
#32933=CARTESIAN_POINT('Ctrl Pts',(15.1,0.455362409197302,3.95209810113337));
#32934=CARTESIAN_POINT('Ctrl Pts',(12.5,0.310062960217722,4.54266560670548));
#32935=CARTESIAN_POINT('Ctrl Pts',(12.5,0.283442099593322,4.54921865641189));
#32936=CARTESIAN_POINT('Ctrl Pts',(12.5,0.256466577744696,4.55390832200786));
#32937=CARTESIAN_POINT('Ctrl Pts',(12.5,0.229324391633413,4.55669460918752));
#32938=CARTESIAN_POINT('Ctrl Pts',(12.5,0.202804350211112,4.55941702996513));
#32939=CARTESIAN_POINT('Ctrl Pts',(12.5,0.176124140498118,4.56032157710196));
#32940=CARTESIAN_POINT('Ctrl Pts',(12.5,0.149491279718871,4.55933465732487));
#32941=CARTESIAN_POINT('Ctrl Pts',(12.5,0.131604301980395,4.55867182909064));
#32942=CARTESIAN_POINT('Ctrl Pts',(12.5,0.113739373486447,4.5571550748263));
#32943=CARTESIAN_POINT('Ctrl Pts',(12.5,0.0959711573489174,4.5547553284502));
#32944=CARTESIAN_POINT('Ctrl Pts',(12.5,0.0885102514788159,4.55374767063663));
#32945=CARTESIAN_POINT('Ctrl Pts',(12.5,0.0810658284660142,4.55258395860043));
#32946=CARTESIAN_POINT('Ctrl Pts',(12.5,0.0736590895785168,4.55126509319275));
#32947=CARTESIAN_POINT('Ctrl Pts',(12.5,0.0532014046082737,4.54762233847462));
#32948=CARTESIAN_POINT('Ctrl Pts',(12.5,0.0329999615976937,4.54279338637244));
#32949=CARTESIAN_POINT('Ctrl Pts',(12.5,0.0131662989716721,4.53674486487483));
#32950=CARTESIAN_POINT('Ctrl Pts',(12.5,-0.00550403753485725,4.53105111411095));
#32951=CARTESIAN_POINT('Ctrl Pts',(12.5,-0.0238485481480196,4.52427602479051));
#32952=CARTESIAN_POINT('Ctrl Pts',(12.5,-0.0417515783368052,4.51643454453567));
#32953=CARTESIAN_POINT('Ctrl Pts',(12.5,-0.0500477299146631,4.51280085190917));
#32954=CARTESIAN_POINT('Ctrl Pts',(12.5,-0.058248775177811,4.50893813195896));
#32955=CARTESIAN_POINT('Ctrl Pts',(12.5,-0.0663415323109863,4.50484786558969));
#32956=CARTESIAN_POINT('Ctrl Pts',(12.5,-0.0727048112135971,4.50163171746301));
#32957=CARTESIAN_POINT('Ctrl Pts',(12.5,-0.0789919703630761,4.49827952355299));
#32958=CARTESIAN_POINT('Ctrl Pts',(12.5,-0.085197598682301,4.4947927546146));
#32959=CARTESIAN_POINT('Ctrl Pts',(12.5,-0.104491803581693,4.48395188067351));
#32960=CARTESIAN_POINT('Ctrl Pts',(12.5,-0.123002674071495,4.47180959856144));
#32961=CARTESIAN_POINT('Ctrl Pts',(12.5,-0.140547257611399,4.45840101528927));
#32962=CARTESIAN_POINT('Ctrl Pts',(12.5,-0.156644205929787,4.44609879839914));
#32963=CARTESIAN_POINT('Ctrl Pts',(12.5,-0.17192740174072,4.43272977950413));
#32964=CARTESIAN_POINT('Ctrl Pts',(12.5,-0.186217277007305,4.41832740439832));
#32965=CARTESIAN_POINT('Origin',(15.1,0.,4.));
#32966=CARTESIAN_POINT('',(15.1,-1.16619037896906,2.5));
#32967=CARTESIAN_POINT('',(15.1,1.16619037896906,2.5));
#32968=CARTESIAN_POINT('',(15.1,1.25,2.5));
#32969=CARTESIAN_POINT('Origin',(15.1,0.,4.));
#32970=CARTESIAN_POINT('Origin',(15.1,0.,4.));
#32971=CARTESIAN_POINT('',(15.1,2.75545529808154E-17,5.725));
#32972=CARTESIAN_POINT('Origin',(15.1,0.,5.5));
#32973=CARTESIAN_POINT('',(15.1,1.5,4.225));
#32974=CARTESIAN_POINT('Origin',(15.1,1.5,4.));
#32975=CARTESIAN_POINT('',(15.1,-1.5,4.225));
#32976=CARTESIAN_POINT('Origin',(15.1,-1.5,4.));
#32977=CARTESIAN_POINT('Origin',(14.4,-1.5,4.));
#32978=CARTESIAN_POINT('',(14.5,-1.5,4.225));
#32979=CARTESIAN_POINT('Origin',(14.5,-1.5,4.));
#32980=CARTESIAN_POINT('',(14.4,-1.5,4.225));
#32981=CARTESIAN_POINT('Origin',(14.4,1.5,4.));
#32982=CARTESIAN_POINT('',(14.5,1.5,4.225));
#32983=CARTESIAN_POINT('Origin',(14.5,1.5,4.));
#32984=CARTESIAN_POINT('',(14.4,1.5,4.225));
#32985=CARTESIAN_POINT('Origin',(14.4,0.,5.5));
#32986=CARTESIAN_POINT('',(14.5,-2.75545529808154E-17,5.725));
#32987=CARTESIAN_POINT('Origin',(14.5,0.,5.5));
#32988=CARTESIAN_POINT('',(14.4,-2.75545529808154E-17,5.725));
#32989=CARTESIAN_POINT('Origin',(14.4,2.5,2.5));
#32990=CARTESIAN_POINT('',(14.5,1.16619037896906,2.5));
#32991=CARTESIAN_POINT('',(14.5,-1.16619037896906,2.5));
#32992=CARTESIAN_POINT('',(14.5,1.25,2.5));
#32993=CARTESIAN_POINT('',(14.5,1.16619037896906,2.5));
#32994=CARTESIAN_POINT('',(14.5,-1.16619037896906,2.5));
#32995=CARTESIAN_POINT('Origin',(14.5,0.,4.));
#32996=CARTESIAN_POINT('Origin',(14.5,0.,4.));
#32997=CARTESIAN_POINT('',(14.5,-1.34711147906209E-16,5.1));
#32998=CARTESIAN_POINT('Origin',(14.5,0.,4.));
#32999=CARTESIAN_POINT('Origin',(14.5,0.,4.));
#33000=CARTESIAN_POINT('Origin',(12.5,0.,4.));
#33001=CARTESIAN_POINT('Origin',(12.5,0.,4.));
#33002=CARTESIAN_POINT('',(12.5,-1.34711147906209E-16,5.1));
#33003=CARTESIAN_POINT('',(12.5,-1.34711147906209E-16,5.1));
#33004=CARTESIAN_POINT('Origin',(12.5,0.,4.));
#33005=CARTESIAN_POINT('Origin',(12.5,0.,4.));
#33006=CARTESIAN_POINT('',(0.,0.,0.));
#33007=CARTESIAN_POINT('Origin',(0.0866025403784439,-0.4,-0.15));
#33008=CARTESIAN_POINT('',(0.173205080756888,-0.4,0.));
#33009=CARTESIAN_POINT('',(0.0866025403784439,-0.4,-0.15));
#33010=CARTESIAN_POINT('',(0.173205080756888,-0.4,0.));
#33011=CARTESIAN_POINT('',(0.0866025403784439,-0.64,-0.15));
#33012=CARTESIAN_POINT('',(0.0866025403784439,-0.4,-0.15));
#33013=CARTESIAN_POINT('',(0.173205080756888,-0.64,0.));
#33014=CARTESIAN_POINT('',(0.173205080756888,-0.64,0.));
#33015=CARTESIAN_POINT('',(0.173205080756888,-0.4,0.));
#33016=CARTESIAN_POINT('Origin',(-0.0866025403784438,-0.4,-0.15));
#33017=CARTESIAN_POINT('',(-0.0866025403784438,-0.4,-0.15));
#33018=CARTESIAN_POINT('',(0.0866025403784439,-0.4,-0.15));
#33019=CARTESIAN_POINT('',(-0.0866025403784438,-0.64,-0.15));
#33020=CARTESIAN_POINT('',(-0.0866025403784438,-0.4,-0.15));
#33021=CARTESIAN_POINT('',(0.0866025403784439,-0.64,-0.15));
#33022=CARTESIAN_POINT('Origin',(-0.173205080756888,-0.4,-2.77555756156289E-17));
#33023=CARTESIAN_POINT('',(-0.173205080756888,-0.4,-2.12115047744981E-17));
#33024=CARTESIAN_POINT('',(-0.0866025403784438,-0.4,-0.15));
#33025=CARTESIAN_POINT('',(-0.173205080756888,-0.64,-2.77555756156289E-17));
#33026=CARTESIAN_POINT('',(-0.173205080756888,-0.4,-2.12115047744981E-17));
#33027=CARTESIAN_POINT('',(-0.0866025403784438,-0.64,-0.15));
#33028=CARTESIAN_POINT('Origin',(-0.0866025403784439,-0.4,0.15));
#33029=CARTESIAN_POINT('',(-0.0866025403784439,-0.4,0.15));
#33030=CARTESIAN_POINT('',(-0.173205080756888,-0.4,-2.12115047744981E-17));
#33031=CARTESIAN_POINT('',(-0.0866025403784439,-0.64,0.15));
#33032=CARTESIAN_POINT('',(-0.0866025403784439,-0.4,0.15));
#33033=CARTESIAN_POINT('',(-0.173205080756888,-0.64,-2.12115047744981E-17));
#33034=CARTESIAN_POINT('Origin',(0.0866025403784439,-0.4,0.15));
#33035=CARTESIAN_POINT('',(0.0866025403784439,-0.4,0.15));
#33036=CARTESIAN_POINT('',(-0.0866025403784439,-0.4,0.15));
#33037=CARTESIAN_POINT('',(0.0866025403784439,-0.64,0.15));
#33038=CARTESIAN_POINT('',(0.0866025403784439,-0.4,0.15));
#33039=CARTESIAN_POINT('',(-0.0866025403784439,-0.64,0.15));
#33040=CARTESIAN_POINT('Origin',(0.173205080756888,-0.4,0.));
#33041=CARTESIAN_POINT('',(0.0866025403784439,-0.4,0.15));
#33042=CARTESIAN_POINT('',(0.0866025403784439,-0.64,0.15));
#33043=CARTESIAN_POINT('Origin',(0.,-0.4,-2.77555756156289E-17));
#33044=CARTESIAN_POINT('Origin',(0.,-0.64,-2.77555756156289E-17));
#33045=CARTESIAN_POINT('Origin',(0.,-1.5,0.));
#33046=CARTESIAN_POINT('',(-0.2,-1.5,2.44929359829471E-17));
#33047=CARTESIAN_POINT('Origin',(0.,-1.5,0.));
#33048=CARTESIAN_POINT('',(-0.1954,-1.5,2.39295984553393E-17));
#33049=CARTESIAN_POINT('Origin',(0.,-1.5,0.));
#33050=CARTESIAN_POINT('Origin',(0.,-3.,0.));
#33051=CARTESIAN_POINT('',(-0.2,-3.,2.44929359829471E-17));
#33052=CARTESIAN_POINT('',(-0.2,-3.,2.44929359829471E-17));
#33053=CARTESIAN_POINT('Origin',(0.,-3.,0.));
#33054=CARTESIAN_POINT('Origin',(0.,-3.,0.));
#33055=CARTESIAN_POINT('Origin',(0.3,0.4,0.));
#33056=CARTESIAN_POINT('',(-0.3,0.4,-3.67394039744206E-17));
#33057=CARTESIAN_POINT('Origin',(0.,0.4,0.));
#33058=CARTESIAN_POINT('Origin',(0.,0.375,0.));
#33059=CARTESIAN_POINT('',(-0.35,0.35,-4.28626379701573E-17));
#33060=CARTESIAN_POINT('Origin',(0.,0.35,0.));
#33061=CARTESIAN_POINT('',(-0.325,0.375,-3.9801020972289E-17));
#33062=CARTESIAN_POINT('Origin',(0.,0.19,0.));
#33063=CARTESIAN_POINT('',(-0.35,0.03,-4.28626379701574E-17));
#33064=CARTESIAN_POINT('Origin',(0.,0.03,0.));
#33065=CARTESIAN_POINT('',(-0.35,0.19,-4.28626379701574E-17));
#33066=CARTESIAN_POINT('Origin',(0.,0.0149999999999999,0.));
#33067=CARTESIAN_POINT('',(-0.32,-3.29597460435593E-17,-3.91886975727153E-17));
#33068=CARTESIAN_POINT('Origin',(0.,0.,0.));
#33069=CARTESIAN_POINT('',(-0.335,0.0149999999999999,-4.10256677714363E-17));
#33070=CARTESIAN_POINT('Origin',(0.22,0.,0.));
#33071=CARTESIAN_POINT('',(-0.22,-6.93889390390723E-18,-2.69422295812418E-17));
#33072=CARTESIAN_POINT('Origin',(0.,0.,0.));
#33073=CARTESIAN_POINT('Origin',(0.,-0.02,0.));
#33074=CARTESIAN_POINT('',(-0.1954,-0.0492,2.39295984553393E-17));
#33075=CARTESIAN_POINT('Origin',(0.,-0.0492,0.));
#33076=CARTESIAN_POINT('',(-0.21,-0.02,-2.57175827820944E-17));
#33077=CARTESIAN_POINT('Origin',(0.,-0.8,0.));
#33078=CARTESIAN_POINT('',(-0.1954,-0.8,-2.39295984553393E-17));
#33079=CARTESIAN_POINT('',(0.,0.,0.));
#33080=CARTESIAN_POINT('Origin',(0.3,0.4,0.));
#33081=CARTESIAN_POINT('',(-0.3,0.4,-3.67394039744206E-17));
#33082=CARTESIAN_POINT('Origin',(0.,0.4,0.));
#33083=CARTESIAN_POINT('Origin',(0.,0.375,0.));
#33084=CARTESIAN_POINT('',(-0.35,0.35,-4.28626379701573E-17));
#33085=CARTESIAN_POINT('Origin',(0.,0.35,0.));
#33086=CARTESIAN_POINT('',(-0.325,0.375,-3.9801020972289E-17));
#33087=CARTESIAN_POINT('Origin',(0.,0.19,0.));
#33088=CARTESIAN_POINT('',(-0.35,0.03,-4.28626379701574E-17));
#33089=CARTESIAN_POINT('Origin',(0.,0.03,0.));
#33090=CARTESIAN_POINT('',(-0.35,0.19,-4.28626379701574E-17));
#33091=CARTESIAN_POINT('Origin',(0.,0.0149999999999999,0.));
#33092=CARTESIAN_POINT('',(-0.32,-3.29597460435593E-17,-3.91886975727153E-17));
#33093=CARTESIAN_POINT('Origin',(0.,0.,0.));
#33094=CARTESIAN_POINT('',(-0.335,0.0149999999999999,-4.10256677714363E-17));
#33095=CARTESIAN_POINT('Origin',(0.22,0.,0.));
#33096=CARTESIAN_POINT('',(-0.22,-6.93889390390723E-18,-2.69422295812418E-17));
#33097=CARTESIAN_POINT('Origin',(0.,0.,0.));
#33098=CARTESIAN_POINT('Origin',(0.,-0.02,0.));
#33099=CARTESIAN_POINT('',(-0.1954,-0.0492,2.39295984553393E-17));
#33100=CARTESIAN_POINT('Origin',(0.,-0.0492,0.));
#33101=CARTESIAN_POINT('',(-0.21,-0.02,-2.57175827820944E-17));
#33102=CARTESIAN_POINT('Origin',(0.,-0.8,0.));
#33103=CARTESIAN_POINT('',(-0.1954,-1.5646,2.39295984553393E-17));
#33104=CARTESIAN_POINT('Origin',(0.,-1.5646,0.));
#33105=CARTESIAN_POINT('',(-0.1954,-0.8,-2.39295984553393E-17));
#33106=CARTESIAN_POINT('Origin',(0.,-1.58,0.));
#33107=CARTESIAN_POINT('',(-0.16,-1.6,-1.95943487863577E-17));
#33108=CARTESIAN_POINT('Origin',(0.,-1.6,0.));
#33109=CARTESIAN_POINT('',(-0.18,-1.58,-2.20436423846524E-17));
#33110=CARTESIAN_POINT('Origin',(0.,-1.6,0.));
#33111=CARTESIAN_POINT('Origin',(0.0866025403784439,-0.4,-0.15));
#33112=CARTESIAN_POINT('',(0.173205080756888,-0.4,0.));
#33113=CARTESIAN_POINT('',(0.0866025403784439,-0.4,-0.15));
#33114=CARTESIAN_POINT('',(0.173205080756888,-0.4,0.));
#33115=CARTESIAN_POINT('',(0.0866025403784439,-0.64,-0.15));
#33116=CARTESIAN_POINT('',(0.0866025403784439,-0.4,-0.15));
#33117=CARTESIAN_POINT('',(0.173205080756888,-0.64,0.));
#33118=CARTESIAN_POINT('',(0.173205080756888,-0.64,0.));
#33119=CARTESIAN_POINT('',(0.173205080756888,-0.4,0.));
#33120=CARTESIAN_POINT('Origin',(-0.0866025403784438,-0.4,-0.15));
#33121=CARTESIAN_POINT('',(-0.0866025403784438,-0.4,-0.15));
#33122=CARTESIAN_POINT('',(0.0866025403784439,-0.4,-0.15));
#33123=CARTESIAN_POINT('',(-0.0866025403784438,-0.64,-0.15));
#33124=CARTESIAN_POINT('',(-0.0866025403784438,-0.4,-0.15));
#33125=CARTESIAN_POINT('',(0.0866025403784439,-0.64,-0.15));
#33126=CARTESIAN_POINT('Origin',(-0.173205080756888,-0.4,-2.77555756156289E-17));
#33127=CARTESIAN_POINT('',(-0.173205080756888,-0.4,-2.12115047744981E-17));
#33128=CARTESIAN_POINT('',(-0.0866025403784438,-0.4,-0.15));
#33129=CARTESIAN_POINT('',(-0.173205080756888,-0.64,-2.77555756156289E-17));
#33130=CARTESIAN_POINT('',(-0.173205080756888,-0.4,-2.12115047744981E-17));
#33131=CARTESIAN_POINT('',(-0.0866025403784438,-0.64,-0.15));
#33132=CARTESIAN_POINT('Origin',(-0.0866025403784439,-0.4,0.15));
#33133=CARTESIAN_POINT('',(-0.0866025403784439,-0.4,0.15));
#33134=CARTESIAN_POINT('',(-0.173205080756888,-0.4,-2.12115047744981E-17));
#33135=CARTESIAN_POINT('',(-0.0866025403784439,-0.64,0.15));
#33136=CARTESIAN_POINT('',(-0.0866025403784439,-0.4,0.15));
#33137=CARTESIAN_POINT('',(-0.173205080756888,-0.64,-2.12115047744981E-17));
#33138=CARTESIAN_POINT('Origin',(0.0866025403784439,-0.4,0.15));
#33139=CARTESIAN_POINT('',(0.0866025403784439,-0.4,0.15));
#33140=CARTESIAN_POINT('',(-0.0866025403784439,-0.4,0.15));
#33141=CARTESIAN_POINT('',(0.0866025403784439,-0.64,0.15));
#33142=CARTESIAN_POINT('',(0.0866025403784439,-0.4,0.15));
#33143=CARTESIAN_POINT('',(-0.0866025403784439,-0.64,0.15));
#33144=CARTESIAN_POINT('Origin',(0.173205080756888,-0.4,0.));
#33145=CARTESIAN_POINT('',(0.0866025403784439,-0.4,0.15));
#33146=CARTESIAN_POINT('',(0.0866025403784439,-0.64,0.15));
#33147=CARTESIAN_POINT('Origin',(0.,-0.4,-2.77555756156289E-17));
#33148=CARTESIAN_POINT('Origin',(0.,-0.64,-2.77555756156289E-17));
#33149=CARTESIAN_POINT('',(0.,0.,0.));
#33150=CARTESIAN_POINT('',(0.,0.,0.));
#33151=CARTESIAN_POINT('',(0.,0.,0.));
#33152=CARTESIAN_POINT('',(0.,0.,0.));
#33153=CARTESIAN_POINT('',(0.,0.,0.));
#33154=CARTESIAN_POINT('',(0.,0.,0.));
#33155=CARTESIAN_POINT('',(0.,0.,0.));
#33156=CARTESIAN_POINT('',(0.,0.,0.));
#33157=CARTESIAN_POINT('',(0.,0.,0.));
#33158=CARTESIAN_POINT('',(0.,0.,0.));
#33159=CARTESIAN_POINT('',(0.,0.,0.));
#33160=CARTESIAN_POINT('',(0.,0.,0.));
#33161=CARTESIAN_POINT('',(0.,0.,0.));
#33162=CARTESIAN_POINT('',(0.,0.,0.));
#33163=CARTESIAN_POINT('',(0.,0.,0.));
#33164=CARTESIAN_POINT('',(0.,0.,0.));
#33165=CARTESIAN_POINT('',(0.,0.,0.));
#33166=CARTESIAN_POINT('',(0.,0.,0.));
#33167=CARTESIAN_POINT('',(0.,0.,0.));
#33168=CARTESIAN_POINT('',(0.,0.,0.));
#33169=CARTESIAN_POINT('',(-7.,9.5,-1.2));
#33170=CARTESIAN_POINT('',(-7.,9.5,31.5));
#33171=CARTESIAN_POINT('',(-7.,10.5,-1.2));
#33172=CARTESIAN_POINT('',(-7.,10.5,31.5));
#33173=CARTESIAN_POINT('',(7.,9.5,-1.2));
#33174=CARTESIAN_POINT('',(7.,9.5,31.5));
#33175=CARTESIAN_POINT('',(7.,10.5,-1.2));
#33176=CARTESIAN_POINT('',(7.,10.5,31.5));
#33177=CARTESIAN_POINT('',(-6.,0.,0.5));
#33178=CARTESIAN_POINT('',(-6.,2.3,1.2));
#33179=CARTESIAN_POINT('',(-7.6,1.7,1.2));
#33180=CARTESIAN_POINT('',(-4.4,1.7,1.2));
#33181=CARTESIAN_POINT('',(-4.8,-1.05,1.2));
#33182=CARTESIAN_POINT('',(-7.6,2.7,-1.2));
#33183=CARTESIAN_POINT('',(-4.4,2.7,-1.2));
#33184=CARTESIAN_POINT('',(-6.,2.3,29.8));
#33185=CARTESIAN_POINT('',(-7.6,1.7,29.8));
#33186=CARTESIAN_POINT('',(-4.4,1.7,29.8));
#33187=CARTESIAN_POINT('',(-4.8,-1.05,29.8));
#33188=CARTESIAN_POINT('',(-7.,5.5,31.5));
#33189=CARTESIAN_POINT('',(-5.,5.5,31.5));
#33190=CARTESIAN_POINT('',(6.,0.,0.5));
#33191=CARTESIAN_POINT('',(6.,2.3,1.2));
#33192=CARTESIAN_POINT('',(4.4,1.7,1.2));
#33193=CARTESIAN_POINT('',(7.6,1.7,1.2));
#33194=CARTESIAN_POINT('',(7.2,-1.05,1.2));
#33195=CARTESIAN_POINT('',(4.4,2.7,-1.2));
#33196=CARTESIAN_POINT('',(7.6,2.7,-1.2));
#33197=CARTESIAN_POINT('',(6.,2.3,29.8));
#33198=CARTESIAN_POINT('',(4.4,1.7,29.8));
#33199=CARTESIAN_POINT('',(7.6,1.7,29.8));
#33200=CARTESIAN_POINT('',(7.2,-1.05,29.8));
#33201=CARTESIAN_POINT('',(5.,5.5,31.5));
#33202=CARTESIAN_POINT('',(7.,5.5,31.5));
#33203=CARTESIAN_POINT('',(0.,5.,3.));
#33204=CARTESIAN_POINT('',(-2.5,2.5,-1.2));
#33205=CARTESIAN_POINT('',(-2.5,7.5,-1.2));
#33206=CARTESIAN_POINT('',(2.5,2.5,-1.2));
#33207=CARTESIAN_POINT('',(2.5,7.5,-1.2));
#33208=CARTESIAN_POINT('',(0.,5.,24.));
#33209=CARTESIAN_POINT('',(-7.5,9.5,24.));
#33210=CARTESIAN_POINT('',(-7.5,10.5,24.));
#33211=CARTESIAN_POINT('',(7.5,9.5,24.));
#33212=CARTESIAN_POINT('',(7.5,10.5,24.));
#33213=CARTESIAN_POINT('',(2.1,5.,1.6));
#33214=CARTESIAN_POINT('',(-1.05,6.81865334794732,1.6));
#33215=CARTESIAN_POINT('',(-1.05,3.18134665205268,1.6));
#33216=CARTESIAN_POINT('',(2.6,5.,25.4));
#33217=CARTESIAN_POINT('',(-1.3,7.25166604983954,25.4));
#33218=CARTESIAN_POINT('',(-1.3,2.74833395016046,25.4));
#33219=CARTESIAN_POINT('',(-6.,5.,-1.2));
#33220=CARTESIAN_POINT('',(-6.,5.,25.));
#33221=CARTESIAN_POINT('',(6.,5.,-1.2));
#33222=CARTESIAN_POINT('',(6.,5.,25.));
#33223=CARTESIAN_POINT('',(2.5,-1.5,0.4));
#33224=CARTESIAN_POINT('',(0.,1.,0.4));
#33225=CARTESIAN_POINT('',(-2.5,-1.5,0.4));
#33226=CARTESIAN_POINT('',(-4.44089209850063E-16,-4.,0.4));
#33227=CARTESIAN_POINT('',(10.,0.,0.));
#33228=CARTESIAN_POINT('',(10.,0.,-1.2));
#33229=CARTESIAN_POINT('',(9.58,0.,3.));
#33230=CARTESIAN_POINT('',(8.7,0.,3.));
#33231=CARTESIAN_POINT('',(9.58,0.,28.));
#33232=CARTESIAN_POINT('',(8.7,0.,28.));
#33233=CARTESIAN_POINT('',(0.,0.,0.));
#33234=CARTESIAN_POINT('',(0.,0.,0.));
#33235=CARTESIAN_POINT('',(0.,0.,0.));
#33236=CARTESIAN_POINT('',(0.,0.,0.));
#33237=CARTESIAN_POINT('',(0.,0.,0.));
#33238=CARTESIAN_POINT('',(0.,0.,0.));
#33239=CARTESIAN_POINT('',(-6.,0.,13.6));
#33240=CARTESIAN_POINT('',(-4.86862915010153,1.13137084989848,16.3));
#33241=CARTESIAN_POINT('',(-7.13137084989848,1.13137084989848,16.3));
#33242=CARTESIAN_POINT('',(-7.13137084989848,-1.13137084989848,16.3));
#33243=CARTESIAN_POINT('',(-4.86862915010152,-1.13137084989848,16.3));
#33244=CARTESIAN_POINT('',(6.,0.,13.6));
#33245=CARTESIAN_POINT('',(7.13137084989848,1.13137084989848,16.3));
#33246=CARTESIAN_POINT('',(4.86862915010152,1.13137084989848,16.3));
#33247=CARTESIAN_POINT('',(4.86862915010152,-1.13137084989848,16.3));
#33248=CARTESIAN_POINT('',(7.13137084989847,-1.13137084989848,16.3));
#33249=CARTESIAN_POINT('',(4.,5.,0.));
#33250=CARTESIAN_POINT('',(0.,3.5,16.3));
#33251=CARTESIAN_POINT('',(0.,6.5,16.3));
#33252=CARTESIAN_POINT('',(-1.5,5.,16.3));
#33253=CARTESIAN_POINT('',(-2.,-1.5,16.3));
#33254=CARTESIAN_POINT('',(2.,-1.5,16.3));
#33255=CARTESIAN_POINT('',(7.2,-0.35,16.7));
#33256=CARTESIAN_POINT('',(7.2,0.35,16.7));
#33257=CARTESIAN_POINT('',(0.,0.,0.));
#33258=CARTESIAN_POINT('',(0.,0.,0.));
#33259=CARTESIAN_POINT('Origin',(4.,0.,4.));
#33260=CARTESIAN_POINT('',(4.12884541125756,8.40637486662632E-6,4.59405635738975));
#33261=CARTESIAN_POINT('',(4.02115458874249,-9.26662433349265E-6,4.59413599269206));
#33262=CARTESIAN_POINT('',(4.,-7.27562663373442E-17,4.5941));
#33263=CARTESIAN_POINT('',(4.,0.254721014554615,3.46322028700965));
#33264=CARTESIAN_POINT('Ctrl Pts',(4.12884541125756,8.40637486662632E-6,
4.59405635738975));
#33265=CARTESIAN_POINT('Ctrl Pts',(4.12564700130467,0.0398130654959074,
4.59407663624518));
#33266=CARTESIAN_POINT('Ctrl Pts',(4.12244859135178,0.079613792300143,4.59013569217808));
#33267=CARTESIAN_POINT('Ctrl Pts',(4.11925018139889,0.118599576779877,4.58219388355888));
#33268=CARTESIAN_POINT('Ctrl Pts',(4.11129754205509,0.215535206692688,4.56244709042845));
#33269=CARTESIAN_POINT('Ctrl Pts',(4.10334490271129,0.30743256945264,4.51796551073728));
#33270=CARTESIAN_POINT('Ctrl Pts',(4.09539226336748,0.383054411795556,4.45418672179759));
#33271=CARTESIAN_POINT('Ctrl Pts',(4.08743962402367,0.458676254138472,4.3904079328579));
#33272=CARTESIAN_POINT('Ctrl Pts',(4.07948698467986,0.518022576064352,4.30733193466969));
#33273=CARTESIAN_POINT('Ctrl Pts',(4.07153434533606,0.553840407547632,4.21511760274296));
#33274=CARTESIAN_POINT('Ctrl Pts',(4.06358170599225,0.589658239030912,4.12290327081622));
#33275=CARTESIAN_POINT('Ctrl Pts',(4.05562906664845,0.601947580071592,4.02155060515096));
#33276=CARTESIAN_POINT('Ctrl Pts',(4.04767642730464,0.589200356533535,3.92344812692479));
#33277=CARTESIAN_POINT('Ctrl Pts',(4.03972378796084,0.576453132995478,3.82534564869861));
#33278=CARTESIAN_POINT('Ctrl Pts',(4.03177114861703,0.538669344878685,3.73049335791153));
#33279=CARTESIAN_POINT('Ctrl Pts',(4.02381850927322,0.480479105222089,3.65049437695417));
#33280=CARTESIAN_POINT('Ctrl Pts',(4.01587900618215,0.422384984811151,3.57062753914914));
#33281=CARTESIAN_POINT('Ctrl Pts',(4.00793950309107,0.343951772361455,3.50556498199611));
#33282=CARTESIAN_POINT('Ctrl Pts',(4.,0.254721014554615,3.46322028700965));
#33283=CARTESIAN_POINT('',(4.,0.254694598474614,4.53673594206822));
#33284=CARTESIAN_POINT('Origin',(4.,0.,4.));
#33285=CARTESIAN_POINT('Ctrl Pts',(3.99999999999998,0.254694598474614,4.53673594206822));
#33286=CARTESIAN_POINT('Ctrl Pts',(4.00705152958082,0.175425736340139,4.5743509952638));
#33287=CARTESIAN_POINT('Ctrl Pts',(4.01410305916165,0.0876996967667308,
4.59405101338575));
#33288=CARTESIAN_POINT('Ctrl Pts',(4.02115458874249,-9.26662433349265E-6,
4.59413599269206));
#33289=CARTESIAN_POINT('Origin',(4.,0.,4.));
#33290=CARTESIAN_POINT('',(4.42884541125756,-2.46302091461148E-6,4.59415045696459));
#33291=CARTESIAN_POINT('',(4.32115458874249,3.58587963140688E-6,4.59404994535016));
#33292=CARTESIAN_POINT('',(4.,-7.27562663373442E-17,4.5941));
#33293=CARTESIAN_POINT('Ctrl Pts',(4.42884541125756,-2.46302091461148E-6,
4.59415045696459));
#33294=CARTESIAN_POINT('Ctrl Pts',(4.42107867343035,0.0966117732708647,
4.59412799973471));
#33295=CARTESIAN_POINT('Ctrl Pts',(4.41331193560314,0.193236775309615,4.57009608476161));
#33296=CARTESIAN_POINT('Ctrl Pts',(4.40554519777592,0.278573173318151,4.52479781884576));
#33297=CARTESIAN_POINT('Ctrl Pts',(4.39759255843212,0.36595214906825,4.47841531183407));
#33298=CARTESIAN_POINT('Ctrl Pts',(4.38963991908831,0.441495654419193,4.40973622444741));
#33299=CARTESIAN_POINT('Ctrl Pts',(4.3816872797445,0.495967466205845,4.32715751007026));
#33300=CARTESIAN_POINT('Ctrl Pts',(4.3737346404007,0.550439277992498,4.24457879569311));
#33301=CARTESIAN_POINT('Ctrl Pts',(4.36578200105689,0.58383939621486,4.14810045432546));
#33302=CARTESIAN_POINT('Ctrl Pts',(4.35782936171309,0.59208420294366,4.04951827803692));
#33303=CARTESIAN_POINT('Ctrl Pts',(4.34987672236928,0.600329009672459,3.95093610174838));
#33304=CARTESIAN_POINT('Ctrl Pts',(4.34192408302547,0.583418504907695,3.85025009053894));
#33305=CARTESIAN_POINT('Ctrl Pts',(4.33397144368167,0.54342022548472,3.75977047903001));
#33306=CARTESIAN_POINT('Ctrl Pts',(4.32601880433786,0.503421946061746,3.66929086752108));
#33307=CARTESIAN_POINT('Ctrl Pts',(4.31806616499406,0.440335891980562,3.58901765571266));
#33308=CARTESIAN_POINT('Ctrl Pts',(4.31011352565025,0.361875197644003,3.52876534000234));
#33309=CARTESIAN_POINT('Ctrl Pts',(4.30216088630644,0.283414503307443,3.46851302429202));
#33310=CARTESIAN_POINT('Ctrl Pts',(4.29420824696263,0.189579168715509,3.4282816046798));
#33311=CARTESIAN_POINT('Ctrl Pts',(4.28625560761883,0.0918418319479975,
3.41298991457491));
#33312=CARTESIAN_POINT('Ctrl Pts',(4.27830296827502,-0.00589550481951406,
3.39769822447003));
#33313=CARTESIAN_POINT('Ctrl Pts',(4.27035032893122,-0.107534843762603,
3.4073462638725));
#33314=CARTESIAN_POINT('Ctrl Pts',(4.26239768958741,-0.200649373295791,
3.44075443909651));
#33315=CARTESIAN_POINT('Ctrl Pts',(4.25444505024361,-0.293763902828979,
3.47416261432052));
#33316=CARTESIAN_POINT('Ctrl Pts',(4.24649241089979,-0.378353622952266,
3.53133092536608));
#33317=CARTESIAN_POINT('Ctrl Pts',(4.23853977155599,-0.444076322467606,
3.60526974769923));
#33318=CARTESIAN_POINT('Ctrl Pts',(4.23058713221218,-0.509799021982947,
3.67920857003239));
#33319=CARTESIAN_POINT('Ctrl Pts',(4.22263449286838,-0.556654700890342,
3.76991790365313));
#33320=CARTESIAN_POINT('Ctrl Pts',(4.21468185352458,-0.578914549750806,
3.86630733464992));
#33321=CARTESIAN_POINT('Ctrl Pts',(4.20672921418077,-0.601174398611269,
3.96269676564671));
#33322=CARTESIAN_POINT('Ctrl Pts',(4.19877657483696,-0.598838417424802,
4.06476629401955));
#33323=CARTESIAN_POINT('Ctrl Pts',(4.19082393549315,-0.5721923335546,4.16003645884502));
#33324=CARTESIAN_POINT('Ctrl Pts',(4.18287129614934,-0.545546249684398,
4.25530662367048));
#33325=CARTESIAN_POINT('Ctrl Pts',(4.17491865680554,-0.494590063130461,
4.34377742494856));
#33326=CARTESIAN_POINT('Ctrl Pts',(4.16696601746173,-0.425553631634784,
4.41463223618795));
#33327=CARTESIAN_POINT('Ctrl Pts',(4.15901337811793,-0.356517200139107,
4.48548704742733));
#33328=CARTESIAN_POINT('Ctrl Pts',(4.15106073877413,-0.269400523701689,
4.53872586862801));
#33329=CARTESIAN_POINT('Ctrl Pts',(4.14310809943032,-0.174855236950146,
4.56783927594351));
#33330=CARTESIAN_POINT('Ctrl Pts',(4.1383538700394,-0.118334381217266,4.5852437891806));
#33331=CARTESIAN_POINT('Ctrl Pts',(4.13359964064848,-0.0591586432141876,
4.59402621418361));
#33332=CARTESIAN_POINT('Ctrl Pts',(4.12884541125756,8.40637486662632E-6,
4.59405635738975));
#33333=CARTESIAN_POINT('Ctrl Pts',(4.02115458874249,-9.26662433349265E-6,
4.59413599269206));
#33334=CARTESIAN_POINT('Ctrl Pts',(4.02205569850546,-0.0112175303500608,
4.59414685213492));
#33335=CARTESIAN_POINT('Ctrl Pts',(4.02295680826843,-0.0224255152200988,
4.5938373961197));
#33336=CARTESIAN_POINT('Ctrl Pts',(4.0238579180314,-0.0336155370699344,
4.59320407706013));
#33337=CARTESIAN_POINT('Ctrl Pts',(4.03181055737521,-0.132371772633995,
4.58761479340425));
#33338=CARTESIAN_POINT('Ctrl Pts',(4.03976319671902,-0.229728915328813,
4.55680066053817));
#33339=CARTESIAN_POINT('Ctrl Pts',(4.04771583606282,-0.31374319278985,4.50455967689729));
#33340=CARTESIAN_POINT('Ctrl Pts',(4.05566847540663,-0.397757470250888,
4.4523186932564));
#33341=CARTESIAN_POINT('Ctrl Pts',(4.06362111475043,-0.468428882478145,
4.37865085884071));
#33342=CARTESIAN_POINT('Ctrl Pts',(4.07157375409424,-0.517135915630147,
4.29254879227412));
#33343=CARTESIAN_POINT('Ctrl Pts',(4.07952639343804,-0.565842948782149,
4.20644672570752));
#33344=CARTESIAN_POINT('Ctrl Pts',(4.08747903278185,-0.592585602858896,
4.10791042699003));
#33345=CARTESIAN_POINT('Ctrl Pts',(4.09543167212566,-0.594084460855775,
4.00899459728238));
#33346=CARTESIAN_POINT('Ctrl Pts',(4.10338431146947,-0.595583318852653,
3.91007876757474));
#33347=CARTESIAN_POINT('Ctrl Pts',(4.11133695081327,-0.571838380769662,
3.81078340687695));
#33348=CARTESIAN_POINT('Ctrl Pts',(4.11928959015708,-0.525757920758293,
3.72324489380985));
#33349=CARTESIAN_POINT('Ctrl Pts',(4.12724222950088,-0.479677460746923,
3.63570638074275));
#33350=CARTESIAN_POINT('Ctrl Pts',(4.13519486884469,-0.411261478807175,
3.55992471530633));
#33351=CARTESIAN_POINT('Ctrl Pts',(4.1431475081885,-0.328872047298013,3.50516726345229));
#33352=CARTESIAN_POINT('Ctrl Pts',(4.1511001475323,-0.246482615788851,3.45040981159825));
#33353=CARTESIAN_POINT('Ctrl Pts',(4.15905278687611,-0.150119734710276,
3.41667657332659));
#33354=CARTESIAN_POINT('Ctrl Pts',(4.16700542621992,-0.0515665150750243,
3.40809082437526));
#33355=CARTESIAN_POINT('Ctrl Pts',(4.17495806556372,0.0469867045602276,
3.39950507542393));
#33356=CARTESIAN_POINT('Ctrl Pts',(4.18291070490753,0.147730262752155,3.41606681579293));
#33357=CARTESIAN_POINT('Ctrl Pts',(4.19086334425134,0.238347648045887,3.45575171487277));
#33358=CARTESIAN_POINT('Ctrl Pts',(4.19881598359514,0.32896503333962,3.49543661395261));
#33359=CARTESIAN_POINT('Ctrl Pts',(4.20676862293895,0.409456245735157,3.55824467174328));
#33360=CARTESIAN_POINT('Ctrl Pts',(4.21472126228276,0.469979735422806,3.63649644709345));
#33361=CARTESIAN_POINT('Ctrl Pts',(4.22267390162656,0.530503225110456,3.71474822244363));
#33362=CARTESIAN_POINT('Ctrl Pts',(4.23062654097037,0.571058992090217,3.80844371535332));
#33363=CARTESIAN_POINT('Ctrl Pts',(4.23857918031417,0.586688754827568,3.90612753493601));
#33364=CARTESIAN_POINT('Ctrl Pts',(4.24653181965798,0.602318517564919,4.0038113545187));
#33365=CARTESIAN_POINT('Ctrl Pts',(4.25448445900178,0.593022276059861,4.10548350077438));
#33366=CARTESIAN_POINT('Ctrl Pts',(4.26243709834559,0.559936509464549,4.19871308474845));
#33367=CARTESIAN_POINT('Ctrl Pts',(4.2703897376894,0.526850742869238,4.29194266872251));
#33368=CARTESIAN_POINT('Ctrl Pts',(4.27834237703321,0.469975451183674,4.37672969041494));
#33369=CARTESIAN_POINT('Ctrl Pts',(4.28629501637701,0.396264473279151,4.44270782630825));
#33370=CARTESIAN_POINT('Ctrl Pts',(4.29424765572082,0.322553495374627,4.50868596220156));
#33371=CARTESIAN_POINT('Ctrl Pts',(4.30220029506462,0.232006831251144,4.55585521229574));
#33372=CARTESIAN_POINT('Ctrl Pts',(4.31015293440843,0.135695012128791,4.57844846968215));
#33373=CARTESIAN_POINT('Ctrl Pts',(4.31382015251978,0.0912825306677821,
4.58886694826517));
#33374=CARTESIAN_POINT('Ctrl Pts',(4.31748737063114,0.0456441298716245,
4.59405951624442));
#33375=CARTESIAN_POINT('Ctrl Pts',(4.32115458874249,3.58587963140688E-6,
4.59404994535016));
#33376=CARTESIAN_POINT('Origin',(4.,0.,4.));
#33377=CARTESIAN_POINT('',(4.72884541125756,-4.67700812217808E-6,4.59405084457266));
#33378=CARTESIAN_POINT('',(4.62115458874249,3.7232086238465E-6,4.59414939806979));
#33379=CARTESIAN_POINT('',(4.,-7.27562663373442E-17,4.5941));
#33380=CARTESIAN_POINT('Ctrl Pts',(4.72884541125756,-4.67700812217808E-6,
4.59405084457266));
#33381=CARTESIAN_POINT('Ctrl Pts',(4.72446298489983,0.0545367878429411,
4.59403588702548));
#33382=CARTESIAN_POINT('Ctrl Pts',(4.7200805585421,0.10908225468116,4.58659074407712));
#33383=CARTESIAN_POINT('Ctrl Pts',(4.71569813218437,0.16154350694756,4.57176871113812));
#33384=CARTESIAN_POINT('Ctrl Pts',(4.70774549284056,0.256743148594298,4.54487167450041));
#33385=CARTESIAN_POINT('Ctrl Pts',(4.69979285349676,0.345079446524661,4.4936824501733));
#33386=CARTESIAN_POINT('Ctrl Pts',(4.69184021415295,0.415752085200636,4.42445961801412));
#33387=CARTESIAN_POINT('Ctrl Pts',(4.68388757480915,0.486424723876611,4.35523678585494));
#33388=CARTESIAN_POINT('Ctrl Pts',(4.67593493546534,0.539433703298198,4.26798034586369));
#33389=CARTESIAN_POINT('Ctrl Pts',(4.66798229612153,0.568297953762936,4.17335858623793));
#33390=CARTESIAN_POINT('Ctrl Pts',(4.66002965677773,0.597162204227674,4.07873682661218));
#33391=CARTESIAN_POINT('Ctrl Pts',(4.65207701743392,0.601881725735563,3.97674974735193));
#33392=CARTESIAN_POINT('Ctrl Pts',(4.64412437809011,0.581879492504365,3.87986665793328));
#33393=CARTESIAN_POINT('Ctrl Pts',(4.63617173874631,0.561877259273167,3.78298356851463));
#33394=CARTESIAN_POINT('Ctrl Pts',(4.6282190994025,0.517153271302883,3.69120446893757));
#33395=CARTESIAN_POINT('Ctrl Pts',(4.6202664600587,0.453175645250056,3.61575060413089));
#33396=CARTESIAN_POINT('Ctrl Pts',(4.61231382071489,0.389198019197228,3.5402967393242));
#33397=CARTESIAN_POINT('Ctrl Pts',(4.60436118137108,0.305966755061857,3.48116810928789));
#33398=CARTESIAN_POINT('Ctrl Pts',(4.59640854202727,0.213658008474022,3.4455939943611));
#33399=CARTESIAN_POINT('Ctrl Pts',(4.58845590268347,0.121349261886187,3.41001987943431));
#33400=CARTESIAN_POINT('Ctrl Pts',(4.58050326333966,0.0199630328458878,
3.39800027961704));
#33401=CARTESIAN_POINT('Ctrl Pts',(4.57255062399586,-0.0781048312986516,
3.41100475468789));
#33402=CARTESIAN_POINT('Ctrl Pts',(4.56459798465205,-0.17617269544319,3.42400922975875));
#33403=CARTESIAN_POINT('Ctrl Pts',(4.55664534530825,-0.270922194691968,
3.46203777971774));
#33404=CARTESIAN_POINT('Ctrl Pts',(4.54869270596444,-0.350768912290741,
3.52044089639904));
#33405=CARTESIAN_POINT('Ctrl Pts',(4.54074006662063,-0.430615629889515,
3.57884401308035));
#33406=CARTESIAN_POINT('Ctrl Pts',(4.53278742727683,-0.495559565838284,
3.65762169648397));
#33407=CARTESIAN_POINT('Ctrl Pts',(4.52483478793302,-0.537660439465301,
3.74714230187364));
#33408=CARTESIAN_POINT('Ctrl Pts',(4.51688214858921,-0.579761313092318,
3.8366629072633));
#33409=CARTESIAN_POINT('Ctrl Pts',(4.50892950924541,-0.599019124397585,
3.936926434639));
#33410=CARTESIAN_POINT('Ctrl Pts',(4.5009768699016,-0.593079343631488,4.03567430223551));
#33411=CARTESIAN_POINT('Ctrl Pts',(4.49302423055779,-0.587139562865391,
4.13442216983203));
#33412=CARTESIAN_POINT('Ctrl Pts',(4.48507159121399,-0.556002190027932,
4.23165437764937));
#33413=CARTESIAN_POINT('Ctrl Pts',(4.47711895187018,-0.503474193090318,
4.31548296397124));
#33414=CARTESIAN_POINT('Ctrl Pts',(4.46916631252638,-0.450946196152703,
4.39931155029312));
#33415=CARTESIAN_POINT('Ctrl Pts',(4.46121367318257,-0.377027575114933,
4.46973651511953));
#33416=CARTESIAN_POINT('Ctrl Pts',(4.45326103383876,-0.290755888038263,
4.51814744739689));
#33417=CARTESIAN_POINT('Ctrl Pts',(4.44530839449495,-0.204484200961595,
4.56655837967425));
#33418=CARTESIAN_POINT('Ctrl Pts',(4.43735575515115,-0.105859447846027,
4.59295527940255));
#33419=CARTESIAN_POINT('Ctrl Pts',(4.42940311580734,-0.00693984821361558,
4.59411076594835));
#33420=CARTESIAN_POINT('Ctrl Pts',(4.42921721429075,-0.0046274959494805,
4.59413777669183));
#33421=CARTESIAN_POINT('Ctrl Pts',(4.42903131277416,-0.00231498256911503,
4.59415099449182));
#33422=CARTESIAN_POINT('Ctrl Pts',(4.42884541125756,-2.46302091461148E-6,
4.59415045696459));
#33423=CARTESIAN_POINT('Ctrl Pts',(4.32115458874249,3.58587963140688E-6,
4.59404994535016));
#33424=CARTESIAN_POINT('Ctrl Pts',(4.32544000997495,-0.0533308355660028,
4.59403876103764));
#33425=CARTESIAN_POINT('Ctrl Pts',(4.3297254312074,-0.106668183692779,4.58692369872924));
#33426=CARTESIAN_POINT('Ctrl Pts',(4.33401085243985,-0.158055593105036,
4.57274269264177));
#33427=CARTESIAN_POINT('Ctrl Pts',(4.34196349178366,-0.253417405095285,
4.54642639353635));
#33428=CARTESIAN_POINT('Ctrl Pts',(4.34991613112746,-0.342064054954561,
4.49577653064689));
#33429=CARTESIAN_POINT('Ctrl Pts',(4.35786877047127,-0.413157291282808,
4.42698573291487));
#33430=CARTESIAN_POINT('Ctrl Pts',(4.36582140981507,-0.484250527611055,
4.35819493518285));
#33431=CARTESIAN_POINT('Ctrl Pts',(4.37377404915888,-0.537790350408272,
4.27126320260829));
#33432=CARTESIAN_POINT('Ctrl Pts',(4.38172668850269,-0.567230782432438,
4.17681912699824));
#33433=CARTESIAN_POINT('Ctrl Pts',(4.3896793278465,-0.596671214456604,4.0823750513882));
#33434=CARTESIAN_POINT('Ctrl Pts',(4.3976319671903,-0.602012255707717,3.98041863274268));
#33435=CARTESIAN_POINT('Ctrl Pts',(4.40558460653411,-0.582600893642323,
3.88341542999892));
#33436=CARTESIAN_POINT('Ctrl Pts',(4.41353724587791,-0.563189531576929,
3.78641222725516));
#33437=CARTESIAN_POINT('Ctrl Pts',(4.42148988522172,-0.519025766195027,
3.69436224041317));
#33438=CARTESIAN_POINT('Ctrl Pts',(4.42944252456553,-0.455509217992651,
3.61851983504546));
#33439=CARTESIAN_POINT('Ctrl Pts',(4.43739516390933,-0.391992669790276,
3.54267742967776));
#33440=CARTESIAN_POINT('Ctrl Pts',(4.44534780325314,-0.309123338767427,
3.48304260578434));
#33441=CARTESIAN_POINT('Ctrl Pts',(4.45330044259694,-0.217033129998519,
3.44690653227429));
#33442=CARTESIAN_POINT('Ctrl Pts',(4.46125308194075,-0.12494292122961,3.41077045876423));
#33443=CARTESIAN_POINT('Ctrl Pts',(4.46920572128456,-0.0236318347146405,
3.39813313563753));
#33444=CARTESIAN_POINT('Ctrl Pts',(4.47715836062837,0.074513469760962,3.41053964803971));
#33445=CARTESIAN_POINT('Ctrl Pts',(4.48511099997217,0.172658774236564,3.42294616044189));
#33446=CARTESIAN_POINT('Ctrl Pts',(4.49306363931598,0.2676382966728,3.46039650837296));
#33447=CARTESIAN_POINT('Ctrl Pts',(4.50101627865978,0.34783949666059,3.51831187658845));
#33448=CARTESIAN_POINT('Ctrl Pts',(4.50896891800359,0.428040696648381,3.57622724480394));
#33449=CARTESIAN_POINT('Ctrl Pts',(4.51692155734739,0.493463574187728,3.65460763330386));
#33450=CARTESIAN_POINT('Ctrl Pts',(4.5248741966912,0.536109291561612,3.74386997215216));
#33451=CARTESIAN_POINT('Ctrl Pts',(4.53282683603501,0.578755008935497,3.83313231100046));
#33452=CARTESIAN_POINT('Ctrl Pts',(4.54077947537881,0.598623566143919,3.93327660019715));
#33453=CARTESIAN_POINT('Ctrl Pts',(4.54873211472262,0.593285761408823,4.03205883640902));
#33454=CARTESIAN_POINT('Ctrl Pts',(4.55668475406643,0.587947956673727,4.1308410726209));
#33455=CARTESIAN_POINT('Ctrl Pts',(4.56463739341024,0.557403789995114,4.22826125584796));
#33456=CARTESIAN_POINT('Ctrl Pts',(4.57259003275404,0.505387701781775,4.31240844187621));
#33457=CARTESIAN_POINT('Ctrl Pts',(4.58054267209785,0.453371613568435,4.39655562790445));
#33458=CARTESIAN_POINT('Ctrl Pts',(4.58849531144165,0.37988360382037,4.46742981673387));
#33459=CARTESIAN_POINT('Ctrl Pts',(4.59644795078546,0.293908582600447,4.51636567348148));
#33460=CARTESIAN_POINT('Ctrl Pts',(4.60440059012926,0.207933561380525,4.56530153022909));
#33461=CARTESIAN_POINT('Ctrl Pts',(4.61235322947307,0.109471528688745,4.59229905489488));
#33462=CARTESIAN_POINT('Ctrl Pts',(4.62030586881688,0.01056080905581,4.59405743239568));
#33463=CARTESIAN_POINT('Ctrl Pts',(4.62058877545875,0.00704216595801619,
4.59411998479525));
#33464=CARTESIAN_POINT('Ctrl Pts',(4.62087168210062,0.00352295504485493,
4.59415059693914));
#33465=CARTESIAN_POINT('Ctrl Pts',(4.62115458874249,3.7232086238465E-6,
4.59414939806979));
#33466=CARTESIAN_POINT('Origin',(4.,0.,4.));
#33467=CARTESIAN_POINT('',(5.02884541125756,1.1583539301252E-5,4.59413174414479));
#33468=CARTESIAN_POINT('',(4.92115458874249,-9.52916733652962E-6,4.59405847898621));
#33469=CARTESIAN_POINT('',(4.,-7.27562663373442E-17,4.5941));
#33470=CARTESIAN_POINT('Ctrl Pts',(5.02884541125756,1.1583539301252E-5,
4.59413174414479));
#33471=CARTESIAN_POINT('Ctrl Pts',(5.02784729636931,0.0124287555737821,
4.59414271605904));
#33472=CARTESIAN_POINT('Ctrl Pts',(5.02684918148107,0.024845254523583,4.59376142828251));
#33473=CARTESIAN_POINT('Ctrl Pts',(5.02585106659282,0.0372368329321061,
4.59298328977014));
#33474=CARTESIAN_POINT('Ctrl Pts',(5.01789842724901,0.135968707532707,4.58678334723719));
#33475=CARTESIAN_POINT('Ctrl Pts',(5.00994578790521,0.233118536601742,4.55538989360237));
#33476=CARTESIAN_POINT('Ctrl Pts',(5.0019931485614,0.316808430381418,4.50264120614281));
#33477=CARTESIAN_POINT('Ctrl Pts',(4.9940405092176,0.400498324161095,4.44989251868324));
#33478=CARTESIAN_POINT('Ctrl Pts',(4.98608786987379,0.470728282651411,4.37578859739892));
#33479=CARTESIAN_POINT('Ctrl Pts',(4.97813523052998,0.518911736914097,4.289389655942));
#33480=CARTESIAN_POINT('Ctrl Pts',(4.97018259118617,0.567095191176782,4.20299071448508));
#33481=CARTESIAN_POINT('Ctrl Pts',(4.96222995184237,0.593232141211837,4.10429675285556));
#33482=CARTESIAN_POINT('Ctrl Pts',(4.95427731249856,0.594126988899363,4.00537445204741));
#33483=CARTESIAN_POINT('Ctrl Pts',(4.94632467315476,0.595021836586889,3.90645215123927));
#33484=CARTESIAN_POINT('Ctrl Pts',(4.93837203381095,0.570674581926886,3.80730151125251));
#33485=CARTESIAN_POINT('Ctrl Pts',(4.93041939446714,0.524062008404491,3.72004504823011));
#33486=CARTESIAN_POINT('Ctrl Pts',(4.92246675512334,0.477449434882097,3.6327885852077));
#33487=CARTESIAN_POINT('Ctrl Pts',(4.91451411577953,0.408571542497308,3.55742629914966));
#33488=CARTESIAN_POINT('Ctrl Pts',(4.90656147643572,0.325849591692228,3.50317225594031));
#33489=CARTESIAN_POINT('Ctrl Pts',(4.89860883709192,0.243127640887147,3.44891821273095));
#33490=CARTESIAN_POINT('Ctrl Pts',(4.89065619774811,0.146561631661773,3.41577241237029));
#33491=CARTESIAN_POINT('Ctrl Pts',(4.88270355840431,0.0479580738465473,
3.40778738038914));
#33492=CARTESIAN_POINT('Ctrl Pts',(4.8747509190605,-0.0506454839686783,
3.39980234840799));
#33493=CARTESIAN_POINT('Ctrl Pts',(4.86679827971669,-0.151286590373755,
3.41697808480634));
#33494=CARTESIAN_POINT('Ctrl Pts',(4.85884564037289,-0.241660499406316,
3.45721462188069));
#33495=CARTESIAN_POINT('Ctrl Pts',(4.85089300102908,-0.332034408438876,
3.49745115895503));
#33496=CARTESIAN_POINT('Ctrl Pts',(4.84294036168527,-0.41214112009892,3.56074849670536));
#33497=CARTESIAN_POINT('Ctrl Pts',(4.83498772234147,-0.472186497854497,
3.63936767349926));
#33498=CARTESIAN_POINT('Ctrl Pts',(4.82703508299766,-0.532231875610076,
3.71798685029316));
#33499=CARTESIAN_POINT('Ctrl Pts',(4.81908244365386,-0.572215919461187,
3.81192786613063));
#33500=CARTESIAN_POINT('Ctrl Pts',(4.81112980431005,-0.587250035475296,
3.9097051523746));
#33501=CARTESIAN_POINT('Ctrl Pts',(4.80317716496624,-0.602284151489406,
4.00748243861856));
#33502=CARTESIAN_POINT('Ctrl Pts',(4.79522452562244,-0.592368339666514,
4.10909599526903));
#33503=CARTESIAN_POINT('Ctrl Pts',(4.78727188627863,-0.558714943052599,
4.20212218107662));
#33504=CARTESIAN_POINT('Ctrl Pts',(4.77931924693482,-0.525061546438685,
4.2951483668842));
#33505=CARTESIAN_POINT('Ctrl Pts',(4.77136660759101,-0.467670565033749,
4.37958718184891));
#33506=CARTESIAN_POINT('Ctrl Pts',(4.76341396824721,-0.393558827964045,
4.44511483080773));
#33507=CARTESIAN_POINT('Ctrl Pts',(4.7554613289034,-0.319447090894342,4.51064247976655));
#33508=CARTESIAN_POINT('Ctrl Pts',(4.7475086895596,-0.228614598159871,4.55725896271948));
#33509=CARTESIAN_POINT('Ctrl Pts',(4.73955605021579,-0.13216685911108,4.5792647797218));
#33510=CARTESIAN_POINT('Ctrl Pts',(4.73598583722972,-0.0888681559330128,
4.58914394690572));
#33511=CARTESIAN_POINT('Ctrl Pts',(4.73241562424364,-0.0444377444908,4.59406302997518));
#33512=CARTESIAN_POINT('Ctrl Pts',(4.72884541125756,-4.67700812217808E-6,
4.59405084457266));
#33513=CARTESIAN_POINT('Ctrl Pts',(4.62115458874249,3.7232086238465E-6,
4.59414939806979));
#33514=CARTESIAN_POINT('Ctrl Pts',(4.62882432144443,-0.0954043143036648,
4.59411689615543));
#33515=CARTESIAN_POINT('Ctrl Pts',(4.63649405414636,-0.190827729806029,
4.57070400848325));
#33516=CARTESIAN_POINT('Ctrl Pts',(4.6441637868483,-0.275369369969159,4.52648596729292));
#33517=CARTESIAN_POINT('Ctrl Pts',(4.65211642619211,-0.363029422787103,
4.48063689435358));
#33518=CARTESIAN_POINT('Ctrl Pts',(4.66006906553591,-0.438990121848901,
4.4124195181391));
#33519=CARTESIAN_POINT('Ctrl Pts',(4.66802170487971,-0.493964237128006,
4.33017434199545));
#33520=CARTESIAN_POINT('Ctrl Pts',(4.67597434422352,-0.548938352407109,
4.24792916585179));
#33521=CARTESIAN_POINT('Ctrl Pts',(4.68392698356733,-0.582925883903521,
4.15165618977896));
#33522=CARTESIAN_POINT('Ctrl Pts',(4.69187962291114,-0.591771392992132,
4.05312609631255));
#33523=CARTESIAN_POINT('Ctrl Pts',(4.69983226225494,-0.600616902080743,
3.95459600284613));
#33524=CARTESIAN_POINT('Ctrl Pts',(4.70778490159875,-0.584320388761555,
3.85380879198612));
#33525=CARTESIAN_POINT('Ctrl Pts',(4.71573754094256,-0.544874323741249,
3.76308707295491));
#33526=CARTESIAN_POINT('Ctrl Pts',(4.72369018028636,-0.505428258720944,
3.6723653539237));
#33527=CARTESIAN_POINT('Ctrl Pts',(4.73164281963017,-0.442832641999522,
3.59170912672127));
#33528=CARTESIAN_POINT('Ctrl Pts',(4.73959545897397,-0.364740640256699,
3.53097971363863));
#33529=CARTESIAN_POINT('Ctrl Pts',(4.74754809831778,-0.286648638513876,
3.47025030055599));
#33530=CARTESIAN_POINT('Ctrl Pts',(4.75550073766158,-0.193060251749651,
3.42944770159313));
#33531=CARTESIAN_POINT('Ctrl Pts',(4.76345337700539,-0.095417934894009,
3.41356059019365));
#33532=CARTESIAN_POINT('Ctrl Pts',(4.7714060163492,0.00222438196163176,
3.39767347879416));
#33533=CARTESIAN_POINT('Ctrl Pts',(4.77935865569301,0.10392062890869,3.40670185495805));
#33534=CARTESIAN_POINT('Ctrl Pts',(4.78731129503681,0.19723705468272,3.43954187673519));
#33535=CARTESIAN_POINT('Ctrl Pts',(4.79526393438062,0.290553480456751,3.47238189851233));
#33536=CARTESIAN_POINT('Ctrl Pts',(4.80321657372443,0.375490085057754,3.52903356590271));
#33537=CARTESIAN_POINT('Ctrl Pts',(4.81116921306823,0.441662211759978,3.60257044098769));
#33538=CARTESIAN_POINT('Ctrl Pts',(4.81912185241204,0.507834338462201,3.67610731607267));
#33539=CARTESIAN_POINT('Ctrl Pts',(4.82707449175584,0.555241987265645,3.76652939885225));
#33540=CARTESIAN_POINT('Ctrl Pts',(4.83502713109965,0.57808892742485,3.86278135818256));
#33541=CARTESIAN_POINT('Ctrl Pts',(4.84297977044346,0.600935867584054,3.95903331751286));
#33542=CARTESIAN_POINT('Ctrl Pts',(4.85093240978726,0.599222099099018,4.0611151533939));
#33543=CARTESIAN_POINT('Ctrl Pts',(4.85888504913107,0.573157153508111,4.15654597106253));
#33544=CARTESIAN_POINT('Ctrl Pts',(4.86683768847488,0.547092207917203,4.25197678873116));
#33545=CARTESIAN_POINT('Ctrl Pts',(4.87479032781868,0.496676085220424,4.34075658818739));
#33546=CARTESIAN_POINT('Ctrl Pts',(4.88274296716249,0.428072843071251,4.41203082979109));
#33547=CARTESIAN_POINT('Ctrl Pts',(4.89069560650629,0.359469600922078,4.48330507139479));
#33548=CARTESIAN_POINT('Ctrl Pts',(4.8986482458501,0.272679239320511,4.53707375514596));
#33549=CARTESIAN_POINT('Ctrl Pts',(4.90660088519391,0.178313062033339,4.56676292714126));
#33550=CARTESIAN_POINT('Ctrl Pts',(4.9114521197101,0.120748216373203,4.58487378690922));
#33551=CARTESIAN_POINT('Ctrl Pts',(4.9163033542263,0.0603642649825261,4.59402420038378));
#33552=CARTESIAN_POINT('Ctrl Pts',(4.92115458874249,-9.52916733652962E-6,
4.59405847898621));
#33553=CARTESIAN_POINT('Origin',(4.,0.,4.));
#33554=CARTESIAN_POINT('',(5.32884541125756,-1.45357002139801E-5,4.59407911932661));
#33555=CARTESIAN_POINT('',(5.22115458874249,1.46139895546772E-5,4.59411444380891));
#33556=CARTESIAN_POINT('',(4.,-7.27562663373442E-17,4.5941));
#33557=CARTESIAN_POINT('Ctrl Pts',(5.32884541125756,-1.45357002139801E-5,
4.59407911932661));
#33558=CARTESIAN_POINT('Ctrl Pts',(5.32327896849499,0.0692531541268509,
4.59401614001471));
#33559=CARTESIAN_POINT('Ctrl Pts',(5.31771252573242,0.138542285837495,4.5819075943171));
#33560=CARTESIAN_POINT('Ctrl Pts',(5.31214608296985,0.203593590158122,4.55818044906639));
#33561=CARTESIAN_POINT('Ctrl Pts',(5.30419344362604,0.296530782575621,4.5242820624512));
#33562=CARTESIAN_POINT('Ctrl Pts',(5.29624080428224,0.380818089806801,4.46666879957728));
#33563=CARTESIAN_POINT('Ctrl Pts',(5.28828816493843,0.446150240572578,4.39238466650784));
#33564=CARTESIAN_POINT('Ctrl Pts',(5.28033552559462,0.511482391338355,4.3181005334384));
#33565=CARTESIAN_POINT('Ctrl Pts',(5.27238288625081,0.557859385638729,4.22714553017344));
#33566=CARTESIAN_POINT('Ctrl Pts',(5.26443024690701,0.579611004278495,4.13064014464439));
#33567=CARTESIAN_POINT('Ctrl Pts',(5.2564776075632,0.601362622918262,4.03413475911534));
#33568=CARTESIAN_POINT('Ctrl Pts',(5.2485249682194,0.598488865897423,3.93207899132219));
#33569=CARTESIAN_POINT('Ctrl Pts',(5.24057232887559,0.571341089151559,3.8369505488493));
#33570=CARTESIAN_POINT('Ctrl Pts',(5.23261968953179,0.544193312405696,3.74182210637642));
#33571=CARTESIAN_POINT('Ctrl Pts',(5.22466705018798,0.492771515934809,3.65362098922379));
#33572=CARTESIAN_POINT('Ctrl Pts',(5.21671441084417,0.423362714708271,3.58313098523844));
#33573=CARTESIAN_POINT('Ctrl Pts',(5.20876177150037,0.353953913481732,3.51264098125308));
#33574=CARTESIAN_POINT('Ctrl Pts',(5.20080913215656,0.266558107499543,3.45986209043499));
#33575=CARTESIAN_POINT('Ctrl Pts',(5.19285649281275,0.171860624350003,3.43124725102074));
#33576=CARTESIAN_POINT('Ctrl Pts',(5.18490385346895,0.0771631412004631,
3.40263241160649));
#33577=CARTESIAN_POINT('Ctrl Pts',(5.17695121412514,-0.0248360191164267,
3.39818162359609));
#33578=CARTESIAN_POINT('Ctrl Pts',(5.16899857478133,-0.121666070051256,
3.41843905644231));
#33579=CARTESIAN_POINT('Ctrl Pts',(5.16104593543753,-0.218496120986084,
3.43869648928852));
#33580=CARTESIAN_POINT('Ctrl Pts',(5.15309329609372,-0.310157062538852,
3.48366214299137));
#33581=CARTESIAN_POINT('Ctrl Pts',(5.14514065674991,-0.385442096207774,
3.54783835396576));
#33582=CARTESIAN_POINT('Ctrl Pts',(5.13718801740611,-0.460727129876697,
3.61201456494015));
#33583=CARTESIAN_POINT('Ctrl Pts',(5.1292353780623,-0.519636255661773,3.6954013331861));
#33584=CARTESIAN_POINT('Ctrl Pts',(5.1212827387185,-0.554967030609594,3.78780349058054));
#33585=CARTESIAN_POINT('Ctrl Pts',(5.11333009937469,-0.590297805557415,
3.88020564797498));
#33586=CARTESIAN_POINT('Ctrl Pts',(5.10537746003088,-0.60205022966798,3.98162319451792));
#33587=CARTESIAN_POINT('Ctrl Pts',(5.09742482068708,-0.588787409028971,
4.07965645386523));
#33588=CARTESIAN_POINT('Ctrl Pts',(5.08947218134327,-0.575524588389962,
4.17768971321255));
#33589=CARTESIAN_POINT('Ctrl Pts',(5.08151954199946,-0.537246523001379,
4.27233868536424));
#33590=CARTESIAN_POINT('Ctrl Pts',(5.07356690265566,-0.47863322769376,4.35203124438164));
#33591=CARTESIAN_POINT('Ctrl Pts',(5.06561426331185,-0.42001993238614,4.43172380339905));
#33592=CARTESIAN_POINT('Ctrl Pts',(5.05766162396805,-0.341071407159484,
4.49645994928216));
#33593=CARTESIAN_POINT('Ctrl Pts',(5.04970898462424,-0.251440184480074,
4.53832480650817));
#33594=CARTESIAN_POINT('Ctrl Pts',(5.04275446016868,-0.1730583412759,4.5749353153996));
#33595=CARTESIAN_POINT('Ctrl Pts',(5.03579993571312,-0.0865070403179845,
4.59405529558476));
#33596=CARTESIAN_POINT('Ctrl Pts',(5.02884541125756,1.1583539301252E-5,
4.59413174414479));
#33597=CARTESIAN_POINT('Ctrl Pts',(4.92115458874249,-9.52916733652962E-6,
4.59405847898621));
#33598=CARTESIAN_POINT('Ctrl Pts',(4.9242559935701,-0.0386066277022544,
4.59408039337166));
#33599=CARTESIAN_POINT('Ctrl Pts',(4.92735739839772,-0.0771995748988638,
4.59037647703175));
#33600=CARTESIAN_POINT('Ctrl Pts',(4.93045880322533,-0.115049119822012,
4.58290605049323));
#33601=CARTESIAN_POINT('Ctrl Pts',(4.93841144256913,-0.212103131417409,
4.56375034161047));
#33602=CARTESIAN_POINT('Ctrl Pts',(4.94636408191294,-0.304269161635426,
4.51982926360553));
#33603=CARTESIAN_POINT('Ctrl Pts',(4.95431672125675,-0.380278658005779,
4.45651276645759));
#33604=CARTESIAN_POINT('Ctrl Pts',(4.96226936060055,-0.456288154376132,
4.39319626930964));
#33605=CARTESIAN_POINT('Ctrl Pts',(4.97022199994436,-0.516141116898821,
4.31048435301868));
#33606=CARTESIAN_POINT('Ctrl Pts',(4.97817463928816,-0.552519705724467,
4.21848967586497));
#33607=CARTESIAN_POINT('Ctrl Pts',(4.98612727863197,-0.588898294550112,
4.12649499871126));
#33608=CARTESIAN_POINT('Ctrl Pts',(4.99407991797578,-0.601802509678713,
4.0252175606948));
#33609=CARTESIAN_POINT('Ctrl Pts',(5.00203255731958,-0.589654635058918,
3.92703990798411));
#33610=CARTESIAN_POINT('Ctrl Pts',(5.00998519666339,-0.577506760439122,
3.82886225527341));
#33611=CARTESIAN_POINT('Ctrl Pts',(5.0179378360072,-0.540306796070929,3.73378438786847));
#33612=CARTESIAN_POINT('Ctrl Pts',(5.025890475351,-0.482602944251693,3.65343086999412));
#33613=CARTESIAN_POINT('Ctrl Pts',(5.03384311469481,-0.424899092432456,
3.57307735211977));
#33614=CARTESIAN_POINT('Ctrl Pts',(5.04179575403862,-0.346691353162178,
3.50744818377599));
#33615=CARTESIAN_POINT('Ctrl Pts',(5.04974839338242,-0.257541687734669,
3.46456742464414));
#33616=CARTESIAN_POINT('Ctrl Pts',(5.05770103272623,-0.16839202230716,3.42168666551229));
#33617=CARTESIAN_POINT('Ctrl Pts',(5.06565367207003,-0.0683004307224215,
3.40155431559236));
#33618=CARTESIAN_POINT('Ctrl Pts',(5.07360631141384,0.0304955267282049,
3.40663182885918));
#33619=CARTESIAN_POINT('Ctrl Pts',(5.08155895075765,0.129291484178831,3.41170934212599));
#33620=CARTESIAN_POINT('Ctrl Pts',(5.08951159010146,0.226791807495345,3.44199671857955));
#33621=CARTESIAN_POINT('Ctrl Pts',(5.09746422944526,0.311075754224562,3.49379091394262));
#33622=CARTESIAN_POINT('Ctrl Pts',(5.10541686878907,0.395359700953779,3.54558510930568));
#33623=CARTESIAN_POINT('Ctrl Pts',(5.11336950813287,0.466427271095698,3.61888612357825));
#33624=CARTESIAN_POINT('Ctrl Pts',(5.12132214747668,0.515589486279599,3.70473190942573));
#33625=CARTESIAN_POINT('Ctrl Pts',(5.12927478682048,0.564751701463499,3.79057769527322));
#33626=CARTESIAN_POINT('Ctrl Pts',(5.13722742616429,0.592008561689381,3.88896825269562));
#33627=CARTESIAN_POINT('Ctrl Pts',(5.1451800655081,0.594027544563649,3.98787399599556));
#33628=CARTESIAN_POINT('Ctrl Pts',(5.1531327048519,0.596046527437917,4.0867797392955));
#33629=CARTESIAN_POINT('Ctrl Pts',(5.16108534419571,0.572827632960568,4.18620066847299));
#33630=CARTESIAN_POINT('Ctrl Pts',(5.16903798353952,0.527209687216453,4.2739812208502));
#33631=CARTESIAN_POINT('Ctrl Pts',(5.17699062288332,0.481591741472338,4.3617617732274));
#33632=CARTESIAN_POINT('Ctrl Pts',(5.18494326222713,0.413574744461461,4.43790194880433));
#33633=CARTESIAN_POINT('Ctrl Pts',(5.19289590157094,0.331474700441294,4.49309257410834));
#33634=CARTESIAN_POINT('Ctrl Pts',(5.20084854091474,0.24937465642113,4.54828319941234));
#33635=CARTESIAN_POINT('Ctrl Pts',(5.20880118025855,0.153191565391677,4.58252427444343));
#33636=CARTESIAN_POINT('Ctrl Pts',(5.21675381960235,0.0546851202186884,
4.59162936142496));
#33637=CARTESIAN_POINT('Ctrl Pts',(5.21822074264906,0.0365148790664279,
4.59330886194775));
#33638=CARTESIAN_POINT('Ctrl Pts',(5.21968766569578,0.018265586889787,4.59413312238171));
#33639=CARTESIAN_POINT('Ctrl Pts',(5.22115458874249,1.46139895546772E-5,
4.59411444380891));
#33640=CARTESIAN_POINT('Origin',(4.,0.,4.));
#33641=CARTESIAN_POINT('',(5.62884541125756,1.52328526200479E-5,4.59408648697874));
#33642=CARTESIAN_POINT('',(5.52115458874249,-1.55733839743342E-5,4.59409663347568));
#33643=CARTESIAN_POINT('',(4.,-7.27562663373442E-17,4.5941));
#33644=CARTESIAN_POINT('Ctrl Pts',(5.62884541125756,1.52328526200479E-5,
4.59408648697874));
#33645=CARTESIAN_POINT('Ctrl Pts',(5.62666327996447,0.0271682673899915,
4.59411287463303));
#33646=CARTESIAN_POINT('Ctrl Pts',(5.62448114867138,0.054317778225707,4.59228554395034));
#33647=CARTESIAN_POINT('Ctrl Pts',(5.62229901737829,0.0812075234320336,
4.58857548522516));
#33648=CARTESIAN_POINT('Ctrl Pts',(5.61434637803449,0.179205497408217,4.57505441109036));
#33649=CARTESIAN_POINT('Ctrl Pts',(5.60639373869068,0.273753285393806,4.53652709601604));
#33650=CARTESIAN_POINT('Ctrl Pts',(5.59844109934688,0.353291132582354,4.47770402899113));
#33651=CARTESIAN_POINT('Ctrl Pts',(5.59048846000307,0.432828979770902,4.41888096196622));
#33652=CARTESIAN_POINT('Ctrl Pts',(5.58253582065927,0.497356886162411,4.33976214299073));
#33653=CARTESIAN_POINT('Ctrl Pts',(5.57458318131546,0.538985436353474,4.25002092526659));
#33654=CARTESIAN_POINT('Ctrl Pts',(5.56663054197165,0.580613986544537,4.16027970754245));
#33655=CARTESIAN_POINT('Ctrl Pts',(5.55867790262784,0.599343180535155,4.05991609106967));
#33656=CARTESIAN_POINT('Ctrl Pts',(5.55072526328404,0.592883119270616,3.96120089488413));
#33657=CARTESIAN_POINT('Ctrl Pts',(5.54277262394023,0.586423058006077,3.86248569869858));
#33658=CARTESIAN_POINT('Ctrl Pts',(5.53481998459642,0.554773741486382,3.76541892280029));
#33659=CARTESIAN_POINT('Ctrl Pts',(5.52686734525262,0.501804729712613,3.68186830256729));
#33660=CARTESIAN_POINT('Ctrl Pts',(5.51891470590881,0.448835717938844,3.5983176823343));
#33661=CARTESIAN_POINT('Ctrl Pts',(5.51096206656501,0.374547010911001,3.52828321776661));
#33662=CARTESIAN_POINT('Ctrl Pts',(5.5030094272212,0.288021414854312,3.48032757600706));
#33663=CARTESIAN_POINT('Ctrl Pts',(5.4950567878774,0.201495818797622,3.4323719342475));
#33664=CARTESIAN_POINT('Ctrl Pts',(5.48710414853359,0.102733333712086,3.40649511529609));
#33665=CARTESIAN_POINT('Ctrl Pts',(5.47915150918978,0.00380901851787326,
3.40586091270526));
#33666=CARTESIAN_POINT('Ctrl Pts',(5.47119886984597,-0.0951152966763399,
3.40522671011442));
#33667=CARTESIAN_POINT('Ctrl Pts',(5.46324623050217,-0.194201441979227,
3.42983512388417));
#33668=CARTESIAN_POINT('Ctrl Pts',(5.45529359115836,-0.281334786601535,
3.47667744027106));
#33669=CARTESIAN_POINT('Ctrl Pts',(5.44734095181456,-0.368468131223842,
3.52351975665794));
#33670=CARTESIAN_POINT('Ctrl Pts',(5.43938831247075,-0.443648675165568,
3.59259597566196));
#33671=CARTESIAN_POINT('Ctrl Pts',(5.43143567312694,-0.497684572991269,
3.67546058871077));
#33672=CARTESIAN_POINT('Ctrl Pts',(5.42348303378314,-0.551720470816969,
3.75832520175959));
#33673=CARTESIAN_POINT('Ctrl Pts',(5.41553039443933,-0.584611722526643,
3.85497820885321));
#33674=CARTESIAN_POINT('Ctrl Pts',(5.40757775509553,-0.592336924628993,
3.95360246348684));
#33675=CARTESIAN_POINT('Ctrl Pts',(5.39962511575172,-0.600062126731343,
4.05222671812048));
#33676=CARTESIAN_POINT('Ctrl Pts',(5.39167247640791,-0.582621279226368,
4.15282222029412));
#33677=CARTESIAN_POINT('Ctrl Pts',(5.3837198370641,-0.542146763261091,4.24308979978386));
#33678=CARTESIAN_POINT('Ctrl Pts',(5.3757671977203,-0.501672247295815,4.3333573792736));
#33679=CARTESIAN_POINT('Ctrl Pts',(5.36781455837649,-0.438164062870237,
4.41329703607943));
#33680=CARTESIAN_POINT('Ctrl Pts',(5.35986191903269,-0.359386950494509,
4.47313505840055));
#33681=CARTESIAN_POINT('Ctrl Pts',(5.35190927968888,-0.28060983811878,4.53297308072167));
#33682=CARTESIAN_POINT('Ctrl Pts',(5.34395664034507,-0.1865637977929,4.57270946855809));
#33683=CARTESIAN_POINT('Ctrl Pts',(5.33600400100126,-0.0887472388280498,
4.58748590729807));
#33684=CARTESIAN_POINT('Ctrl Pts',(5.33361780442003,-0.0593972924141157,
4.59191959101989));
#33685=CARTESIAN_POINT('Ctrl Pts',(5.3312316078388,-0.0297078841644672,
4.59410611700271));
#33686=CARTESIAN_POINT('Ctrl Pts',(5.32884541125756,-1.45357002139801E-5,
4.59407911932661));
#33687=CARTESIAN_POINT('Ctrl Pts',(5.22115458874249,1.46139895546772E-5,
4.59411444380891));
#33688=CARTESIAN_POINT('Ctrl Pts',(5.22764030503958,-0.0806785298274998,
4.59403186011492));
#33689=CARTESIAN_POINT('Ctrl Pts',(5.23412602133668,-0.161404528346198,
4.57747154641029));
#33690=CARTESIAN_POINT('Ctrl Pts',(5.24061173763377,-0.235476461490165,
4.54549665421293));
#33691=CARTESIAN_POINT('Ctrl Pts',(5.24856437697758,-0.32630179870949,4.50628976108741));
#33692=CARTESIAN_POINT('Ctrl Pts',(5.25651701632139,-0.407122673831612,
4.44390687590439));
#33693=CARTESIAN_POINT('Ctrl Pts',(5.26446965566519,-0.468057634114636,
4.36597515601533));
#33694=CARTESIAN_POINT('Ctrl Pts',(5.272422295009,-0.52899259439766,4.28804343612627));
#33695=CARTESIAN_POINT('Ctrl Pts',(5.28037493435281,-0.570041639841584,
4.19456288153117));
#33696=CARTESIAN_POINT('Ctrl Pts',(5.28832757369661,-0.586185965564114,
4.09696276320888));
#33697=CARTESIAN_POINT('Ctrl Pts',(5.29628021304042,-0.602330291286644,
3.99936264488659));
#33698=CARTESIAN_POINT('Ctrl Pts',(5.30423285238423,-0.59356989728778,3.89764296283709));
#33699=CARTESIAN_POINT('Ctrl Pts',(5.31218549172803,-0.560975861048054,
3.80424033358521));
#33700=CARTESIAN_POINT('Ctrl Pts',(5.32013813107184,-0.528381824808328,
3.71083770433334));
#33701=CARTESIAN_POINT('Ctrl Pts',(5.32809077041564,-0.471954146327742,
3.62575212787907));
#33702=CARTESIAN_POINT('Ctrl Pts',(5.33604340975945,-0.398591877830097,
3.55938647478623));
#33703=CARTESIAN_POINT('Ctrl Pts',(5.34399604910326,-0.325229609332449,
3.49302082169338));
#33704=CARTESIAN_POINT('Ctrl Pts',(5.35194868844707,-0.234932750817741,
3.44537509196196));
#33705=CARTESIAN_POINT('Ctrl Pts',(5.35990132779087,-0.138741323057917,
3.42227462497344));
#33706=CARTESIAN_POINT('Ctrl Pts',(5.36785396713468,-0.042549895298095,
3.39917415798493));
#33707=CARTESIAN_POINT('Ctrl Pts',(5.37580660647848,0.059536101706843,3.40061895373932));
#33708=CARTESIAN_POINT('Ctrl Pts',(5.38375924582229,0.155035264439678,3.42643236627792));
#33709=CARTESIAN_POINT('Ctrl Pts',(5.39171188516609,0.250534427172515,3.45224577881651));
#33710=CARTESIAN_POINT('Ctrl Pts',(5.3996645245099,0.339446755633248,3.5024278081393));
#33711=CARTESIAN_POINT('Ctrl Pts',(5.40761716385371,0.41090150670596,3.57084301769608));
#33712=CARTESIAN_POINT('Ctrl Pts',(5.41556980319751,0.482356257778672,3.63925822725286));
#33713=CARTESIAN_POINT('Ctrl Pts',(5.42352244254132,0.536353431463363,3.72590661704362));
#33714=CARTESIAN_POINT('Ctrl Pts',(5.43147508188513,0.566291137850326,3.82019424128906));
#33715=CARTESIAN_POINT('Ctrl Pts',(5.43942772122893,0.596228844237288,3.91448186553449));
#33716=CARTESIAN_POINT('Ctrl Pts',(5.44738036057274,0.602107083326521,4.01640872423458));
#33717=CARTESIAN_POINT('Ctrl Pts',(5.45533299991655,0.583207160329387,4.11351287069736));
#33718=CARTESIAN_POINT('Ctrl Pts',(5.46328563926035,0.564307237332252,4.21061701716013));
#33719=CARTESIAN_POINT('Ctrl Pts',(5.47123827860416,0.520629152248751,4.30289845138559));
#33720=CARTESIAN_POINT('Ctrl Pts',(5.47919091794796,0.457513145863858,4.37907451119169));
#33721=CARTESIAN_POINT('Ctrl Pts',(5.48714355729177,0.394397139478966,4.45525057099779));
#33722=CARTESIAN_POINT('Ctrl Pts',(5.49509619663558,0.311843211792683,4.51532125638452));
#33723=CARTESIAN_POINT('Ctrl Pts',(5.50304883597938,0.219944704826683,4.5519421079172));
#33724=CARTESIAN_POINT('Ctrl Pts',(5.50908408690042,0.150203009669811,4.5797336395568));
#33725=CARTESIAN_POINT('Ctrl Pts',(5.51511933782146,0.0750795109720808,
4.59401975858331));
#33726=CARTESIAN_POINT('Ctrl Pts',(5.52115458874249,-1.55733839743342E-5,
4.59409663347568));
#33727=CARTESIAN_POINT('Origin',(4.,0.,4.));
#33728=CARTESIAN_POINT('',(5.92884541125757,-1.3134308860685E-5,4.59412454375027));
#33729=CARTESIAN_POINT('',(5.82115458874249,1.31105368646138E-5,4.59407040741879));
#33730=CARTESIAN_POINT('',(4.,-7.27562663373442E-17,4.5941));
#33731=CARTESIAN_POINT('Ctrl Pts',(5.92884541125757,-1.3134308860685E-5,
4.59412454375027));
#33732=CARTESIAN_POINT('Ctrl Pts',(5.92209495209015,0.0839697382976411,
4.5940436242297));
#33733=CARTESIAN_POINT('Ctrl Pts',(5.91534449292274,0.16798613900316,4.57606223573506));
#33734=CARTESIAN_POINT('Ctrl Pts',(5.90859403375532,0.244517407380453,4.54150437939301));
#33735=CARTESIAN_POINT('Ctrl Pts',(5.90064139441152,0.334678026211646,4.50079216098422));
#33736=CARTESIAN_POINT('Ctrl Pts',(5.89268875506771,0.41445008323119,4.43707358099086));
#33737=CARTESIAN_POINT('Ctrl Pts',(5.8847361157239,0.474080337065587,4.35813908232779));
#33738=CARTESIAN_POINT('Ctrl Pts',(5.8767834763801,0.533710590899983,4.27920458366471));
#33739=CARTESIAN_POINT('Ctrl Pts',(5.86883083703629,0.573199041549232,4.18505416633191));
#33740=CARTESIAN_POINT('Ctrl Pts',(5.86087819769249,0.587717699183782,4.08719901244189));
#33741=CARTESIAN_POINT('Ctrl Pts',(5.85292555834868,0.602236356818331,3.98934385855186));
#33742=CARTESIAN_POINT('Ctrl Pts',(5.84497291900487,0.591785221438181,3.88778396810461));
#33743=CARTESIAN_POINT('Ctrl Pts',(5.83702027966107,0.557642080814915,3.79493641494568));
#33744=CARTESIAN_POINT('Ctrl Pts',(5.82906764031726,0.523498940191649,3.70208886178675));
#33745=CARTESIAN_POINT('Ctrl Pts',(5.82111500097346,0.465663794325265,3.61795364591614));
#33746=CARTESIAN_POINT('Ctrl Pts',(5.81316236162965,0.391207780605707,3.55281744653948));
#33747=CARTESIAN_POINT('Ctrl Pts',(5.80520972228584,0.31675176688615,3.48768124716281));
#33748=CARTESIAN_POINT('Ctrl Pts',(5.79725708294203,0.225674885313418,3.44154406428009));
#33749=CARTESIAN_POINT('Ctrl Pts',(5.78930444359823,0.129112523455512,3.42004679519738));
#33750=CARTESIAN_POINT('Ctrl Pts',(5.78135180425442,0.0325501615976049,
3.39854952611466));
#33751=CARTESIAN_POINT('Ctrl Pts',(5.77339916491062,-0.0694976805454773,
3.40169217083197));
#33752=CARTESIAN_POINT('Ctrl Pts',(5.76544652556681,-0.164554263536051,
3.42909049911887));
#33753=CARTESIAN_POINT('Ctrl Pts',(5.75749388622301,-0.259610846526622,
3.45648882740576));
#33754=CARTESIAN_POINT('Ctrl Pts',(5.7495412468792,-0.347676170364685,3.50814283926225));
#33755=CARTESIAN_POINT('Ctrl Pts',(5.74158860753539,-0.417983050247216,
3.57773712775495));
#33756=CARTESIAN_POINT('Ctrl Pts',(5.73363596819158,-0.488289930129746,
3.64733141624764));
#33757=CARTESIAN_POINT('Ctrl Pts',(5.72568332884778,-0.540838366056745,
3.73486598137654));
#33758=CARTESIAN_POINT('Ctrl Pts',(5.71773068950397,-0.569203595796233,
3.82963853060694));
#33759=CARTESIAN_POINT('Ctrl Pts',(5.70977805016017,-0.597568825535722,
3.92441107983734));
#33760=CARTESIAN_POINT('Ctrl Pts',(5.70182541081636,-0.6017508490877,4.02642161316923));
#33761=CARTESIAN_POINT('Ctrl Pts',(5.69387277147255,-0.581238357244447,
4.12319795341528));
#33762=CARTESIAN_POINT('Ctrl Pts',(5.68592013212875,-0.560725865401195,
4.21997429366132));
#33763=CARTESIAN_POINT('Ctrl Pts',(5.67796749278494,-0.515518858162713,
4.31151644082153));
#33764=CARTESIAN_POINT('Ctrl Pts',(5.67001485344113,-0.451144507802385,
4.38663212069642));
#33765=CARTESIAN_POINT('Ctrl Pts',(5.66206221409732,-0.386770157442057,
4.46174780057131));
#33766=CARTESIAN_POINT('Ctrl Pts',(5.65410957475352,-0.303228463959881,
4.52043701316089));
#33767=CARTESIAN_POINT('Ctrl Pts',(5.64615693540972,-0.210733537235404,
4.55552420285805));
#33768=CARTESIAN_POINT('Ctrl Pts',(5.640386427359,-0.143618370026196,4.5809837895275));
#33769=CARTESIAN_POINT('Ctrl Pts',(5.63461591930828,-0.07178924788396,4.59401670649762));
#33770=CARTESIAN_POINT('Ctrl Pts',(5.62884541125756,1.52328526200479E-5,
4.59408648697874));
#33771=CARTESIAN_POINT('Ctrl Pts',(5.52115458874249,-1.55733839743342E-5,
4.59409663347568));
#33772=CARTESIAN_POINT('Ctrl Pts',(5.52307197716526,-0.0238731473664388,
4.59412105649149));
#33773=CARTESIAN_POINT('Ctrl Pts',(5.52498936558803,-0.0477278534282068,
4.59271130989713));
#33774=CARTESIAN_POINT('Ctrl Pts',(5.5269067540108,-0.0714062077139717,
4.58984482465595));
#33775=CARTESIAN_POINT('Ctrl Pts',(5.53485939335461,-0.169615527042917,
4.57795567218339));
#33776=CARTESIAN_POINT('Ctrl Pts',(5.54281203269841,-0.264791079455087,
4.54100634955965));
#33777=CARTESIAN_POINT('Ctrl Pts',(5.55076467204222,-0.345296357402727,
4.48351441471562));
#33778=CARTESIAN_POINT('Ctrl Pts',(5.55871731138603,-0.425801635350366,
4.4260224798716));
#33779=CARTESIAN_POINT('Ctrl Pts',(5.56666995072984,-0.491636638833473,
4.34798793280729));
#33780=CARTESIAN_POINT('Ctrl Pts',(5.57462259007364,-0.534752142022197,
4.2589515597096));
#33781=CARTESIAN_POINT('Ctrl Pts',(5.58257522941745,-0.577867645210921,
4.16991518661191));
#33782=CARTESIAN_POINT('Ctrl Pts',(5.59052786876125,-0.598263648105263,
4.06987698748084));
#33783=CARTESIAN_POINT('Ctrl Pts',(5.59848050810506,-0.59344646156208,3.97106799465478));
#33784=CARTESIAN_POINT('Ctrl Pts',(5.60643314744886,-0.588629275018896,
3.87225900182873));
#33785=CARTESIAN_POINT('Ctrl Pts',(5.61438578679267,-0.558598899038186,
3.77467921530768));
#33786=CARTESIAN_POINT('Ctrl Pts',(5.62233842613648,-0.50702695609161,3.69025909300064));
#33787=CARTESIAN_POINT('Ctrl Pts',(5.63029106548029,-0.455455013145033,
3.6058389706936));
#33788=CARTESIAN_POINT('Ctrl Pts',(5.63824370482409,-0.382341503232591,
3.53457851260056));
#33789=CARTESIAN_POINT('Ctrl Pts',(5.6461963441679,-0.296625548722353,3.48519028027742));
#33790=CARTESIAN_POINT('Ctrl Pts',(5.6541489835117,-0.210909594212113,3.43580204795428));
#33791=CARTESIAN_POINT('Ctrl Pts',(5.66210162285551,-0.112591195104077,
3.40828604140104));
#33792=CARTESIAN_POINT('Ctrl Pts',(5.67005426219932,-0.0136911147678568,
3.40600646716786));
#33793=CARTESIAN_POINT('Ctrl Pts',(5.67800690154312,0.0852089655683624,
3.40372689293467));
#33794=CARTESIAN_POINT('Ctrl Pts',(5.68595954088693,0.184690727132768,3.42668375102154));
#33795=CARTESIAN_POINT('Ctrl Pts',(5.69391218023074,0.272591169676606,3.47207025288287));
#33796=CARTESIAN_POINT('Ctrl Pts',(5.70186481957454,0.360491612220445,3.51745675474419));
#33797=CARTESIAN_POINT('Ctrl Pts',(5.70981745891835,0.436810735743714,3.58527290037998));
#33798=CARTESIAN_POINT('Ctrl Pts',(5.71777009826216,0.492217487918224,3.667227242308));
#33799=CARTESIAN_POINT('Ctrl Pts',(5.72572273760596,0.547624240092733,3.74918158423602));
#33800=CARTESIAN_POINT('Ctrl Pts',(5.73367537694977,0.582118620918482,3.84527412245626));
#33801=CARTESIAN_POINT('Ctrl Pts',(5.74162801629357,0.591483222595687,3.94375623549444));
#33802=CARTESIAN_POINT('Ctrl Pts',(5.74958065563738,0.600847824272892,4.04223834853263));
#33803=CARTESIAN_POINT('Ctrl Pts',(5.75753329498119,0.585082646801554,4.14311003638875));
#33804=CARTESIAN_POINT('Ctrl Pts',(5.76548593432499,0.546115197731279,4.23403836123177));
#33805=CARTESIAN_POINT('Ctrl Pts',(5.7734385736688,0.507147748661005,4.32496668607478));
#33806=CARTESIAN_POINT('Ctrl Pts',(5.78139121301261,0.444978027991796,4.4059516479047));
#33807=CARTESIAN_POINT('Ctrl Pts',(5.78934385235641,0.367207131024688,4.46709173242012));
#33808=CARTESIAN_POINT('Ctrl Pts',(5.79729649170022,0.28943623405758,4.52823181693554));
#33809=CARTESIAN_POINT('Ctrl Pts',(5.80524913104403,0.196064160792572,4.56952702413646));
#33810=CARTESIAN_POINT('Ctrl Pts',(5.81320177038783,0.0985069184831505,
4.58592845199323));
#33811=CARTESIAN_POINT('Ctrl Pts',(5.81585270983939,0.0659871057213339,
4.59139571767544));
#33812=CARTESIAN_POINT('Ctrl Pts',(5.81850364929094,0.0330022532417819,
4.59409688335147));
#33813=CARTESIAN_POINT('Ctrl Pts',(5.82115458874249,1.31105368646138E-5,
4.59407040741879));
#33814=CARTESIAN_POINT('Origin',(4.,0.,4.));
#33815=CARTESIAN_POINT('',(6.22884541125756,-1.27841859475647E-5,4.5940334609955));
#33816=CARTESIAN_POINT('',(6.12115458874249,-9.50793186244619E-6,4.59413936148612));
#33817=CARTESIAN_POINT('',(4.,-7.27562663373442E-17,4.5941));
#33818=CARTESIAN_POINT('Ctrl Pts',(6.22884541125756,-1.27841859475647E-5,
4.5940334609955));
#33819=CARTESIAN_POINT('Ctrl Pts',(6.22547926355963,0.0418951881409122,
4.59406590912705));
#33820=CARTESIAN_POINT('Ctrl Pts',(6.2221131158617,0.0838018877146867,4.58971510200585));
#33821=CARTESIAN_POINT('Ctrl Pts',(6.21874696816377,0.124749109322564,4.58093223526196));
#33822=CARTESIAN_POINT('Ctrl Pts',(6.21079432881996,0.22148832423537,4.56018241146135));
#33823=CARTESIAN_POINT('Ctrl Pts',(6.20284168947616,0.31287214740051,4.51469474440412));
#33824=CARTESIAN_POINT('Ctrl Pts',(6.19488905013236,0.387808805213989,4.4501133836823));
#33825=CARTESIAN_POINT('Ctrl Pts',(6.18693641078855,0.462745463027469,4.38553202296047));
#33826=CARTESIAN_POINT('Ctrl Pts',(6.17898377144474,0.521234955489287,4.30185696857405));
#33827=CARTESIAN_POINT('Ctrl Pts',(6.17103113210093,0.556083161424236,4.20927485003939));
#33828=CARTESIAN_POINT('Ctrl Pts',(6.16307849275713,0.590931367359184,4.11669273150472));
#33829=CARTESIAN_POINT('Ctrl Pts',(6.15512585341332,0.602138286767263,4.0152035488218));
#33830=CARTESIAN_POINT('Ctrl Pts',(6.14717321406952,0.588356486924291,3.9172389266648));
#33831=CARTESIAN_POINT('Ctrl Pts',(6.13922057472571,0.574574687081318,3.81927430450779));
#33832=CARTESIAN_POINT('Ctrl Pts',(6.1312679353819,0.535804167987293,3.7248342428767));
#33833=CARTESIAN_POINT('Ctrl Pts',(6.12331529603809,0.476773096629474,3.64545304401991));
#33834=CARTESIAN_POINT('Ctrl Pts',(6.11536265669429,0.417742025271657,3.56607184516312));
#33835=CARTESIAN_POINT('Ctrl Pts',(6.10741001735048,0.338450401650047,3.50174950908064));
#33836=CARTESIAN_POINT('Ctrl Pts',(6.09945737800668,0.248599092144812,3.46035682177302));
#33837=CARTESIAN_POINT('Ctrl Pts',(6.09150473866287,0.158747782639575,3.41896413446539));
#33838=CARTESIAN_POINT('Ctrl Pts',(6.08355209931906,0.0583367872507115,
3.40050109593262));
#33839=CARTESIAN_POINT('Ctrl Pts',(6.07559945997526,-0.0403606640336046,
3.40722161935946));
#33840=CARTESIAN_POINT('Ctrl Pts',(6.06764682063145,-0.139058115317921,
3.4139421427863));
#33841=CARTESIAN_POINT('Ctrl Pts',(6.05969418128764,-0.23604202249769,3.44584622817275));
#33842=CARTESIAN_POINT('Ctrl Pts',(6.05174154194384,-0.319452991027635,
3.49903499090221));
#33843=CARTESIAN_POINT('Ctrl Pts',(6.04378890260003,-0.40286395955758,3.55222375363166));
#33844=CARTESIAN_POINT('Ctrl Pts',(6.03583626325623,-0.472701989437702,
3.62669719370411));
#33845=CARTESIAN_POINT('Ctrl Pts',(6.02788362391242,-0.520429378860104,
3.71334895258148));
#33846=CARTESIAN_POINT('Ctrl Pts',(6.01993098456861,-0.568156768282506,
3.80000071145885));
#33847=CARTESIAN_POINT('Ctrl Pts',(6.0119783452248,-0.593773517247188,3.89883078914114));
#33848=CARTESIAN_POINT('Ctrl Pts',(6.004025705881,-0.594147126960238,3.99775637428654));
#33849=CARTESIAN_POINT('Ctrl Pts',(5.99607306653719,-0.594520736673288,
4.09668195943193));
#33850=CARTESIAN_POINT('Ctrl Pts',(5.98812042719339,-0.569651207134705,
4.19570305204043));
#33851=CARTESIAN_POINT('Ctrl Pts',(5.98016778784958,-0.52257944308796,4.28271270390554));
#33852=CARTESIAN_POINT('Ctrl Pts',(5.97221514850578,-0.475507679041215,
4.36972235577065));
#33853=CARTESIAN_POINT('Ctrl Pts',(5.96426250916196,-0.406233680486307,
4.44472056689237));
#33854=CARTESIAN_POINT('Ctrl Pts',(5.95630986981816,-0.323226996343023,
4.49853792802592));
#33855=CARTESIAN_POINT('Ctrl Pts',(5.94835723047435,-0.240220312199739,
4.55235528915947));
#33856=CARTESIAN_POINT('Ctrl Pts',(5.94040459113055,-0.143480942468078,
4.58499180030486));
#33857=CARTESIAN_POINT('Ctrl Pts',(5.93245195178675,-0.0448366672808267,
4.59245712746544));
#33858=CARTESIAN_POINT('Ctrl Pts',(5.93124977161035,-0.0299248641651563,
4.59358564190382));
#33859=CARTESIAN_POINT('Ctrl Pts',(5.93004759143396,-0.0149695309183627,
4.59413895459864));
#33860=CARTESIAN_POINT('Ctrl Pts',(5.92884541125757,-1.3134308860685E-5,
4.59412454375027));
#33861=CARTESIAN_POINT('Ctrl Pts',(5.82115458874249,1.31105368646138E-5,
4.59407040741879));
#33862=CARTESIAN_POINT('Ctrl Pts',(5.82645628863475,-0.0659629472043463,
4.59401745734129));
#33863=CARTESIAN_POINT('Ctrl Pts',(5.831757988527,-0.131956164688202,4.58305467757793));
#33864=CARTESIAN_POINT('Ctrl Pts',(5.83705968841925,-0.194280919321303,
4.56148970414564));
#33865=CARTESIAN_POINT('Ctrl Pts',(5.84501232776306,-0.287769103462499,
4.52914187992864));
#33866=CARTESIAN_POINT('Ctrl Pts',(5.85296496710686,-0.373003060391055,
4.47293858298203));
#33867=CARTESIAN_POINT('Ctrl Pts',(5.86091760645067,-0.439561779454174,
4.39975142997742));
#33868=CARTESIAN_POINT('Ctrl Pts',(5.86887024579447,-0.506120498517293,
4.32656427697281));
#33869=CARTESIAN_POINT('Ctrl Pts',(5.87682288513828,-0.554003979714975,
4.2363932679102));
#33870=CARTESIAN_POINT('Ctrl Pts',(5.88477552448209,-0.577357812582609,
4.14026304025204));
#33871=CARTESIAN_POINT('Ctrl Pts',(5.8927281638259,-0.600711645450243,4.04413281259387));
#33872=CARTESIAN_POINT('Ctrl Pts',(5.9006808031697,-0.59953582998783,3.94204336634015));
#33873=CARTESIAN_POINT('Ctrl Pts',(5.90863344251351,-0.573974130801472,
3.84647652011691));
#33874=CARTESIAN_POINT('Ctrl Pts',(5.91658608185731,-0.548412431615114,
3.75090967389367));
#33875=CARTESIAN_POINT('Ctrl Pts',(5.92453872120112,-0.498464848704808,
3.66186542770092));
#33876=CARTESIAN_POINT('Ctrl Pts',(5.93249136054493,-0.430238144626613,
3.59023066587279));
#33877=CARTESIAN_POINT('Ctrl Pts',(5.94044399988873,-0.362011440548417,
3.51859590404466));
#33878=CARTESIAN_POINT('Ctrl Pts',(5.94839663923254,-0.275505615302329,
3.46437062658116));
#33879=CARTESIAN_POINT('Ctrl Pts',(5.95634927857635,-0.181297202577209,
3.43418458862315));
#33880=CARTESIAN_POINT('Ctrl Pts',(5.96430191792015,-0.087088789852092,
3.40399855066514));
#33881=CARTESIAN_POINT('Ctrl Pts',(5.97225455726396,0.0148222103520573,
3.39785175221263));
#33882=CARTESIAN_POINT('Ctrl Pts',(5.98020719660777,0.111975824940657,3.41649576758492));
#33883=CARTESIAN_POINT('Ctrl Pts',(5.98815983595157,0.209129439529257,3.43513978295721));
#33884=CARTESIAN_POINT('Ctrl Pts',(5.99611247529537,0.301525668502307,3.47857461215431));
#33885=CARTESIAN_POINT('Ctrl Pts',(6.00406511463918,0.377867748972965,3.54148967172874));
#33886=CARTESIAN_POINT('Ctrl Pts',(6.01201775398299,0.454209829443624,3.60440473130317));
#33887=CARTESIAN_POINT('Ctrl Pts',(6.0199703933268,0.514497761411887,3.68680002125492));
#33888=CARTESIAN_POINT('Ctrl Pts',(6.02792303267061,0.551360647735685,3.77860175380959));
#33889=CARTESIAN_POINT('Ctrl Pts',(6.03587567201441,0.588223534059482,3.87040348636426));
#33890=CARTESIAN_POINT('Ctrl Pts',(6.04382831135821,0.601661374738811,3.97161166152184));
#33891=CARTESIAN_POINT('Ctrl Pts',(6.05178095070202,0.590030977261751,4.06985190192822));
#33892=CARTESIAN_POINT('Ctrl Pts',(6.05973359004583,0.578400579784692,4.16809214233459));
#33893=CARTESIAN_POINT('Ctrl Pts',(6.06768622938964,0.541701944151245,4.26336444798975));
#33894=CARTESIAN_POINT('Ctrl Pts',(6.07563886873345,0.484422419230229,4.3440210474869));
#33895=CARTESIAN_POINT('Ctrl Pts',(6.08359150807725,0.427142894309213,4.42467764698404));
#33896=CARTESIAN_POINT('Ctrl Pts',(6.09154414742105,0.349282480100627,4.49071854032316));
#33897=CARTESIAN_POINT('Ctrl Pts',(6.09949678676486,0.26035984028865,4.53406826097581));
#33898=CARTESIAN_POINT('Ctrl Pts',(6.10671605409073,0.179637418414302,4.5734203814938));
#33899=CARTESIAN_POINT('Ctrl Pts',(6.11393532141662,0.0897989573399868,
4.59407340590587));
#33900=CARTESIAN_POINT('Ctrl Pts',(6.12115458874249,-9.50793186244619E-6,
4.59413936148612));
#33901=CARTESIAN_POINT('Origin',(4.,0.,4.));
#33902=CARTESIAN_POINT('',(6.52884541125757,2.61457539729726E-5,4.59508370962656));
#33903=CARTESIAN_POINT('',(6.42115458874249,-0.000630941829811112,4.59394485456974));
#33904=CARTESIAN_POINT('',(4.,-7.27562663373442E-17,4.5941));
#33905=CARTESIAN_POINT('Ctrl Pts',(6.52884541125757,2.61457539729726E-5,
4.59508370962656));
#33906=CARTESIAN_POINT('Ctrl Pts',(6.5129582963415,0.196771080344787,4.59506033873941));
#33907=CARTESIAN_POINT('Ctrl Pts',(6.49707118142544,0.393450480974957,4.48779253427891));
#33908=CARTESIAN_POINT('Ctrl Pts',(6.48118406650938,0.500111739713094,4.32240987211318));
#33909=CARTESIAN_POINT('Ctrl Pts',(6.46527878782176,0.606894944490356,4.15683812760557));
#33910=CARTESIAN_POINT('Ctrl Pts',(6.44937350913416,0.623454053851315,3.93301856375293));
#33911=CARTESIAN_POINT('Ctrl Pts',(6.43346823044654,0.541809843535619,3.75368369989414));
#33912=CARTESIAN_POINT('Ctrl Pts',(6.41756295175893,0.460165633219924,3.57434883603535));
#33913=CARTESIAN_POINT('Ctrl Pts',(6.40165767307132,0.280318103227576,3.43949867217041));
#33914=CARTESIAN_POINT('Ctrl Pts',(6.3857523943837,0.085604811340831,3.41110814665827));
#33915=CARTESIAN_POINT('Ctrl Pts',(6.36984711569609,-0.109108480545914,
3.38271762114613));
#33916=CARTESIAN_POINT('Ctrl Pts',(6.35394183700848,-0.318687534327053,
3.46078673398678));
#33917=CARTESIAN_POINT('Ctrl Pts',(6.33803655832087,-0.448733343985475,
3.60951691634857));
#33918=CARTESIAN_POINT('Ctrl Pts',(6.33008391897706,-0.513756248814686,
3.68388200752946));
#33919=CARTESIAN_POINT('Ctrl Pts',(6.32213127963325,-0.558895842613217,
3.77591236609064));
#33920=CARTESIAN_POINT('Ctrl Pts',(6.31417864028945,-0.579995970841135,
3.87270290659392));
#33921=CARTESIAN_POINT('Ctrl Pts',(6.30622600094564,-0.601096099069052,
3.9694934470972));
#33922=CARTESIAN_POINT('Ctrl Pts',(6.29827336160184,-0.598156761726356,
4.07104416954258));
#33923=CARTESIAN_POINT('Ctrl Pts',(6.29032072225803,-0.570614590620327,
4.16591643177432));
#33924=CARTESIAN_POINT('Ctrl Pts',(6.28236808291422,-0.543072419514299,
4.26078869400605));
#33925=CARTESIAN_POINT('Ctrl Pts',(6.27441544357042,-0.490927414644939,
4.34898249602413));
#33926=CARTESIAN_POINT('Ctrl Pts',(6.26646280422661,-0.421087730399527,
4.41916768405122));
#33927=CARTESIAN_POINT('Ctrl Pts',(6.2585101648828,-0.351248046154114,4.48935287207832));
#33928=CARTESIAN_POINT('Ctrl Pts',(6.250557525539,-0.263713682532649,4.54152944611444));
#33929=CARTESIAN_POINT('Ctrl Pts',(6.24260488619519,-0.168899197391682,
4.5696117428605));
#33930=CARTESIAN_POINT('Ctrl Pts',(6.23801839454932,-0.114217245248871,
4.58580752565092));
#33931=CARTESIAN_POINT('Ctrl Pts',(6.23343190290344,-0.0571138332845632,
4.59398924930378));
#33932=CARTESIAN_POINT('Ctrl Pts',(6.22884541125756,-1.27841859475647E-5,
4.5940334609955));
#33933=CARTESIAN_POINT('Ctrl Pts',(6.12115458874249,-9.50793186244619E-6,
4.59413936148612));
#33934=CARTESIAN_POINT('Ctrl Pts',(6.12188796076042,-0.00913273504488762,
4.59414606160884));
#33935=CARTESIAN_POINT('Ctrl Pts',(6.12262133277835,-0.0182556526135436,
4.59394031163173));
#33936=CARTESIAN_POINT('Ctrl Pts',(6.12335470479628,-0.0273686726716501,
4.59352013235631));
#33937=CARTESIAN_POINT('Ctrl Pts',(6.13130734414009,-0.126189680404606,
4.58896373511797));
#33938=CARTESIAN_POINT('Ctrl Pts',(6.13925998348389,-0.223846830455152,
4.55919239267511));
#33939=CARTESIAN_POINT('Ctrl Pts',(6.14721262282769,-0.308403173896691,
4.50784224986958));
#33940=CARTESIAN_POINT('Ctrl Pts',(6.1551652621715,-0.392959517338232,4.45649210706404));
#33941=CARTESIAN_POINT('Ctrl Pts',(6.16311790151532,-0.464415054170765,
4.38356316389581));
#33942=CARTESIAN_POINT('Ctrl Pts',(6.17107054085912,-0.514027768136376,
4.29797916579711));
#33943=CARTESIAN_POINT('Ctrl Pts',(6.17902318020293,-0.563640482101988,
4.2123951676984));
#33944=CARTESIAN_POINT('Ctrl Pts',(6.18697581954673,-0.591410373200678,
4.11415611466921));
#33945=CARTESIAN_POINT('Ctrl Pts',(6.19492845889053,-0.593952774873424,
4.0152594949342));
#33946=CARTESIAN_POINT('Ctrl Pts',(6.20288109823434,-0.59649517654617,3.9163628751992));
#33947=CARTESIAN_POINT('Ctrl Pts',(6.21083373757815,-0.573810088792972,
3.81680868875837));
#33948=CARTESIAN_POINT('Ctrl Pts',(6.21878637692196,-0.528651094032059,
3.72879442104321));
#33949=CARTESIAN_POINT('Ctrl Pts',(6.22673901626577,-0.483492099271145,
3.64078015332805));
#33950=CARTESIAN_POINT('Ctrl Pts',(6.23469165560957,-0.415859197502516,
3.56430580433857));
#33951=CARTESIAN_POINT('Ctrl Pts',(6.24264429495337,-0.334059153459168,
3.50867301156809));
#33952=CARTESIAN_POINT('Ctrl Pts',(6.25059693429718,-0.252259109415819,
3.45304021879761));
#33953=CARTESIAN_POINT('Ctrl Pts',(6.25854957364099,-0.156291923097747,
3.41824898224614));
#33954=CARTESIAN_POINT('Ctrl Pts',(6.2665022129848,-0.057819682214149,3.40864436538418));
#33955=CARTESIAN_POINT('Ctrl Pts',(6.2744548523286,0.0406525586694487,3.39903974852221));
#33956=CARTESIAN_POINT('Ctrl Pts',(6.28240749167241,0.141629854118573,3.41462175134974));
#33957=CARTESIAN_POINT('Ctrl Pts',(6.29036013101621,0.232632044389671,3.453312878872));
#33958=CARTESIAN_POINT('Ctrl Pts',(6.29831277036002,0.323634234660771,3.49200400639426));
#33959=CARTESIAN_POINT('Ctrl Pts',(6.30626540970382,0.404661319753841,3.55380425861124));
#33960=CARTESIAN_POINT('Ctrl Pts',(6.31421804904763,0.466059055789261,3.63148218419904));
#33961=CARTESIAN_POINT('Ctrl Pts',(6.32217068839144,0.527456791824679,3.70916010978684));
#33962=CARTESIAN_POINT('Ctrl Pts',(6.33012332773525,0.569225178802449,3.80271570874544));
#33963=CARTESIAN_POINT('Ctrl Pts',(6.33807596707905,0.585790493249255,3.90010619949006));
#33964=CARTESIAN_POINT('Ctrl Pts',(6.34602860642286,0.602355807696062,3.99749669023468));
#33965=CARTESIAN_POINT('Ctrl Pts',(6.35398124576666,0.593718049611903,4.09872207276531));
#33966=CARTESIAN_POINT('Ctrl Pts',(6.36193388511047,0.56173881546021,4.19248215342453));
#33967=CARTESIAN_POINT('Ctrl Pts',(6.36988652445427,0.529759581308516,4.28624223408375));
#33968=CARTESIAN_POINT('Ctrl Pts',(6.37783916379808,0.474438871089287,4.37253701287156));
#33969=CARTESIAN_POINT('Ctrl Pts',(6.38579180314189,0.401374624788453,4.4390182948332));
#33970=CARTESIAN_POINT('Ctrl Pts',(6.39757939834209,0.293077024234899,4.53755846574697));
#33971=CARTESIAN_POINT('Ctrl Pts',(6.40936699354229,0.145797072855576,4.59256860517148));
#33972=CARTESIAN_POINT('Ctrl Pts',(6.42115458874249,-0.000630941829811112,
4.59394485456974));
#33973=CARTESIAN_POINT('Origin',(4.,0.,4.));
#33974=CARTESIAN_POINT('',(6.82884541125756,0.000528213615369061,4.5937871332276));
#33975=CARTESIAN_POINT('',(6.72115458874249,0.000109070110168276,4.59505938903171));
#33976=CARTESIAN_POINT('',(4.,-7.27562663373442E-17,4.5941));
#33977=CARTESIAN_POINT('Ctrl Pts',(6.82884541125756,0.000528213615369061,
4.5937871332276));
#33978=CARTESIAN_POINT('Ctrl Pts',(6.82429524715479,0.0572034606387535,
4.59426930340541));
#33979=CARTESIAN_POINT('Ctrl Pts',(6.81974508305202,0.113754426020979,4.58681959872387));
#33980=CARTESIAN_POINT('Ctrl Pts',(6.81519491894924,0.167823213394864,4.57092612439125));
#33981=CARTESIAN_POINT('Ctrl Pts',(6.79928964026163,0.356822799356826,4.51536985589957));
#33982=CARTESIAN_POINT('Ctrl Pts',(6.78338436157403,0.515493156338912,4.35664088088147));
#33983=CARTESIAN_POINT('Ctrl Pts',(6.76747908288642,0.570983871223461,4.16762126762428));
#33984=CARTESIAN_POINT('Ctrl Pts',(6.7515738041988,0.626474586108011,3.97860165436708));
#33985=CARTESIAN_POINT('Ctrl Pts',(6.73566852551118,0.578785658895023,3.75929140287077));
#33986=CARTESIAN_POINT('Ctrl Pts',(6.71976324682357,0.449805704301045,3.61038767491097));
#33987=CARTESIAN_POINT('Ctrl Pts',(6.70385796813595,0.320825749707067,3.46148394695116));
#33988=CARTESIAN_POINT('Ctrl Pts',(6.68795268944834,0.110554767732096,3.38298674252784));
#33989=CARTESIAN_POINT('Ctrl Pts',(6.67204741076073,-0.0844443642884844,
3.4109402193496));
#33990=CARTESIAN_POINT('Ctrl Pts',(6.65614213207312,-0.279443496309066,
3.43889369617135));
#33991=CARTESIAN_POINT('Ctrl Pts',(6.64023685338551,-0.459170778375258,
3.57329785423817));
#33992=CARTESIAN_POINT('Ctrl Pts',(6.6243315746979,-0.541132009270427,3.75243704050979));
#33993=CARTESIAN_POINT('Ctrl Pts',(6.60842629601029,-0.623093240165596,
3.9315762267814));
#33994=CARTESIAN_POINT('Ctrl Pts',(6.59252101732267,-0.60728841988974,4.15545044125781));
#33995=CARTESIAN_POINT('Ctrl Pts',(6.57661573863506,-0.500919754058047,
4.32127168369798));
#33996=CARTESIAN_POINT('Ctrl Pts',(6.56069229617589,-0.394429615589227,
4.48728229340579));
#33997=CARTESIAN_POINT('Ctrl Pts',(6.54476885371673,-0.197168666623305,
4.59510713395368));
#33998=CARTESIAN_POINT('Ctrl Pts',(6.52884541125757,2.61457539729726E-5,
4.59508370962656));
#33999=CARTESIAN_POINT('Ctrl Pts',(6.42115458874249,-0.000630941829811112,
4.59394485456974));
#34000=CARTESIAN_POINT('Ctrl Pts',(6.4252722722299,-0.0517816819022344,
4.59442561076518));
#34001=CARTESIAN_POINT('Ctrl Pts',(6.42938995571731,-0.102828462800867,
4.58836159088269));
#34002=CARTESIAN_POINT('Ctrl Pts',(6.43350763920472,-0.152073274319339,
4.5753220992581));
#34003=CARTESIAN_POINT('Ctrl Pts',(6.44941291789233,-0.342290043897387,
4.52495476314113));
#34004=CARTESIAN_POINT('Ctrl Pts',(6.46531819657995,-0.5056209461254,4.37051151428857));
#34005=CARTESIAN_POINT('Ctrl Pts',(6.48122347526756,-0.56632363157735,4.18304963962536));
#34006=CARTESIAN_POINT('Ctrl Pts',(6.49712875395518,-0.627026317029301,
3.99558776496215));
#34007=CARTESIAN_POINT('Ctrl Pts',(6.51303403264279,-0.58510078570519,3.77510726448829));
#34008=CARTESIAN_POINT('Ctrl Pts',(6.5289393113304,-0.460166914262479,3.62276494217392));
#34009=CARTESIAN_POINT('Ctrl Pts',(6.54484459001801,-0.335233042819767,
3.47042261985956));
#34010=CARTESIAN_POINT('Ctrl Pts',(6.56074986870563,-0.127290831258456,
3.38621847570468));
#34011=CARTESIAN_POINT('Ctrl Pts',(6.57665514739324,0.068373869747762,3.4088573345089));
#34012=CARTESIAN_POINT('Ctrl Pts',(6.59256042608085,0.26403857075398,3.43149619331313));
#34013=CARTESIAN_POINT('Ctrl Pts',(6.60846570476847,0.447425761205104,3.56097805507645));
#34014=CARTESIAN_POINT('Ctrl Pts',(6.62437098345608,0.534230294511761,3.73782813427527));
#34015=CARTESIAN_POINT('Ctrl Pts',(6.64027626214369,0.621034827818418,3.91467821347409));
#34016=CARTESIAN_POINT('Ctrl Pts',(6.65618154083131,0.611256703980608,4.1388965101084));
#34017=CARTESIAN_POINT('Ctrl Pts',(6.67208681951892,0.509439333868548,4.30754322537844));
#34018=CARTESIAN_POINT('Ctrl Pts',(6.68799209820653,0.40762196375649,4.47618994064847));
#34019=CARTESIAN_POINT('Ctrl Pts',(6.70389737689414,0.213765347370184,4.58926507455422));
#34020=CARTESIAN_POINT('Ctrl Pts',(6.71980265558175,0.016851802420978,4.59484308232941));
#34021=CARTESIAN_POINT('Ctrl Pts',(6.72025329996867,0.0112726493937942,
4.59500112406784));
#34022=CARTESIAN_POINT('Ctrl Pts',(6.72070394435558,0.00569104238866241,
4.59507287148453));
#34023=CARTESIAN_POINT('Ctrl Pts',(6.72115458874249,0.000109070110168276,
4.59505938903171));
#34024=CARTESIAN_POINT('Origin',(4.,0.,4.));
#34025=CARTESIAN_POINT('',(7.12884541125757,-0.000233413975479213,4.59320261234329));
#34026=CARTESIAN_POINT('',(7.02115458874249,0.000491936389841303,4.5936290357477));
#34027=CARTESIAN_POINT('',(4.,-7.27562663373442E-17,4.5941));
#34028=CARTESIAN_POINT('Ctrl Pts',(7.12884541125757,-0.000233413975479213,
4.59320261234329));
#34029=CARTESIAN_POINT('Ctrl Pts',(7.11972691928047,0.113624805666132,4.59280158872514));
#34030=CARTESIAN_POINT('Ctrl Pts',(7.11060842730338,0.227688545642871,4.56127879346404));
#34031=CARTESIAN_POINT('Ctrl Pts',(7.10148993532628,0.322592019514134,4.50005536307953));
#34032=CARTESIAN_POINT('Ctrl Pts',(7.08558465663867,0.488131036726243,4.39326405099382));
#34033=CARTESIAN_POINT('Ctrl Pts',(7.06967937795105,0.595374147168556,4.19610732087965));
#34034=CARTESIAN_POINT('Ctrl Pts',(7.05377409926343,0.595079946532544,3.99911121186167));
#34035=CARTESIAN_POINT('Ctrl Pts',(7.03786882057582,0.594785745896532,3.80211510284369));
#34036=CARTESIAN_POINT('Ctrl Pts',(7.02196354188821,0.486954234182196,3.60527961492189));
#34037=CARTESIAN_POINT('Ctrl Pts',(7.0060582632006,0.321096900356496,3.49898325846904));
#34038=CARTESIAN_POINT('Ctrl Pts',(6.99015298451299,0.155239566530797,3.3926869020162));
#34039=CARTESIAN_POINT('Ctrl Pts',(6.97424770582538,-0.0686435894062663,
3.37692967703231));
#34040=CARTESIAN_POINT('Ctrl Pts',(6.95834242713776,-0.247754555527299,
3.45894666907189));
#34041=CARTESIAN_POINT('Ctrl Pts',(6.94243714845015,-0.426865521648332,
3.54096366111146));
#34042=CARTESIAN_POINT('Ctrl Pts',(6.92653186976253,-0.561204297953336,
3.72075487017451));
#34043=CARTESIAN_POINT('Ctrl Pts',(6.91062659107492,-0.589088840804576,
3.91576771430201));
#34044=CARTESIAN_POINT('Ctrl Pts',(6.89472131238731,-0.616973383655816,
4.11078055842951));
#34045=CARTESIAN_POINT('Ctrl Pts',(6.8788160336997,-0.538403693053295,4.32101503762147));
#34046=CARTESIAN_POINT('Ctrl Pts',(6.86291075501209,-0.389454440281117,
4.44994049623482));
#34047=CARTESIAN_POINT('Ctrl Pts',(6.85155564042725,-0.283116420949728,
4.54198310574898));
#34048=CARTESIAN_POINT('Ctrl Pts',(6.8402005258424,-0.140907108175025,4.59258385846765));
#34049=CARTESIAN_POINT('Ctrl Pts',(6.82884541125756,0.000528213615369061,
4.5937871332276));
#34050=CARTESIAN_POINT('Ctrl Pts',(6.72115458874249,0.000109070110168276,
4.59505938903171));
#34051=CARTESIAN_POINT('Ctrl Pts',(6.73660922304319,-0.191322006690816,
4.59459701474307));
#34052=CARTESIAN_POINT('Ctrl Pts',(6.75206385734389,-0.38318268672033,4.49389457135631));
#34053=CARTESIAN_POINT('Ctrl Pts',(6.76751849164459,-0.49122657597837,4.33588597251985));
#34054=CARTESIAN_POINT('Ctrl Pts',(6.78342377033221,-0.60242093591639,4.17326997329048));
#34055=CARTESIAN_POINT('Ctrl Pts',(6.79932904901982,-0.624839182280325,
3.94995709318712));
#34056=CARTESIAN_POINT('Ctrl Pts',(6.81523432770743,-0.548195780923551,
3.76848141254984));
#34057=CARTESIAN_POINT('Ctrl Pts',(6.83113960639504,-0.471552379566775,
3.58700573191256));
#34058=CARTESIAN_POINT('Ctrl Pts',(6.84704488508266,-0.295847330489284,
3.44736725074137));
#34059=CARTESIAN_POINT('Ctrl Pts',(6.86295016377027,-0.101752734572189,
3.41368297698799));
#34060=CARTESIAN_POINT('Ctrl Pts',(6.87885544245788,0.0923418613449005,
3.37999870323461));
#34061=CARTESIAN_POINT('Ctrl Pts',(6.8947607211455,0.304826004101594,3.45226863689903));
#34062=CARTESIAN_POINT('Ctrl Pts',(6.91066599983311,0.438133727661537,3.59730899203965));
#34063=CARTESIAN_POINT('Ctrl Pts',(6.92657127852072,0.571441451221483,3.74234934718029));
#34064=CARTESIAN_POINT('Ctrl Pts',(6.94247655720833,0.625572755584675,3.96016012379713));
#34065=CARTESIAN_POINT('Ctrl Pts',(6.95838183589594,0.57567402069499,4.15073208753033));
#34066=CARTESIAN_POINT('Ctrl Pts',(6.97428711458356,0.525775285805305,4.34130405126353));
#34067=CARTESIAN_POINT('Ctrl Pts',(6.99019239327118,0.371846511662747,4.5046372021131));
#34068=CARTESIAN_POINT('Ctrl Pts',(7.00609767195879,0.184564651688987,4.56573572985967));
#34069=CARTESIAN_POINT('Ctrl Pts',(7.01111664422002,0.125467135782336,4.58501560681028));
#34070=CARTESIAN_POINT('Ctrl Pts',(7.01613561648126,0.0630485115161635,
4.59411554829291));
#34071=CARTESIAN_POINT('Ctrl Pts',(7.02115458874249,0.000491936389841303,
4.5936290357477));
#34072=CARTESIAN_POINT('Origin',(4.,0.,4.));
#34073=CARTESIAN_POINT('',(7.42884541125756,-0.000438237927964824,4.59464495791636));
#34074=CARTESIAN_POINT('',(7.32115458874249,-0.000317338366111653,4.59328419319629));
#34075=CARTESIAN_POINT('',(4.,-7.27562663373442E-17,4.5941));
#34076=CARTESIAN_POINT('Ctrl Pts',(7.42884541125756,-0.000438237927964824,
4.59464495791636));
#34077=CARTESIAN_POINT('Ctrl Pts',(7.41515859140615,0.169409178821721,4.5932420274804));
#34078=CARTESIAN_POINT('Ctrl Pts',(7.40147177155473,0.340360224580004,4.51673272682389));
#34079=CARTESIAN_POINT('Ctrl Pts',(7.38778495170331,0.450965110664874,4.38826722161738));
#34080=CARTESIAN_POINT('Ctrl Pts',(7.37187967301569,0.579497637321094,4.23897909740477));
#34081=CARTESIAN_POINT('Ctrl Pts',(7.35597439432808,0.626535888751401,4.01952688559808));
#34082=CARTESIAN_POINT('Ctrl Pts',(7.34006911564046,0.570481892017836,3.83067375781486));
#34083=CARTESIAN_POINT('Ctrl Pts',(7.32416383695285,0.51442789528427,3.64182063003164));
#34084=CARTESIAN_POINT('Ctrl Pts',(7.30825855826524,0.355281650386831,3.48356658627189));
#34085=CARTESIAN_POINT('Ctrl Pts',(7.29235327957763,0.166116376105148,3.42857518785077));
#34086=CARTESIAN_POINT('Ctrl Pts',(7.27644800089002,-0.023048898176535,
3.37358378942964));
#34087=CARTESIAN_POINT('Ctrl Pts',(7.2605427222024,-0.242233201842457,3.42185503634715));
#34088=CARTESIAN_POINT('Ctrl Pts',(7.24463744351479,-0.390796368104757,
3.5512248149675));
#34089=CARTESIAN_POINT('Ctrl Pts',(7.22873216482718,-0.539359534367058,
3.68059459358785));
#34090=CARTESIAN_POINT('Ctrl Pts',(7.21282688613957,-0.617301563225728,
3.89106290391106));
#34091=CARTESIAN_POINT('Ctrl Pts',(7.19692160745195,-0.588834786584626,
4.08599160058025));
#34092=CARTESIAN_POINT('Ctrl Pts',(7.18101632876434,-0.560368009943526,
4.28092029724944));
#34093=CARTESIAN_POINT('Ctrl Pts',(7.16511105007672,-0.425492427802657,
4.46030938026461));
#34094=CARTESIAN_POINT('Ctrl Pts',(7.14920577138911,-0.24613717474127,4.54179097474357));
#34095=CARTESIAN_POINT('Ctrl Pts',(7.1424189846786,-0.169606239833077,4.57655919310821));
#34096=CARTESIAN_POINT('Ctrl Pts',(7.13563219796808,-0.0849767524450092,
4.59350108952231));
#34097=CARTESIAN_POINT('Ctrl Pts',(7.12884541125757,-0.000233413975479213,
4.59320261234329));
#34098=CARTESIAN_POINT('Ctrl Pts',(7.02115458874249,0.000491936389841303,
4.5936290357477));
#34099=CARTESIAN_POINT('Ctrl Pts',(7.03204089516887,-0.135195214358064,
4.59257377495492));
#34100=CARTESIAN_POINT('Ctrl Pts',(7.04292720159524,-0.271531381894462,
4.54641716720817));
#34101=CARTESIAN_POINT('Ctrl Pts',(7.05381350802162,-0.376033620593693,
4.46121547122365));
#34102=CARTESIAN_POINT('Ctrl Pts',(7.06971878670923,-0.528715087097646,
4.33673278019746));
#34103=CARTESIAN_POINT('Ctrl Pts',(7.08562406539685,-0.613443074300594,
4.1289034935015));
#34104=CARTESIAN_POINT('Ctrl Pts',(7.10152934408446,-0.591314251018945,
3.93315398851514));
#34105=CARTESIAN_POINT('Ctrl Pts',(7.11743462277207,-0.569185427737295,
3.73740448352876));
#34106=CARTESIAN_POINT('Ctrl Pts',(7.13333990145968,-0.440199793971044,
3.55373476025198));
#34107=CARTESIAN_POINT('Ctrl Pts',(7.14924518014729,-0.263582002606135,
3.46647820559892));
#34108=CARTESIAN_POINT('Ctrl Pts',(7.16515045883491,-0.0869642112412332,
3.37922165094586));
#34109=CARTESIAN_POINT('Ctrl Pts',(7.18105573752253,0.137285737722324,3.38837826491652));
#34110=CARTESIAN_POINT('Ctrl Pts',(7.19696101621014,0.306201705590428,3.48974370695041));
#34111=CARTESIAN_POINT('Ctrl Pts',(7.21286629489775,0.47511767345854,3.59110914898431));
#34112=CARTESIAN_POINT('Ctrl Pts',(7.22877157358536,0.588699660231196,3.78468341908144));
#34113=CARTESIAN_POINT('Ctrl Pts',(7.24467685227297,0.594795648982816,3.98158540759));
#34114=CARTESIAN_POINT('Ctrl Pts',(7.26058213096058,0.600891637734436,4.17848739609855));
#34115=CARTESIAN_POINT('Ctrl Pts',(7.2764874096482,0.499501628465021,4.37871710301853));
#34116=CARTESIAN_POINT('Ctrl Pts',(7.29239268833581,0.337179610128186,4.49033751492072));
#34117=CARTESIAN_POINT('Ctrl Pts',(7.30197998847137,0.239335998647354,4.5576194790522));
#34118=CARTESIAN_POINT('Ctrl Pts',(7.31156728860693,0.119353510611835,4.59270637405629));
#34119=CARTESIAN_POINT('Ctrl Pts',(7.32115458874249,-0.000317338366111653,
4.59328419319629));
#34120=CARTESIAN_POINT('Origin',(4.,0.,4.));
#34121=CARTESIAN_POINT('',(7.72884541125757,0.000455182276646732,4.59460030787683));
#34122=CARTESIAN_POINT('',(7.62115458874249,-0.000367422317862595,4.59479267874092));
#34123=CARTESIAN_POINT('',(4.,-7.27562663373442E-17,4.5941));
#34124=CARTESIAN_POINT('Ctrl Pts',(7.72884541125757,0.000455182276646732,
4.59460030787683));
#34125=CARTESIAN_POINT('Ctrl Pts',(7.72649554221944,0.0296217258780686,
4.59484761241511));
#34126=CARTESIAN_POINT('Ctrl Pts',(7.72414567318131,0.0587549042441869,
4.59288776399295));
#34127=CARTESIAN_POINT('Ctrl Pts',(7.72179580414318,0.0875427725731367,
4.58860617484604));
#34128=CARTESIAN_POINT('Ctrl Pts',(7.70589052545556,0.282395788279217,4.55962589232715));
#34129=CARTESIAN_POINT('Ctrl Pts',(7.68998524676794,0.461428877889185,4.42427810603975));
#34130=CARTESIAN_POINT('Ctrl Pts',(7.67407996808033,0.542437620895056,4.24470879335187));
#34131=CARTESIAN_POINT('Ctrl Pts',(7.65817468939272,0.623446363900926,4.065139480664));
#34132=CARTESIAN_POINT('Ctrl Pts',(7.64226941070511,0.606430760302702,3.84134864157567));
#34133=CARTESIAN_POINT('Ctrl Pts',(7.6263641320175,0.499203655448083,3.67609156159133));
#34134=CARTESIAN_POINT('Ctrl Pts',(7.61045885332988,0.391976550593464,3.51083448160699));
#34135=CARTESIAN_POINT('Ctrl Pts',(7.59455357464227,0.19453794448245,3.40411116072664));
#34136=CARTESIAN_POINT('Ctrl Pts',(7.57864829595466,-0.00245670798462758,
3.40492443279829));
#34137=CARTESIAN_POINT('Ctrl Pts',(7.56274301726704,-0.199451360451705,
3.40573770486994));
#34138=CARTESIAN_POINT('Ctrl Pts',(7.54683773857943,-0.396002059274846,
3.5140875698936));
#34139=CARTESIAN_POINT('Ctrl Pts',(7.53093245989182,-0.50186103876401,3.68022435377194));
#34140=CARTESIAN_POINT('Ctrl Pts',(7.51502718120421,-0.607720018253171,
3.84636113765028));
#34141=CARTESIAN_POINT('Ctrl Pts',(7.4991219025166,-0.622887278408357,4.07028484038331));
#34142=CARTESIAN_POINT('Ctrl Pts',(7.48321662382898,-0.540398655351294,
4.24917917107494));
#34143=CARTESIAN_POINT('Ctrl Pts',(7.46731134514137,-0.45791003229423,4.42807350176658));
#34144=CARTESIAN_POINT('Ctrl Pts',(7.45140606645375,-0.277765526024924,
4.56193846041682));
#34145=CARTESIAN_POINT('Ctrl Pts',(7.43550078776614,-0.0826798719492015,
4.58930892143267));
#34146=CARTESIAN_POINT('Ctrl Pts',(7.43328232892995,-0.0554694406452989,
4.59312653709876));
#34147=CARTESIAN_POINT('Ctrl Pts',(7.43106387009376,-0.0279683367079049,
4.5948723550368));
#34148=CARTESIAN_POINT('Ctrl Pts',(7.42884541125756,-0.000438237927964824,
4.59464495791636));
#34149=CARTESIAN_POINT('Ctrl Pts',(7.32115458874249,-0.000317338366111653,
4.59328419319629));
#34150=CARTESIAN_POINT('Ctrl Pts',(7.32747256729455,-0.0791797758050172,
4.59366497286126));
#34151=CARTESIAN_POINT('Ctrl Pts',(7.3337905458466,-0.157906876560309,4.57905936436794));
#34152=CARTESIAN_POINT('Ctrl Pts',(7.34010852439865,-0.230073660466993,
4.54880513582638));
#34153=CARTESIAN_POINT('Ctrl Pts',(7.35601380308626,-0.411750885321067,
4.47264122794544));
#34154=CARTESIAN_POINT('Ctrl Pts',(7.37191908177388,-0.551851307624962,
4.29730229529918));
#34155=CARTESIAN_POINT('Ctrl Pts',(7.38782436046149,-0.586046744500155,
4.10329655692985));
#34156=CARTESIAN_POINT('Ctrl Pts',(7.4037296391491,-0.620242181375348,3.90929081856053));
#34157=CARTESIAN_POINT('Ctrl Pts',(7.41963491783671,-0.548532632821828,
3.69661827446815));
#34158=CARTESIAN_POINT('Ctrl Pts',(7.43554019652432,-0.403844087697925,
3.56292915991696));
#34159=CARTESIAN_POINT('Ctrl Pts',(7.45144547521194,-0.259155542574025,
3.42924004536577));
#34160=CARTESIAN_POINT('Ctrl Pts',(7.46735075389955,-0.0414880008797467,
3.37453436035576));
#34161=CARTESIAN_POINT('Ctrl Pts',(7.48325603258717,0.149214809903968,3.42393064079835));
#34162=CARTESIAN_POINT('Ctrl Pts',(7.49916131127478,0.339917620687686,3.47332692124094));
#34163=CARTESIAN_POINT('Ctrl Pts',(7.51506658996239,0.50365570056084,3.62682516713614));
#34164=CARTESIAN_POINT('Ctrl Pts',(7.53097186865001,0.56524745100941,3.81394547807041));
#34165=CARTESIAN_POINT('Ctrl Pts',(7.54687714733762,0.626839201457978,4.00106578900469));
#34166=CARTESIAN_POINT('Ctrl Pts',(7.56278242602523,0.58628462248197,4.22180816497804));
#34167=CARTESIAN_POINT('Ctrl Pts',(7.57868770471284,0.462204660718925,4.3748170457164));
#34168=CARTESIAN_POINT('Ctrl Pts',(7.59284333272272,0.351774041004839,4.51099427596058));
#34169=CARTESIAN_POINT('Ctrl Pts',(7.60699896073261,0.175183620117616,4.59352033541115));
#34170=CARTESIAN_POINT('Ctrl Pts',(7.62115458874249,-0.000367422317862596,
4.59479267874092));
#34171=CARTESIAN_POINT('Origin',(4.,0.,4.));
#34172=CARTESIAN_POINT('',(8.02884541125756,0.000208508845897126,4.59318438507865));
#34173=CARTESIAN_POINT('',(7.92115458874249,0.000504499356536197,4.59443266285439));
#34174=CARTESIAN_POINT('',(4.,-7.27562663373442E-17,4.5941));
#34175=CARTESIAN_POINT('Ctrl Pts',(8.02884541125756,0.000208508845897126,
4.59318438507865));
#34176=CARTESIAN_POINT('Ctrl Pts',(8.02192721434511,0.0865993248636432,
4.5934556945658));
#34177=CARTESIAN_POINT('Ctrl Pts',(8.01500901743265,0.17288466952141,4.57582457789876));
#34178=CARTESIAN_POINT('Ctrl Pts',(8.0080908205202,0.250602156771344,4.53974023855861));
#34179=CARTESIAN_POINT('Ctrl Pts',(7.99218554183259,0.42927852421987,4.4567805482338));
#34180=CARTESIAN_POINT('Ctrl Pts',(7.97628026314498,0.562668370741438,4.27628395749428));
#34181=CARTESIAN_POINT('Ctrl Pts',(7.96037498445736,0.589524722071826,4.08112686462655));
#34182=CARTESIAN_POINT('Ctrl Pts',(7.94446970576975,0.616381073402214,3.88596977175883));
#34183=CARTESIAN_POINT('Ctrl Pts',(7.92856442708213,0.536703929541425,3.67615217676291));
#34184=CARTESIAN_POINT('Ctrl Pts',(7.91265914839452,0.387077664089382,3.54801344261061));
#34185=CARTESIAN_POINT('Ctrl Pts',(7.89675386970691,0.237451398637336,3.41987470845831));
#34186=CARTESIAN_POINT('Ctrl Pts',(7.88084859101929,0.0178760115940344,
3.37341483514963));
#34187=CARTESIAN_POINT('Ctrl Pts',(7.86494331233168,-0.170828768780714,
3.42996623095257));
#34188=CARTESIAN_POINT('Ctrl Pts',(7.84903803364407,-0.359533549155462,
3.48651762675552));
#34189=CARTESIAN_POINT('Ctrl Pts',(7.83313275495647,-0.517367722861657,
3.64608029167009));
#34190=CARTESIAN_POINT('Ctrl Pts',(7.81722747626885,-0.571860514742998,
3.83538980050754));
#34191=CARTESIAN_POINT('Ctrl Pts',(7.80132219758124,-0.626353306624339,
4.02469930934499));
#34192=CARTESIAN_POINT('Ctrl Pts',(7.78541691889362,-0.577504716680827,
4.24375566210532));
#34193=CARTESIAN_POINT('Ctrl Pts',(7.769511640206,-0.447743950807975,4.3919774491103));
#34194=CARTESIAN_POINT('Ctrl Pts',(7.75595623055652,-0.337154229471824,
4.51830073342946));
#34195=CARTESIAN_POINT('Ctrl Pts',(7.74240082090705,-0.16779438404434,4.593173711641));
#34196=CARTESIAN_POINT('Ctrl Pts',(7.72884541125757,0.000455182276646732,
4.59460030787683));
#34197=CARTESIAN_POINT('Ctrl Pts',(7.62115458874249,-0.000367422317862596,
4.59479267874092));
#34198=CARTESIAN_POINT('Ctrl Pts',(7.62290423942022,-0.022065717876263,
4.59494994172972));
#34199=CARTESIAN_POINT('Ctrl Pts',(7.62465389009795,-0.043748134618359,
4.59386587358433));
#34200=CARTESIAN_POINT('Ctrl Pts',(7.62640354077568,-0.0652877816099521,
4.59148835294282));
#34201=CARTESIAN_POINT('Ctrl Pts',(7.64230881946329,-0.261094917625702,
4.56987539392751));
#34202=CARTESIAN_POINT('Ctrl Pts',(7.6582140981509,-0.445103845107109,4.44137409039354));
#34203=CARTESIAN_POINT('Ctrl Pts',(7.67411937683852,-0.532825449416136,
4.2649868044631));
#34204=CARTESIAN_POINT('Ctrl Pts',(7.69002465552613,-0.620547053725161,
4.08859951853267));
#34205=CARTESIAN_POINT('Ctrl Pts',(7.70592993421374,-0.611981334861803,
3.86432625020577));
#34206=CARTESIAN_POINT('Ctrl Pts',(7.72183521290136,-0.511061308497056,
3.69514379608856));
#34207=CARTESIAN_POINT('Ctrl Pts',(7.73774049158897,-0.410141282132307,
3.52596134197134));
#34208=CARTESIAN_POINT('Ctrl Pts',(7.75364577027658,-0.216866948266163,
3.4118697020638));
#34209=CARTESIAN_POINT('Ctrl Pts',(7.76955104896419,-0.0199817042712483,
3.40525493058698));
#34210=CARTESIAN_POINT('Ctrl Pts',(7.78545632765181,0.176903539723664,3.39864015911017));
#34211=CARTESIAN_POINT('Ctrl Pts',(7.80136160633942,0.377399693847348,3.49950225606407));
#34212=CARTESIAN_POINT('Ctrl Pts',(7.81726688502703,0.489447406431712,3.66152961365368));
#34213=CARTESIAN_POINT('Ctrl Pts',(7.83317216371464,0.601495119016078,3.82355697124329));
#34214=CARTESIAN_POINT('Ctrl Pts',(7.84907744240226,0.625094390061116,4.04674958946861));
#34215=CARTESIAN_POINT('Ctrl Pts',(7.86498272108987,0.549409432699027,4.22862686054007));
#34216=CARTESIAN_POINT('Ctrl Pts',(7.88088799977748,0.473724475336938,4.41050413161152));
#34217=CARTESIAN_POINT('Ctrl Pts',(7.89679327846509,0.298755289567731,4.55106605552911));
#34218=CARTESIAN_POINT('Ctrl Pts',(7.91269855715271,0.104840323164387,4.58577254351526));
#34219=CARTESIAN_POINT('Ctrl Pts',(7.9155172343493,0.0704753991278659,4.59192310448195));
#34220=CARTESIAN_POINT('Ctrl Pts',(7.91833591154589,0.0355154700816755,
4.59474920414003));
#34221=CARTESIAN_POINT('Ctrl Pts',(7.92115458874249,0.000504499356536197,
4.59443266285439));
#34222=CARTESIAN_POINT('Origin',(4.,0.,4.));
#34223=CARTESIAN_POINT('',(8.32884541125757,-0.000534402448739424,4.5938336238991));
#34224=CARTESIAN_POINT('',(8.2211545887425,0.000116005647334215,4.59313666129657));
#34225=CARTESIAN_POINT('',(4.,-7.27562663373442E-17,4.5941));
#34226=CARTESIAN_POINT('Ctrl Pts',(8.32884541125757,-0.000534402448739424,
4.5938336238991));
#34227=CARTESIAN_POINT('Ctrl Pts',(8.31735888647079,0.142509087977489,4.59259298046846));
#34228=CARTESIAN_POINT('Ctrl Pts',(8.30587236168401,0.286359812054371,4.54070236535691));
#34229=CARTESIAN_POINT('Ctrl Pts',(8.29438583689723,0.393155811111917,4.44670960845581));
#34230=CARTESIAN_POINT('Ctrl Pts',(8.27848055820962,0.541035187969857,4.31655875596735));
#34231=CARTESIAN_POINT('Ctrl Pts',(8.262575279522,0.617867056310918,4.10568264439756));
#34232=CARTESIAN_POINT('Ctrl Pts',(8.24667000083439,0.588373472681163,3.91090666274675));
#34233=CARTESIAN_POINT('Ctrl Pts',(8.23076472214677,0.558879889051408,3.71613068109593));
#34234=CARTESIAN_POINT('Ctrl Pts',(8.21485944345917,0.423060853450833,3.53745482936408));
#34235=CARTESIAN_POINT('Ctrl Pts',(8.19895416477155,0.243278720997716,3.45691949951456));
#34236=CARTESIAN_POINT('Ctrl Pts',(8.18304888608394,0.0634965885445972,
3.37638416966503));
#34237=CARTESIAN_POINT('Ctrl Pts',(8.16714360739632,-0.160248640761069,
3.39398936169784));
#34238=CARTESIAN_POINT('Ctrl Pts',(8.15123832870871,-0.325222623502191,
3.50165151624576));
#34239=CARTESIAN_POINT('Ctrl Pts',(8.1353330500211,-0.490196606243315,3.60931367079368));
#34240=CARTESIAN_POINT('Ctrl Pts',(8.11942777133349,-0.59639934241989,3.80703278785672));
#34241=CARTESIAN_POINT('Ctrl Pts',(8.10352249264588,-0.595067028646789,
4.00402461368555));
#34242=CARTESIAN_POINT('Ctrl Pts',(8.08761721395827,-0.593734714873688,
4.20101643951437));
#34243=CARTESIAN_POINT('Ctrl Pts',(8.07171193527065,-0.484867351150922,
4.39728097410898));
#34244=CARTESIAN_POINT('Ctrl Pts',(8.05580665658303,-0.3184522251018,4.50270184645125));
#34245=CARTESIAN_POINT('Ctrl Pts',(8.04681957480788,-0.224421408301879,
4.56226861162124));
#34246=CARTESIAN_POINT('Ctrl Pts',(8.03783249303272,-0.112017456676448,
4.59283194056482));
#34247=CARTESIAN_POINT('Ctrl Pts',(8.02884541125756,0.000208508845897126,
4.59318438507865));
#34248=CARTESIAN_POINT('Ctrl Pts',(7.92115458874249,0.000504499356536197,
4.59443266285439));
#34249=CARTESIAN_POINT('Ctrl Pts',(7.93424119023351,-0.162045019349314,
4.59296301969496));
#34250=CARTESIAN_POINT('Ctrl Pts',(7.94732779172453,-0.325694779556815,
4.52375140444135));
#34251=CARTESIAN_POINT('Ctrl Pts',(7.96041439321555,-0.436005268305889,
4.40499428651169));
#34252=CARTESIAN_POINT('Ctrl Pts',(7.97631967190316,-0.570075146335334,
4.26065848946726));
#34253=CARTESIAN_POINT('Ctrl Pts',(7.99222495059077,-0.625354155356748,
4.04313584332371));
#34254=CARTESIAN_POINT('Ctrl Pts',(8.00813022927838,-0.576460513088508,
3.85230354456612));
#34255=CARTESIAN_POINT('Ctrl Pts',(8.024035507966,-0.527566870820267,3.66147124580852));
#34256=CARTESIAN_POINT('Ctrl Pts',(8.03994078665361,-0.374500577262366,
3.49732929443689));
#34257=CARTESIAN_POINT('Ctrl Pts',(8.05584606534123,-0.187543198716277,
3.43524473024767));
#34258=CARTESIAN_POINT('Ctrl Pts',(8.07175134402884,-0.000585820170193818,
3.37316016605846));
#34259=CARTESIAN_POINT('Ctrl Pts',(8.08765662271645,0.220262643364076,3.41313298905166));
#34260=CARTESIAN_POINT('Ctrl Pts',(8.10356190140406,0.37359792075985,3.53680937001953));
#34261=CARTESIAN_POINT('Ctrl Pts',(8.11946718009167,0.526933198155627,3.66048575098741));
#34262=CARTESIAN_POINT('Ctrl Pts',(8.13537245877928,0.612755289412907,3.86786568992997));
#34263=CARTESIAN_POINT('Ctrl Pts',(8.1512777374669,0.591658321059451,4.06372909240644));
#34264=CARTESIAN_POINT('Ctrl Pts',(8.16718301615451,0.570561352705995,4.2595924948829));
#34265=CARTESIAN_POINT('Ctrl Pts',(8.18308829484212,0.44254532474181,4.44393936089328));
#34266=CARTESIAN_POINT('Ctrl Pts',(8.19899357352974,0.266389781296621,4.53212540863836));
#34267=CARTESIAN_POINT('Ctrl Pts',(8.20638057860065,0.184576572093718,4.57308230066594));
#34268=CARTESIAN_POINT('Ctrl Pts',(8.21376758367158,0.0923795717789203,
4.59329710918813));
#34269=CARTESIAN_POINT('Ctrl Pts',(8.2211545887425,0.000116005647334215,
4.59313666129657));
#34270=CARTESIAN_POINT('Origin',(4.,0.,4.));
#34271=CARTESIAN_POINT('',(8.62884541125757,3.48566139269993E-5,4.59507810043999));
#34272=CARTESIAN_POINT('',(8.5211545887425,-0.000547905086566465,4.594005652201));
#34273=CARTESIAN_POINT('',(4.,-7.27562663373442E-17,4.5941));
#34274=CARTESIAN_POINT('Ctrl Pts',(8.62884541125757,3.48566139269993E-5,
4.59507810043999));
#34275=CARTESIAN_POINT('Ctrl Pts',(8.62869583728408,0.00188744051982823,
4.59507966949126));
#34276=CARTESIAN_POINT('Ctrl Pts',(8.62854626331059,0.00374001065808006,
4.59507176912216));
#34277=CARTESIAN_POINT('Ctrl Pts',(8.6283966893371,0.00559249142073073,
4.59505435897699));
#34278=CARTESIAN_POINT('Ctrl Pts',(8.61249141064948,0.202580123064263,4.59320301275402));
#34279=CARTESIAN_POINT('Ctrl Pts',(8.59658613196187,0.398557131004382,4.48381890612783));
#34280=CARTESIAN_POINT('Ctrl Pts',(8.58068085327426,0.503539164298441,4.31712659320126));
#34281=CARTESIAN_POINT('Ctrl Pts',(8.56477557458664,0.608521197592498,4.15043428027469));
#34282=CARTESIAN_POINT('Ctrl Pts',(8.54887029589904,0.622508256240502,3.92643376104774));
#34283=CARTESIAN_POINT('Ctrl Pts',(8.53296501721142,0.539078074654942,3.74797659726896));
#34284=CARTESIAN_POINT('Ctrl Pts',(8.51705973852381,0.455647893069379,3.56951943349019));
#34285=CARTESIAN_POINT('Ctrl Pts',(8.50115445983619,0.274800471250253,3.43660562515959));
#34286=CARTESIAN_POINT('Ctrl Pts',(8.48524918114857,0.0795732942734406,
3.41026356994308));
#34287=CARTESIAN_POINT('Ctrl Pts',(8.46934390246096,-0.115653882703369,
3.38392151472657));
#34288=CARTESIAN_POINT('Ctrl Pts',(8.45343862377335,-0.32526081483786,3.46415121262414));
#34289=CARTESIAN_POINT('Ctrl Pts',(8.43753334508574,-0.453004866631874,
3.61411458059983));
#34290=CARTESIAN_POINT('Ctrl Pts',(8.42162806639813,-0.580748918425883,
3.76407794857552));
#34291=CARTESIAN_POINT('Ctrl Pts',(8.40572278771052,-0.626630089879422,
3.98377498662932));
#34292=CARTESIAN_POINT('Ctrl Pts',(8.3898175090229,-0.569581688133314,4.17233010950212));
#34293=CARTESIAN_POINT('Ctrl Pts',(8.37391223033529,-0.512533286387202,
4.36088523237493));
#34294=CARTESIAN_POINT('Ctrl Pts',(8.35800695164768,-0.352555311441432,
4.51829844006673));
#34295=CARTESIAN_POINT('Ctrl Pts',(8.34210167296007,-0.163102881281137,
4.57229224720906));
#34296=CARTESIAN_POINT('Ctrl Pts',(8.33768291905923,-0.110469810133188,
4.58729263485501));
#34297=CARTESIAN_POINT('Ctrl Pts',(8.3332641651584,-0.0555618361628184,
4.59431088730997));
#34298=CARTESIAN_POINT('Ctrl Pts',(8.32884541125757,-0.000534402448739424,
4.5938336238991));
#34299=CARTESIAN_POINT('Ctrl Pts',(8.2211545887425,0.000116005647334215,
4.59313666129657));
#34300=CARTESIAN_POINT('Ctrl Pts',(8.22967286235919,-0.106277085140544,
4.59295164192424));
#34301=CARTESIAN_POINT('Ctrl Pts',(8.23819113597589,-0.212758691085218,
4.56567285125378));
#34302=CARTESIAN_POINT('Ctrl Pts',(8.24670940959258,-0.303508593564514,
4.51186277431583));
#34303=CARTESIAN_POINT('Ctrl Pts',(8.26261468828019,-0.472956366054245,
4.41138886276846));
#34304=CARTESIAN_POINT('Ctrl Pts',(8.2785199669678,-0.587556852107514,4.21841581019395));
#34305=CARTESIAN_POINT('Ctrl Pts',(8.29442524565541,-0.594690356875377,
4.02154867831793));
#34306=CARTESIAN_POINT('Ctrl Pts',(8.31033052434302,-0.60182386164324,3.82468154644191));
#34307=CARTESIAN_POINT('Ctrl Pts',(8.32623580303064,-0.501490385125681,
3.62392033526436));
#34308=CARTESIAN_POINT('Ctrl Pts',(8.34214108171825,-0.339758814980244,
3.51144609945163));
#34309=CARTESIAN_POINT('Ctrl Pts',(8.35804636040587,-0.178027244834812,
3.3989718636389));
#34310=CARTESIAN_POINT('Ctrl Pts',(8.37395163909348,0.0451024189384938,
3.37478460319097));
#34311=CARTESIAN_POINT('Ctrl Pts',(8.38985691778109,0.227178474572579,3.44999008482693));
#34312=CARTESIAN_POINT('Ctrl Pts',(8.4057621964687,0.40925453020667,3.5251955664629));
#34313=CARTESIAN_POINT('Ctrl Pts',(8.42166747515631,0.550276977701535,3.69979379018275));
#34314=CARTESIAN_POINT('Ctrl Pts',(8.43757275384392,0.585494275335268,3.89361663829603));
#34315=CARTESIAN_POINT('Ctrl Pts',(8.45347803253154,0.620711572969,4.0874394864093));
#34316=CARTESIAN_POINT('Ctrl Pts',(8.46938331121915,0.550123720741606,4.30048695891599));
#34317=CARTESIAN_POINT('Ctrl Pts',(8.48528858990677,0.406141674070155,4.4349366697363));
#34318=CARTESIAN_POINT('Ctrl Pts',(8.49724392285201,0.297916389879728,4.53599689564107));
#34319=CARTESIAN_POINT('Ctrl Pts',(8.50919925579725,0.148224117540273,4.59265016978245));
#34320=CARTESIAN_POINT('Ctrl Pts',(8.5211545887425,-0.000547905086566465,
4.594005652201));
#34321=CARTESIAN_POINT('Origin',(4.,0.,4.));
#34322=CARTESIAN_POINT('',(8.92884541125757,0.000516595407308196,4.59372894893997));
#34323=CARTESIAN_POINT('',(8.82115458874249,0.000142235148737217,4.59503945166131));
#34324=CARTESIAN_POINT('',(4.,-7.27562663373442E-17,4.5941));
#34325=CARTESIAN_POINT('Ctrl Pts',(8.92884541125757,0.000516595407308196,
4.59372894893997));
#34326=CARTESIAN_POINT('Ctrl Pts',(8.92412750940976,0.0592956068199462,
4.59421507565108));
#34327=CARTESIAN_POINT('Ctrl Pts',(8.91940960756194,0.117944888069788,4.58619493689145));
#34328=CARTESIAN_POINT('Ctrl Pts',(8.91469170571413,0.17383025386194,4.56912565303288));
#34329=CARTESIAN_POINT('Ctrl Pts',(8.89878642702651,0.362234410233906,4.51158064138869));
#34330=CARTESIAN_POINT('Ctrl Pts',(8.8828811483389,0.519225559109383,4.35118846702123));
#34331=CARTESIAN_POINT('Ctrl Pts',(8.86697586965128,0.572720006672535,4.16159443076672));
#34332=CARTESIAN_POINT('Ctrl Pts',(8.85107059096367,0.626214454235688,3.97200039451221));
#34333=CARTESIAN_POINT('Ctrl Pts',(8.83516531227606,0.576212200486512,3.75320449637065));
#34334=CARTESIAN_POINT('Ctrl Pts',(8.81926003358845,0.445672164925724,3.60566855627755));
#34335=CARTESIAN_POINT('Ctrl Pts',(8.80335475490084,0.315132129364936,3.45813261618446));
#34336=CARTESIAN_POINT('Ctrl Pts',(8.78744947621322,0.104054311992536,3.38185663413984));
#34337=CARTESIAN_POINT('Ctrl Pts',(8.77154419752561,-0.0906432834200916,
3.41186331412789));
#34338=CARTESIAN_POINT('Ctrl Pts',(8.755638918838,-0.285340878832719,3.44186999411594));
#34339=CARTESIAN_POINT('Ctrl Pts',(8.73973364015038,-0.463658252285575,
3.57815933613666));
#34340=CARTESIAN_POINT('Ctrl Pts',(8.72382836146277,-0.543719609875046,
3.75815304026071));
#34341=CARTESIAN_POINT('Ctrl Pts',(8.70792308277515,-0.623780967464517,
3.93814674438476));
#34342=CARTESIAN_POINT('Ctrl Pts',(8.69201780408754,-0.605586309190603,
4.16184481061213));
#34343=CARTESIAN_POINT('Ctrl Pts',(8.67611252539993,-0.497489852380174,
4.32653455081593));
#34344=CARTESIAN_POINT('Ctrl Pts',(8.66035682068581,-0.390409939629295,
4.48967554111606));
#34345=CARTESIAN_POINT('Ctrl Pts',(8.64460111597169,-0.195111159088962,
4.59491282095998));
#34346=CARTESIAN_POINT('Ctrl Pts',(8.62884541125757,3.48566139269993E-5,
4.59507810043999));
#34347=CARTESIAN_POINT('Ctrl Pts',(8.5211545887425,-0.000547905086566465,
4.594005652201));
#34348=CARTESIAN_POINT('Ctrl Pts',(8.52510453448487,-0.0497009834700827,
4.59445349267793));
#34349=CARTESIAN_POINT('Ctrl Pts',(8.52905448022724,-0.0987536084630192,
4.58886509038946));
#34350=CARTESIAN_POINT('Ctrl Pts',(8.53300442596961,-0.146177075786514,
4.57684766499685));
#34351=CARTESIAN_POINT('Ctrl Pts',(8.54890970465722,-0.337137537856201,
4.52845700030318));
#34352=CARTESIAN_POINT('Ctrl Pts',(8.56481498334483,-0.501682220880061,
4.37582372178193));
#34353=CARTESIAN_POINT('Ctrl Pts',(8.58072026203244,-0.564259167724997,
4.18903057354857));
#34354=CARTESIAN_POINT('Ctrl Pts',(8.59662554072005,-0.626836114569933,
4.00223742531521));
#34355=CARTESIAN_POINT('Ctrl Pts',(8.61253081940767,-0.587445325235947,
3.78128440736974));
#34356=CARTESIAN_POINT('Ctrl Pts',(8.62843609809528,-0.464173383698336,
3.62762379780141));
#34357=CARTESIAN_POINT('Ctrl Pts',(8.6443413767829,-0.340901442160722,3.47396318823307));
#34358=CARTESIAN_POINT('Ctrl Pts',(8.66024665547051,-0.133748348419481,
3.38759498704188));
#34359=CARTESIAN_POINT('Ctrl Pts',(8.67615193415812,0.0621699608040676,
3.40817581827756));
#34360=CARTESIAN_POINT('Ctrl Pts',(8.69205721284573,0.25808827002761,3.42875664951325));
#34361=CARTESIAN_POINT('Ctrl Pts',(8.70796249153334,0.44277179473346,3.55628651317581));
#34362=CARTESIAN_POINT('Ctrl Pts',(8.72386777022095,0.531421673692279,3.73220909121499));
#34363=CARTESIAN_POINT('Ctrl Pts',(8.73977304890857,0.620071552651101,3.90813166925417));
#34364=CARTESIAN_POINT('Ctrl Pts',(8.75567832759618,0.612687785862888,4.13244696166997));
#34365=CARTESIAN_POINT('Ctrl Pts',(8.7715836062838,0.512660686655375,4.30215887618246));
#34366=CARTESIAN_POINT('Ctrl Pts',(8.78748888497141,0.412633587447865,4.47187079069495));
#34367=CARTESIAN_POINT('Ctrl Pts',(8.80339416365902,0.21996315582106,4.58697932730413));
#34368=CARTESIAN_POINT('Ctrl Pts',(8.81929944234663,0.0231155027642346,
4.59463151583965));
#34369=CARTESIAN_POINT('Ctrl Pts',(8.81991782447859,0.0154622529370322,
4.59492902566351));
#34370=CARTESIAN_POINT('Ctrl Pts',(8.82053620661054,0.00780268890311657,
4.59506410656044));
#34371=CARTESIAN_POINT('Ctrl Pts',(8.82115458874249,0.000142235148737217,
4.59503945166131));
#34372=CARTESIAN_POINT('Origin',(4.,0.,4.));
#34373=CARTESIAN_POINT('',(9.22884541125756,-0.000264402795292107,4.59322887297718));
#34374=CARTESIAN_POINT('',(9.12115458874249,0.000475196148639644,4.59357609051269));
#34375=CARTESIAN_POINT('',(4.,-7.27562663373442E-17,4.5941));
#34376=CARTESIAN_POINT('Ctrl Pts',(9.22884541125756,-0.000264402795292107,
4.59322887297718));
#34377=CARTESIAN_POINT('Ctrl Pts',(9.21955918153543,0.115675446261185,4.59276508993807));
#34378=CARTESIAN_POINT('Ctrl Pts',(9.21027295181329,0.231857423975292,4.55999255403315));
#34379=CARTESIAN_POINT('Ctrl Pts',(9.20098672209116,0.327844211240712,4.49662776730038));
#34380=CARTESIAN_POINT('Ctrl Pts',(9.18508144340355,0.492248565587605,4.38809775866155));
#34381=CARTESIAN_POINT('Ctrl Pts',(9.16917616471593,0.597407924103304,4.18982173958679));
#34382=CARTESIAN_POINT('Ctrl Pts',(9.15327088602831,0.595037558282966,3.99283966966863));
#34383=CARTESIAN_POINT('Ctrl Pts',(9.1373656073407,0.592667192462628,3.79585759975047));
#34384=CARTESIAN_POINT('Ctrl Pts',(9.12146032865309,0.482767102306254,3.60016947898891));
#34385=CARTESIAN_POINT('Ctrl Pts',(9.10555504996548,0.315798759724268,3.49562701355602));
#34386=CARTESIAN_POINT('Ctrl Pts',(9.08964977127787,0.148830417142278,3.39108454812312));
#34387=CARTESIAN_POINT('Ctrl Pts',(9.07374449259025,-0.0752061778653251,
3.37768773801888));
#34388=CARTESIAN_POINT('Ctrl Pts',(9.05783921390264,-0.253442899077741,
3.46158783167087));
#34389=CARTESIAN_POINT('Ctrl Pts',(9.04193393521502,-0.431679620290152,
3.54548792532286));
#34390=CARTESIAN_POINT('Ctrl Pts',(9.02602865652741,-0.56411646770738,3.72668492273107));
#34391=CARTESIAN_POINT('Ctrl Pts',(9.0101233778398,-0.589944043936388,3.92198082849844));
#34392=CARTESIAN_POINT('Ctrl Pts',(8.99421809915219,-0.615771620165397,
4.11727673426582));
#34393=CARTESIAN_POINT('Ctrl Pts',(8.97831282046457,-0.534989925206181,
4.32667154839236));
#34394=CARTESIAN_POINT('Ctrl Pts',(8.96240754177696,-0.384690495792338,
4.45402003099517));
#34395=CARTESIAN_POINT('Ctrl Pts',(8.95122016493716,-0.278973620993485,
4.54359378149875));
#34396=CARTESIAN_POINT('Ctrl Pts',(8.94003278809737,-0.138863784294423,
4.59257621560968));
#34397=CARTESIAN_POINT('Ctrl Pts',(8.92884541125757,0.000516595407308196,
4.59372894893997));
#34398=CARTESIAN_POINT('Ctrl Pts',(8.82115458874249,0.000142235148737217,
4.59503945166131));
#34399=CARTESIAN_POINT('Ctrl Pts',(8.83644148529816,-0.189230254871984,
4.59442996300828));
#34400=CARTESIAN_POINT('Ctrl Pts',(8.85172838185382,-0.379146468724227,
4.49620311855542));
#34401=CARTESIAN_POINT('Ctrl Pts',(8.86701527840948,-0.487657002993039,
4.34104488491935));
#34402=CARTESIAN_POINT('Ctrl Pts',(8.88292055709709,-0.600556981206626,
4.17961022500168));
#34403=CARTESIAN_POINT('Ctrl Pts',(8.89882583578469,-0.62533206314696,3.95654506470448));
#34404=CARTESIAN_POINT('Ctrl Pts',(8.91473111447231,-0.550606579334316,
3.77427148852754));
#34405=CARTESIAN_POINT('Ctrl Pts',(8.93063639315992,-0.47588109552167,3.5919979123506));
#34406=CARTESIAN_POINT('Ctrl Pts',(8.94654167184753,-0.301655045956043,
3.45051592029392));
#34407=CARTESIAN_POINT('Ctrl Pts',(8.96244695053515,-0.107925661701669,
3.41478805750048));
#34408=CARTESIAN_POINT('Ctrl Pts',(8.97835222922276,0.0858037225526985,
3.37906019470703));
#34409=CARTESIAN_POINT('Ctrl Pts',(8.99425750791037,0.299036441495806,3.4490864611768));
#34410=CARTESIAN_POINT('Ctrl Pts',(9.01016278659798,0.433865051721373,3.5927137579139));
#34411=CARTESIAN_POINT('Ctrl Pts',(9.0260680652856,0.568693661946943,3.736341054651));
#34412=CARTESIAN_POINT('Ctrl Pts',(9.04197334397321,0.625118163454969,3.95356938165542));
#34413=CARTESIAN_POINT('Ctrl Pts',(9.05787862266082,0.577230812276762,4.14465668133936));
#34414=CARTESIAN_POINT('Ctrl Pts',(9.07378390134844,0.529343461098555,4.3357439810233));
#34415=CARTESIAN_POINT('Ctrl Pts',(9.08968918003605,0.377144257234124,4.50069025338676));
#34416=CARTESIAN_POINT('Ctrl Pts',(9.10559445872366,0.190516636080703,4.56375914846174));
#34417=CARTESIAN_POINT('Ctrl Pts',(9.11078116872994,0.129657384941762,4.58432590969837));
#34418=CARTESIAN_POINT('Ctrl Pts',(9.11596787873622,0.0651369761893139,
4.59405891310139));
#34419=CARTESIAN_POINT('Ctrl Pts',(9.12115458874249,0.000475196148639644,
4.59357609051269));
#34420=CARTESIAN_POINT('Origin',(4.,0.,4.));
#34421=CARTESIAN_POINT('',(9.52884541125756,-0.000414715089906426,4.59470005288553));
#34422=CARTESIAN_POINT('',(9.4211545887425,-0.000345133784900094,4.59331940772745));
#34423=CARTESIAN_POINT('',(4.,-7.27562663373442E-17,4.5941));
#34424=CARTESIAN_POINT('Ctrl Pts',(9.52884541125756,-0.000414715089906426,
4.59470005288553));
#34425=CARTESIAN_POINT('Ctrl Pts',(9.5149908536611,0.17147269131647,4.59333531965569));
#34426=CARTESIAN_POINT('Ctrl Pts',(9.50113629606464,0.344448366351018,4.51470554290992));
#34427=CARTESIAN_POINT('Ctrl Pts',(9.48728173846818,0.455032043431697,4.38349290156166));
#34428=CARTESIAN_POINT('Ctrl Pts',(9.47137645978057,0.581984072756561,4.23285845412795));
#34429=CARTESIAN_POINT('Ctrl Pts',(9.45547118109296,0.626706888961734,4.01292269047354));
#34430=CARTESIAN_POINT('Ctrl Pts',(9.43956590240535,0.56866566691212,3.82467080855373));
#34431=CARTESIAN_POINT('Ctrl Pts',(9.42366062371773,0.510624444862503,3.63641892663391));
#34432=CARTESIAN_POINT('Ctrl Pts',(9.40775534503012,0.349819184558098,3.47985092644869));
#34433=CARTESIAN_POINT('Ctrl Pts',(9.39185006634251,0.160084858421151,3.42685620983728));
#34434=CARTESIAN_POINT('Ctrl Pts',(9.37594478765489,-0.0296494677157886,
3.37386149322587));
#34435=CARTESIAN_POINT('Ctrl Pts',(9.36003950896728,-0.248312859685263,
3.42444006018826));
#34436=CARTESIAN_POINT('Ctrl Pts',(9.34413423027966,-0.395504338780113,
3.55536837257802));
#34437=CARTESIAN_POINT('Ctrl Pts',(9.32822895159205,-0.542695817874971,
3.6862966849678));
#34438=CARTESIAN_POINT('Ctrl Pts',(9.31232367290444,-0.618415384095196,
3.89757474278496));
#34439=CARTESIAN_POINT('Ctrl Pts',(9.29641839421683,-0.587895816063128,
4.09219260031737));
#34440=CARTESIAN_POINT('Ctrl Pts',(9.28051311552922,-0.55737624803106,4.28681045784976));
#34441=CARTESIAN_POINT('Ctrl Pts',(9.26460783684159,-0.42061754574671,4.4647681150974));
#34442=CARTESIAN_POINT('Ctrl Pts',(9.24870255815398,-0.240413519515492,
4.54435494461976));
#34443=CARTESIAN_POINT('Ctrl Pts',(9.24208350918851,-0.165420852186184,
4.57747534017911));
#34444=CARTESIAN_POINT('Ctrl Pts',(9.23546446022304,-0.0829041350566004,
4.59355944875842));
#34445=CARTESIAN_POINT('Ctrl Pts',(9.22884541125756,-0.000264402795292107,
4.59322887297718));
#34446=CARTESIAN_POINT('Ctrl Pts',(9.12115458874249,0.000475196148639644,
4.59357609051269));
#34447=CARTESIAN_POINT('Ctrl Pts',(9.13187315742383,-0.133151270259641,
4.59257831599443));
#34448=CARTESIAN_POINT('Ctrl Pts',(9.14259172610516,-0.267381477949042,
4.54795275857003));
#34449=CARTESIAN_POINT('Ctrl Pts',(9.1533102947865,-0.371151898503526,4.46515291500219));
#34450=CARTESIAN_POINT('Ctrl Pts',(9.16921557347411,-0.525136773491911,
4.34228626868117));
#34451=CARTESIAN_POINT('Ctrl Pts',(9.18512085216173,-0.612050485026272,
4.13536145825263));
#34452=CARTESIAN_POINT('Ctrl Pts',(9.20102613084934,-0.591985933785934,
3.93938960239856));
#34453=CARTESIAN_POINT('Ctrl Pts',(9.21693140953695,-0.571921382545595,
3.74341774654449));
#34454=CARTESIAN_POINT('Ctrl Pts',(9.23283668822456,-0.444878568530549,
3.55839884526489));
#34455=CARTESIAN_POINT('Ctrl Pts',(9.24874196691217,-0.269190177198291,
3.46928575052316));
#34456=CARTESIAN_POINT('Ctrl Pts',(9.26464724559978,-0.0935017858660342,
3.38017265578144));
#34457=CARTESIAN_POINT('Ctrl Pts',(9.28055252428739,0.130832182783434,3.38696536757758));
#34458=CARTESIAN_POINT('Ctrl Pts',(9.29645780297501,0.300807061133818,3.48654496003073));
#34459=CARTESIAN_POINT('Ctrl Pts',(9.31236308166262,0.470781939484206,3.58612455248389));
#34460=CARTESIAN_POINT('Ctrl Pts',(9.32826836035024,0.586397727535503,3.77849102559406));
#34461=CARTESIAN_POINT('Ctrl Pts',(9.34417363903785,0.594568546715174,3.97531783326339));
#34462=CARTESIAN_POINT('Ctrl Pts',(9.36007891772546,0.602739365894845,4.17214464093271));
#34463=CARTESIAN_POINT('Ctrl Pts',(9.37598419641307,0.503465216202894,4.37343178316119));
#34464=CARTESIAN_POINT('Ctrl Pts',(9.39188947510069,0.342328587234952,4.48675671999422));
#34465=CARTESIAN_POINT('Ctrl Pts',(9.40164451298129,0.243500144778355,4.55626125828842));
#34466=CARTESIAN_POINT('Ctrl Pts',(9.41139955086189,0.121401365174849,4.59267772446372));
#34467=CARTESIAN_POINT('Ctrl Pts',(9.4211545887425,-0.000345133784900094,
4.59331940772745));
#34468=CARTESIAN_POINT('Origin',(4.,0.,4.));
#34469=CARTESIAN_POINT('',(9.82884541125756,0.000474857175501747,4.59454166667424));
#34470=CARTESIAN_POINT('',(9.7211545887425,-0.000338423355870402,4.59484023865297));
#34471=CARTESIAN_POINT('',(4.,-7.27562663373442E-17,4.5941));
#34472=CARTESIAN_POINT('Ctrl Pts',(9.82884541125756,0.000474857175501747,
4.59454166667424));
#34473=CARTESIAN_POINT('Ctrl Pts',(9.82632780447438,0.0317313679687054,
4.59481419231428));
#34474=CARTESIAN_POINT('Ctrl Pts',(9.82381019769121,0.0629485386443197,
4.59256288124703));
#34475=CARTESIAN_POINT('Ctrl Pts',(9.82129259090804,0.093741277189286,4.58765086492638));
#34476=CARTESIAN_POINT('Ctrl Pts',(9.80538731222043,0.288278045752977,4.55661862072519));
#34477=CARTESIAN_POINT('Ctrl Pts',(9.78948203353282,0.465874751366426,4.41939150759219));
#34478=CARTESIAN_POINT('Ctrl Pts',(9.77357675484521,0.54498650030893,4.23897841027765));
#34479=CARTESIAN_POINT('Ctrl Pts',(9.7576714761576,0.624098249251433,4.05856531296313));
#34480=CARTESIAN_POINT('Ctrl Pts',(9.74176619746998,0.604725041522997,3.83496623146707));
#34481=CARTESIAN_POINT('Ctrl Pts',(9.72586091878237,0.495762234499694,3.67084840431546));
#34482=CARTESIAN_POINT('Ctrl Pts',(9.70995564009475,0.386799427476386,3.50673057716384));
#34483=CARTESIAN_POINT('Ctrl Pts',(9.69405036140714,0.188247021158209,3.40209400435668));
#34484=CARTESIAN_POINT('Ctrl Pts',(9.67814508271953,-0.00872811953311764,
3.40498337331868));
#34485=CARTESIAN_POINT('Ctrl Pts',(9.66223980403192,-0.205703260224436,
3.40787274228067));
#34486=CARTESIAN_POINT('Ctrl Pts',(9.6463345253443,-0.4011011352889,3.51828805301183));
#34487=CARTESIAN_POINT('Ctrl Pts',(9.63042924665669,-0.505203307099277,
3.68553126611098));
#34488=CARTESIAN_POINT('Ctrl Pts',(9.61452396796908,-0.609305478909656,
3.85277447921013));
#34489=CARTESIAN_POINT('Ctrl Pts',(9.59861868928147,-0.622111947465945,
4.07684559467727));
#34490=CARTESIAN_POINT('Ctrl Pts',(9.58271341059386,-0.537742524204099,
4.25486063595701));
#34491=CARTESIAN_POINT('Ctrl Pts',(9.56680813190624,-0.453373100942255,
4.43287567723675));
#34492=CARTESIAN_POINT('Ctrl Pts',(9.55090285321863,-0.271827785862281,
4.5648346443291));
#34493=CARTESIAN_POINT('Ctrl Pts',(9.53499757453102,-0.0764645071000137,
4.59014756226876));
#34494=CARTESIAN_POINT('Ctrl Pts',(9.53294685343987,-0.0512756623106346,
4.5934112419387));
#34495=CARTESIAN_POINT('Ctrl Pts',(9.53089613234871,-0.025857110284879,
4.59490205769144));
#34496=CARTESIAN_POINT('Ctrl Pts',(9.52884541125756,-0.000414715089906426,
4.59470005288553));
#34497=CARTESIAN_POINT('Ctrl Pts',(9.4211545887425,-0.000345133784900094,
4.59331940772745));
#34498=CARTESIAN_POINT('Ctrl Pts',(9.42730482954951,-0.0771024252662454,
4.59372396859559));
#34499=CARTESIAN_POINT('Ctrl Pts',(9.43345507035652,-0.153719688677923,
4.57990840728947));
#34500=CARTESIAN_POINT('Ctrl Pts',(9.43960531116353,-0.224276981305518,
4.55119942103951));
#34501=CARTESIAN_POINT('Ctrl Pts',(9.45551058985114,-0.406746812634079,
4.47695445381419));
#34502=CARTESIAN_POINT('Ctrl Pts',(9.47141586853875,-0.548687367047265,
4.30310178792596));
#34503=CARTESIAN_POINT('Ctrl Pts',(9.48732114722636,-0.58492554696818,4.10946721245096));
#34504=CARTESIAN_POINT('Ctrl Pts',(9.50322642591398,-0.621163726889096,
3.91583263697596));
#34505=CARTESIAN_POINT('Ctrl Pts',(9.5191317046016,-0.55169953231774,3.70241615191419));
#34506=CARTESIAN_POINT('Ctrl Pts',(9.53503698328921,-0.408427982613559,
3.56720957829912));
#34507=CARTESIAN_POINT('Ctrl Pts',(9.55094226197682,-0.265156432909381,
3.43200300468405));
#34508=CARTESIAN_POINT('Ctrl Pts',(9.56684754066442,-0.0480775280723801,
3.37500634251568));
#34509=CARTESIAN_POINT('Ctrl Pts',(9.58275281935204,0.14313528264739,3.42239004773181));
#34510=CARTESIAN_POINT('Ctrl Pts',(9.59865809803965,0.334348093367161,3.46977375294793));
#34511=CARTESIAN_POINT('Ctrl Pts',(9.61456337672728,0.499694809969701,3.62153782554855));
#34512=CARTESIAN_POINT('Ctrl Pts',(9.63046865541489,0.563255215433827,3.80799862400389));
#34513=CARTESIAN_POINT('Ctrl Pts',(9.6463739341025,0.626815620897955,3.99445942245922));
#34514=CARTESIAN_POINT('Ctrl Pts',(9.6622792127901,0.588589715223662,4.21561694676927));
#34515=CARTESIAN_POINT('Ctrl Pts',(9.67818449147771,0.466129217091882,4.36992501817411));
#34516=CARTESIAN_POINT('Ctrl Pts',(9.69250785723264,0.355848439261942,4.50888586187125));
#34517=CARTESIAN_POINT('Ctrl Pts',(9.70683122298757,0.177255492135987,4.59363345408847));
#34518=CARTESIAN_POINT('Ctrl Pts',(9.7211545887425,-0.000338423355870402,
4.59484023865297));
#34519=CARTESIAN_POINT('Origin',(4.,0.,4.));
#34520=CARTESIAN_POINT('',(10.1288454112576,0.000175993811045716,4.59316417414361));
#34521=CARTESIAN_POINT('',(10.0211545887425,0.000517772199431355,4.59437035498519));
#34522=CARTESIAN_POINT('',(4.,-7.27562663373442E-17,4.5941));
#34523=CARTESIAN_POINT('Ctrl Pts',(10.1288454112576,0.000175993811045716,
4.59316417414361));
#34524=CARTESIAN_POINT('Ctrl Pts',(10.1217594766001,0.0886689559287146,
4.59339827721605));
#34525=CARTESIAN_POINT('Ctrl Pts',(10.1146735419426,0.177068724884878,4.57486525982572));
#34526=CARTESIAN_POINT('Ctrl Pts',(10.1075876072851,0.256276603526552,4.53706914692868));
#34527=CARTESIAN_POINT('Ctrl Pts',(10.0916823285975,0.434068729046268,4.45223097977176));
#34528=CARTESIAN_POINT('Ctrl Pts',(10.0757770499098,0.565548899719798,4.27033860735548));
#34529=CARTESIAN_POINT('Ctrl Pts',(10.0598717712222,0.590346983641159,4.0749093118617));
#34530=CARTESIAN_POINT('Ctrl Pts',(10.0439664925346,0.61514506756252,3.87948001636793));
#34531=CARTESIAN_POINT('Ctrl Pts',(10.028061213847,0.533261064731712,3.67051379779667));
#34532=CARTESIAN_POINT('Ctrl Pts',(10.0121559351594,0.382292645022166,3.5439591030842));
#34533=CARTESIAN_POINT('Ctrl Pts',(9.99625065647179,0.231324225312614,3.41740440837173));
#34534=CARTESIAN_POINT('Ctrl Pts',(9.98034537778417,0.011271388724311,3.37326123751805));
#34535=CARTESIAN_POINT('Ctrl Pts',(9.96444009909655,-0.17682691184915,3.43179826703564));
#34536=CARTESIAN_POINT('Ctrl Pts',(9.94853482040894,-0.364925212422603,
3.49033529655323));
#34537=CARTESIAN_POINT('Ctrl Pts',(9.93262954172133,-0.521068976981223,
3.65155252644206));
#34538=CARTESIAN_POINT('Ctrl Pts',(9.91672426303372,-0.573563594737602,
3.84142582527571));
#34539=CARTESIAN_POINT('Ctrl Pts',(9.90081898434611,-0.626058212493981,
4.03129912410937));
#34540=CARTESIAN_POINT('Ctrl Pts',(9.8849137056585,-0.574903683448118,4.24982849188785));
#34541=CARTESIAN_POINT('Ctrl Pts',(9.86900842697089,-0.443588003168223,
4.39667448814241));
#34542=CARTESIAN_POINT('Ctrl Pts',(9.85562075506645,-0.333057953489513,
4.52027659892262));
#34543=CARTESIAN_POINT('Ctrl Pts',(9.842233083162,-0.165735336637852,4.59309247934331));
#34544=CARTESIAN_POINT('Ctrl Pts',(9.82884541125756,0.000474857175501747,
4.59454166667424));
#34545=CARTESIAN_POINT('Ctrl Pts',(9.7211545887425,-0.000338423355870402,
4.59484023865297));
#34546=CARTESIAN_POINT('Ctrl Pts',(9.72273650167518,-0.0199523965301825,
4.59497351934566));
#34547=CARTESIAN_POINT('Ctrl Pts',(9.72431841460787,-0.0395541838993478,
4.59408780127083));
#34548=CARTESIAN_POINT('Ctrl Pts',(9.72590032754056,-0.0590504136254521,
4.592143576127));
#34549=CARTESIAN_POINT('Ctrl Pts',(9.74180560622817,-0.255074455621757,
4.57259544417541));
#34550=CARTESIAN_POINT('Ctrl Pts',(9.75771088491579,-0.4404274490251,4.4460405617726));
#34551=CARTESIAN_POINT('Ctrl Pts',(9.7736161636034,-0.530003140903138,4.2705875768224));
#34552=CARTESIAN_POINT('Ctrl Pts',(9.78952144229101,-0.619578832781174,
4.0951345918722));
#34553=CARTESIAN_POINT('Ctrl Pts',(9.80542672097862,-0.61337722313391,3.87078350437461));
#34554=CARTESIAN_POINT('Ctrl Pts',(9.82133199966623,-0.514245828742901,
3.70054684219675));
#34555=CARTESIAN_POINT('Ctrl Pts',(9.83723727835384,-0.41511443435189,3.53031018001889));
#34556=CARTESIAN_POINT('Ctrl Pts',(9.85314255704146,-0.223053255217129,
3.41418794316076));
#34557=CARTESIAN_POINT('Ctrl Pts',(9.86904783572907,-0.0262486593588972,
3.40549855006092));
#34558=CARTESIAN_POINT('Ctrl Pts',(9.88495311441669,0.170555936499329,3.39680915696108));
#34559=CARTESIAN_POINT('Ctrl Pts',(9.9008583931043,0.372103949081026,3.49555260761951));
#34560=CARTESIAN_POINT('Ctrl Pts',(9.91676367179191,0.485853057801912,3.65639008698476));
#34561=CARTESIAN_POINT('Ctrl Pts',(9.93266895047952,0.5996021665228,3.81722756635002));
#34562=CARTESIAN_POINT('Ctrl Pts',(9.94857422916713,0.625552371382872,4.04015907442209));
#34563=CARTESIAN_POINT('Ctrl Pts',(9.96447950785475,0.551788436173011,4.22282389414861));
#34564=CARTESIAN_POINT('Ctrl Pts',(9.98038478654236,0.478024500963153,4.40548871387512));
#34565=CARTESIAN_POINT('Ctrl Pts',(9.99629006522997,0.304546425683368,4.54788684525607));
#34566=CARTESIAN_POINT('Ctrl Pts',(10.0121953439176,0.111008003250015,4.58463509072946));
#34567=CARTESIAN_POINT('Ctrl Pts',(10.0151817588592,0.0746687445744621,
4.59153503329043));
#34568=CARTESIAN_POINT('Ctrl Pts',(10.0181681738009,0.0376222632219309,
4.59471031472953));
#34569=CARTESIAN_POINT('Ctrl Pts',(10.0211545887425,0.000517772199431355,
4.59437035498519));
#34570=CARTESIAN_POINT('Origin',(4.,0.,4.));
#34571=CARTESIAN_POINT('',(10.4288454112576,-0.000541293539476018,4.59389423388278));
#34572=CARTESIAN_POINT('',(10.3211545887425,8.19078234495683E-5,4.59312629593825));
#34573=CARTESIAN_POINT('',(4.,-7.27562663373442E-17,4.5941));
#34574=CARTESIAN_POINT('Ctrl Pts',(10.4288454112576,-0.000541293539476018,
4.59389423388278));
#34575=CARTESIAN_POINT('Ctrl Pts',(10.4171911487257,0.144553461780974,4.59260897165526));
#34576=CARTESIAN_POINT('Ctrl Pts',(10.4055368861939,0.290497422953868,4.53904330389552));
#34577=CARTESIAN_POINT('Ctrl Pts',(10.3938826236621,0.397841883685798,4.4425412994096));
#34578=CARTESIAN_POINT('Ctrl Pts',(10.3779773449745,0.544341377656434,4.31083916286766));
#34579=CARTESIAN_POINT('Ctrl Pts',(10.3620720662869,0.618946539098701,4.09916502578488));
#34580=CARTESIAN_POINT('Ctrl Pts',(10.3461667875993,0.587401834162399,3.90471069671543));
#34581=CARTESIAN_POINT('Ctrl Pts',(10.3302615089117,0.555857129226098,3.710256367646));
#34582=CARTESIAN_POINT('Ctrl Pts',(10.314356230224,0.418162557911234,3.5330218465899));
#34583=CARTESIAN_POINT('Ctrl Pts',(10.2984509515364,0.237541641988682,3.45438572744188));
#34584=CARTESIAN_POINT('Ctrl Pts',(10.2825456728488,0.0569207260661262,
3.37574960829385));
#34585=CARTESIAN_POINT('Ctrl Pts',(10.2666403941612,-0.16662653446412,3.3957118910539));
#34586=CARTESIAN_POINT('Ctrl Pts',(10.2507351154736,-0.330456695071223,
3.50510674001315));
#34587=CARTESIAN_POINT('Ctrl Pts',(10.234829836786,-0.494286855678321,3.61450158897239));
#34588=CARTESIAN_POINT('Ctrl Pts',(10.2189245580984,-0.59839991636228,3.81332900413083));
#34589=CARTESIAN_POINT('Ctrl Pts',(10.2030192794108,-0.594991564317383,
4.01029584814195));
#34590=CARTESIAN_POINT('Ctrl Pts',(10.1871140007231,-0.591583212272486,
4.20726269215308));
#34591=CARTESIAN_POINT('Ctrl Pts',(10.1712087220355,-0.480653447498727,
4.40236896501689));
#34592=CARTESIAN_POINT('Ctrl Pts',(10.1553034433479,-0.313136524928893,
4.50603012050002));
#34593=CARTESIAN_POINT('Ctrl Pts',(10.1464840993178,-0.220249792163878,
4.56350936438632));
#34594=CARTESIAN_POINT('Ctrl Pts',(10.1376647552877,-0.109964716607974,
4.59287280319057));
#34595=CARTESIAN_POINT('Ctrl Pts',(10.1288454112576,0.000175993811045716,
4.59316417414361));
#34596=CARTESIAN_POINT('Ctrl Pts',(10.0211545887425,0.000517772199431355,
4.59437035498519));
#34597=CARTESIAN_POINT('Ctrl Pts',(10.0340734524885,-0.159991692577292,
4.59289973094197));
#34598=CARTESIAN_POINT('Ctrl Pts',(10.0469923162344,-0.321586704601994,
4.52564765365589));
#34599=CARTESIAN_POINT('Ctrl Pts',(10.0599111799804,-0.431712787135162,
4.40956688772629));
#34600=CARTESIAN_POINT('Ctrl Pts',(10.075816458668,-0.567296385500051,4.2666520796839));
#34601=CARTESIAN_POINT('Ctrl Pts',(10.0917217373556,-0.624864812642908,
4.04972410403331));
#34602=CARTESIAN_POINT('Ctrl Pts',(10.1076270160433,-0.577985082339038,
3.85838710972745));
#34603=CARTESIAN_POINT('Ctrl Pts',(10.1235322947309,-0.531105352035168,
3.6670501154216));
#34604=CARTESIAN_POINT('Ctrl Pts',(10.1394375734185,-0.379777464284567,
3.50130410246047));
#34605=CARTESIAN_POINT('Ctrl Pts',(10.1553428521061,-0.193484782987353,
3.43725262786029));
#34606=CARTESIAN_POINT('Ctrl Pts',(10.1712481307937,-0.00719210169012799,
3.37320115326011));
#34607=CARTESIAN_POINT('Ctrl Pts',(10.1871534094813,0.214065373153706,3.41084421702088));
#34608=CARTESIAN_POINT('Ctrl Pts',(10.2030586881689,0.368695569727689,3.53289771681035));
#34609=CARTESIAN_POINT('Ctrl Pts',(10.2189639668565,0.523325766301663,3.65495121659981));
#34610=CARTESIAN_POINT('Ctrl Pts',(10.2348692455442,0.611328684605784,3.86141515241798));
#34611=CARTESIAN_POINT('Ctrl Pts',(10.2507745242318,0.592297107651237,4.05749001970593));
#34612=CARTESIAN_POINT('Ctrl Pts',(10.2666798029194,0.573265530696689,4.25356488699388));
#34613=CARTESIAN_POINT('Ctrl Pts',(10.282585081607,0.447199458483466,4.43925068575162));
#34614=CARTESIAN_POINT('Ctrl Pts',(10.2984903602946,0.271983097956201,4.5292883529079));
#34615=CARTESIAN_POINT('Ctrl Pts',(10.3060451031106,0.188758241169316,4.57205474716445));
#34616=CARTESIAN_POINT('Ctrl Pts',(10.3135998459265,0.0944446272328244,
4.59324204311815));
#34617=CARTESIAN_POINT('Ctrl Pts',(10.3211545887425,8.19078234495684E-5,
4.59312629593825));
#34618=CARTESIAN_POINT('Origin',(4.,0.,4.));
#34619=CARTESIAN_POINT('',(10.7288454112576,7.37317986114466E-5,4.59506942345298));
#34620=CARTESIAN_POINT('',(10.6211545887425,-0.000548317120500629,4.59406879148573));
#34621=CARTESIAN_POINT('',(4.,-7.27562663373442E-17,4.5941));
#34622=CARTESIAN_POINT('Ctrl Pts',(10.7288454112576,7.37317986114466E-5,
4.59506942345298));
#34623=CARTESIAN_POINT('Ctrl Pts',(10.728528099539,0.00400402563557926,
4.59507627971693));
#34624=CARTESIAN_POINT('Ctrl Pts',(10.7282107878205,0.00793419209028873,
4.59504072157671));
#34625=CARTESIAN_POINT('Ctrl Pts',(10.727893476102,0.0118635052742893,4.59496237136513));
#34626=CARTESIAN_POINT('Ctrl Pts',(10.7119881974144,0.208820685209451,4.59103505989901));
#34627=CARTESIAN_POINT('Ctrl Pts',(10.6960829187267,0.403634001393415,4.47959161118634));
#34628=CARTESIAN_POINT('Ctrl Pts',(10.6801776400391,0.506853420906232,4.31180214209248));
#34629=CARTESIAN_POINT('Ctrl Pts',(10.6642723613515,0.610072840419052,4.14401267299861));
#34630=CARTESIAN_POINT('Ctrl Pts',(10.6483670826639,0.621698363260717,3.91987718352354));
#34631=CARTESIAN_POINT('Ctrl Pts',(10.6324618039763,0.536392041177647,3.74230920804366));
#34632=CARTESIAN_POINT('Ctrl Pts',(10.6165565252887,0.451085719094577,3.56474123256377));
#34633=CARTESIAN_POINT('Ctrl Pts',(10.6006512466011,0.26884755208677,3.43374077107907));
#34634=CARTESIAN_POINT('Ctrl Pts',(10.5847459679135,0.0733535965831807,
3.40945769333085));
#34635=CARTESIAN_POINT('Ctrl Pts',(10.5688406892258,-0.122140358920403,
3.38517461558263));
#34636=CARTESIAN_POINT('Ctrl Pts',(10.5529354105382,-0.33089010291977,3.46760892157089));
#34637=CARTESIAN_POINT('Ctrl Pts',(10.5370301318506,-0.457046584443773,
3.61891026549369));
#34638=CARTESIAN_POINT('Ctrl Pts',(10.521124853163,-0.583203065967777,3.7702116094165));
#34639=CARTESIAN_POINT('Ctrl Pts',(10.5052195744754,-0.626766285016417,
3.99037999127385));
#34640=CARTESIAN_POINT('Ctrl Pts',(10.4893142957878,-0.567733854410369,
4.17832340467295));
#34641=CARTESIAN_POINT('Ctrl Pts',(10.4734090171002,-0.508701423804317,
4.36626681807206));
#34642=CARTESIAN_POINT('Ctrl Pts',(10.4575037384126,-0.347073343543565,
4.52198526301292));
#34643=CARTESIAN_POINT('Ctrl Pts',(10.4415984597249,-0.157062390163684,
4.57397941748279));
#34644=CARTESIAN_POINT('Ctrl Pts',(10.4373474435692,-0.106278015462724,
4.58787593542499));
#34645=CARTESIAN_POINT('Ctrl Pts',(10.4330964274134,-0.0534661480554494,
4.59436304694399));
#34646=CARTESIAN_POINT('Ctrl Pts',(10.4288454112576,-0.000541293539476018,
4.59389423388278));
#34647=CARTESIAN_POINT('Ctrl Pts',(10.3211545887425,8.19078234495684E-5,
4.59312629593825));
#34648=CARTESIAN_POINT('Ctrl Pts',(10.3295051246142,-0.104220686264852,
4.59299835631127));
#34649=CARTESIAN_POINT('Ctrl Pts',(10.3378556604858,-0.208583275928277,
4.56684300569277));
#34650=CARTESIAN_POINT('Ctrl Pts',(10.3462061963575,-0.298097175589899,
4.5150330474864));
#34651=CARTESIAN_POINT('Ctrl Pts',(10.3621114750451,-0.468594439767441,
4.41635053935381));
#34652=CARTESIAN_POINT('Ctrl Pts',(10.3780167537327,-0.585222319281217,
4.22459598753381));
#34653=CARTESIAN_POINT('Ctrl Pts',(10.3939220324203,-0.594430225977177,
4.02781496975607));
#34654=CARTESIAN_POINT('Ctrl Pts',(10.4098273111079,-0.603638132673137,
3.83103395197833));
#34655=CARTESIAN_POINT('Ctrl Pts',(10.4257325897955,-0.505426066551287,
3.62922646824286));
#34656=CARTESIAN_POINT('Ctrl Pts',(10.4416378684831,-0.344888853364916,
3.51505397731042));
#34657=CARTESIAN_POINT('Ctrl Pts',(10.4575431471707,-0.184351640178541,
3.40088148637798));
#34658=CARTESIAN_POINT('Ctrl Pts',(10.4734484258584,0.0385107200723601,
3.37434398824859));
#34659=CARTESIAN_POINT('Ctrl Pts',(10.489353704546,0.221369260089487,3.4476263793543));
#34660=CARTESIAN_POINT('Ctrl Pts',(10.5052589832336,0.40422780010661,3.52090877046001));
#34661=CARTESIAN_POINT('Ctrl Pts',(10.5211642619212,0.54708251988996,3.69401105080081));
#34662=CARTESIAN_POINT('Ctrl Pts',(10.5370695406088,0.584340575799814,3.88745197659776));
#34663=CARTESIAN_POINT('Ctrl Pts',(10.5529748192964,0.621598631709669,4.08089290239472));
#34664=CARTESIAN_POINT('Ctrl Pts',(10.568880097984,0.55326002374602,4.29467247364782));
#34665=CARTESIAN_POINT('Ctrl Pts',(10.5847853766716,0.4107029495177,4.43063215550545));
#34666=CARTESIAN_POINT('Ctrl Pts',(10.5969084473619,0.302045344566967,4.53426120008624));
#34667=CARTESIAN_POINT('Ctrl Pts',(10.6090315180522,0.150270129189204,4.59268036842864));
#34668=CARTESIAN_POINT('Ctrl Pts',(10.6211545887425,-0.000548317120500629,
4.59406879148573));
#34669=CARTESIAN_POINT('Origin',(4.,0.,4.));
#34670=CARTESIAN_POINT('',(11.0288454112576,0.000503618959454472,4.59367252935801));
#34671=CARTESIAN_POINT('',(10.9211545887425,0.000179316795020235,4.59501533910171));
#34672=CARTESIAN_POINT('',(4.,-7.27562663373442E-17,4.5941));
#34673=CARTESIAN_POINT('Ctrl Pts',(11.0288454112576,0.000503618959454472,
4.59367252935801));
#34674=CARTESIAN_POINT('Ctrl Pts',(11.0239597716647,0.0613870506829751,
4.59415995979602));
#34675=CARTESIAN_POINT('Ctrl Pts',(11.0190741320719,0.122135879976345,4.58554712933309));
#34676=CARTESIAN_POINT('Ctrl Pts',(11.014188492479,0.179818659528701,4.56726203449827));
#34677=CARTESIAN_POINT('Ctrl Pts',(10.9982832137914,0.36760588100072,4.50773461262244));
#34678=CARTESIAN_POINT('Ctrl Pts',(10.9823779351038,0.52289792528528,4.34569680405454));
#34679=CARTESIAN_POINT('Ctrl Pts',(10.9664726564162,0.574391255511512,4.15554951523459));
#34680=CARTESIAN_POINT('Ctrl Pts',(10.9505673777285,0.625884585737745,3.96540222641464));
#34681=CARTESIAN_POINT('Ctrl Pts',(10.9346620990409,0.573579201905647,3.74714545734266));
#34682=CARTESIAN_POINT('Ctrl Pts',(10.9187568203533,0.441491523412615,3.60099348269406));
#34683=CARTESIAN_POINT('Ctrl Pts',(10.9028515416657,0.309403844919578,3.45484150804546));
#34684=CARTESIAN_POINT('Ctrl Pts',(10.8869462629781,0.0975338717655902,
3.38079432782024));
#34685=CARTESIAN_POINT('Ctrl Pts',(10.8710409842905,-0.0968366678563846,
3.41285127449999));
#34686=CARTESIAN_POINT('Ctrl Pts',(10.8551357056029,-0.291207207478354,
3.44490822117975));
#34687=CARTESIAN_POINT('Ctrl Pts',(10.8392304269153,-0.468078313568319,
3.58306929476445));
#34688=CARTESIAN_POINT('Ctrl Pts',(10.8233251482276,-0.546238257009186,
3.76389677537701));
#34689=CARTESIAN_POINT('Ctrl Pts',(10.80741986954,-0.624398200450053,3.94472425598957));
#34690=CARTESIAN_POINT('Ctrl Pts',(10.7915145908524,-0.603846981241821,
4.16821814362997));
#34691=CARTESIAN_POINT('Ctrl Pts',(10.7756093121648,-0.494020849794526,
4.33175950034039));
#34692=CARTESIAN_POINT('Ctrl Pts',(10.7600213451957,-0.386385759396791,
4.49203819249975));
#34693=CARTESIAN_POINT('Ctrl Pts',(10.7444333782267,-0.193002309618558,
4.59473260886404));
#34694=CARTESIAN_POINT('Ctrl Pts',(10.7288454112576,7.37317986114466E-5,
4.59506942345298));
#34695=CARTESIAN_POINT('Ctrl Pts',(10.6211545887425,-0.000548317120500629,
4.59406879148573));
#34696=CARTESIAN_POINT('Ctrl Pts',(10.6249367967398,-0.0476013079303647,
4.5945019577127));
#34697=CARTESIAN_POINT('Ctrl Pts',(10.6287190047372,-0.0945611723716044,
4.58938408097059));
#34698=CARTESIAN_POINT('Ctrl Pts',(10.6325012127345,-0.140089514783682,
4.57835619988505));
#34699=CARTESIAN_POINT('Ctrl Pts',(10.6484064914221,-0.331549364363767,
4.53198076994489));
#34700=CARTESIAN_POINT('Ctrl Pts',(10.6643117701097,-0.497693523030948,
4.38109011760241));
#34701=CARTESIAN_POINT('Ctrl Pts',(10.6802170487973,-0.562235622104956,
4.19496684675621));
#34702=CARTESIAN_POINT('Ctrl Pts',(10.6961223274849,-0.626777721178965,
4.00884357591002));
#34703=CARTESIAN_POINT('Ctrl Pts',(10.7120276061725,-0.589717760659791,
3.78748768656011));
#34704=CARTESIAN_POINT('Ctrl Pts',(10.7279328848602,-0.468072106540212,
3.63253643830059));
#34705=CARTESIAN_POINT('Ctrl Pts',(10.7438381635478,-0.346426452420629,
3.47758519004106));
#34706=CARTESIAN_POINT('Ctrl Pts',(10.7597434422354,-0.140195104700642,
3.38903858287192));
#34707=CARTESIAN_POINT('Ctrl Pts',(10.775648720923,0.0559292266755373,3.40755347270721));
#34708=CARTESIAN_POINT('Ctrl Pts',(10.7915539996106,0.252053558051711,3.4260683625425));
#34709=CARTESIAN_POINT('Ctrl Pts',(10.8074592782982,0.438070873084069,3.55164474938222));
#34710=CARTESIAN_POINT('Ctrl Pts',(10.8233645569858,0.528569890453362,3.72662326908837));
#34711=CARTESIAN_POINT('Ctrl Pts',(10.8392698356734,0.619068907822657,3.90160178879453));
#34712=CARTESIAN_POINT('Ctrl Pts',(10.8551751143611,0.614049627528876,4.12598244136713));
#34713=CARTESIAN_POINT('Ctrl Pts',(10.8710803930487,0.515816690734684,4.29673912390739));
#34714=CARTESIAN_POINT('Ctrl Pts',(10.8869856717363,0.417583753940498,4.46749580644764));
#34715=CARTESIAN_POINT('Ctrl Pts',(10.9028909504239,0.226137160645921,4.58462851895556));
#34716=CARTESIAN_POINT('Ctrl Pts',(10.9187962291115,0.0293810870543861,
4.59435487532392));
#34717=CARTESIAN_POINT('Ctrl Pts',(10.9195823489885,0.0196563998352688,
4.59483560139116));
#34718=CARTESIAN_POINT('Ctrl Pts',(10.9203684688655,0.00991874240631306,
4.5950539509358));
#34719=CARTESIAN_POINT('Ctrl Pts',(10.9211545887425,0.000179316795020235,
4.59501533910171));
#34720=CARTESIAN_POINT('Origin',(4.,0.,4.));
#34721=CARTESIAN_POINT('',(11.3288454112576,-0.000294350894641693,4.59325842069974));
#34722=CARTESIAN_POINT('',(11.2211545887425,0.000456638431143918,4.59352536526061));
#34723=CARTESIAN_POINT('',(4.,-7.27562663373442E-17,4.5941));
#34724=CARTESIAN_POINT('Ctrl Pts',(11.3288454112576,-0.000294350894641693,
4.59325842069974));
#34725=CARTESIAN_POINT('Ctrl Pts',(11.3193914437904,0.117725031793324,4.59273125875086));
#34726=CARTESIAN_POINT('Ctrl Pts',(11.3099374763232,0.236024696118704,4.55868066117597));
#34727=CARTESIAN_POINT('Ctrl Pts',(11.300483508856,0.333060002447629,4.49314500997921));
#34728=CARTESIAN_POINT('Ctrl Pts',(11.2845782301684,0.496311419914153,4.38288835848583));
#34729=CARTESIAN_POINT('Ctrl Pts',(11.2686729514808,0.599375291650127,4.18351506848348));
#34730=CARTESIAN_POINT('Ctrl Pts',(11.2527676727932,0.594929048027223,3.98656891995295));
#34731=CARTESIAN_POINT('Ctrl Pts',(11.2368623941056,0.59048280440432,3.78962277142242));
#34732=CARTESIAN_POINT('Ctrl Pts',(11.220957115418,0.478526445422532,3.5951037643637));
#34733=CARTESIAN_POINT('Ctrl Pts',(11.2050518367303,0.310465594643358,3.49232679739763));
#34734=CARTESIAN_POINT('Ctrl Pts',(11.1891465580427,0.142404743864184,3.38954983043155));
#34735=CARTESIAN_POINT('Ctrl Pts',(11.1732412793551,-0.0817605987123653,
3.37851490355812));
#34736=CARTESIAN_POINT('Ctrl Pts',(11.1573360006675,-0.259103191428711,
3.46428878834836));
#34737=CARTESIAN_POINT('Ctrl Pts',(11.1414307219799,-0.436445784145052,
3.5500626731386));
#34738=CARTESIAN_POINT('Ctrl Pts',(11.1255254432923,-0.566965627001181,
3.73264536959251));
#34739=CARTESIAN_POINT('Ctrl Pts',(11.1096201646047,-0.590733529996744,
3.92820262793532));
#34740=CARTESIAN_POINT('Ctrl Pts',(11.0937148859171,-0.614501432992307,
4.12375988627813));
#34741=CARTESIAN_POINT('Ctrl Pts',(11.0778096072294,-0.531517396127296,
4.33229170650985));
#34742=CARTESIAN_POINT('Ctrl Pts',(11.0619043285418,-0.379884178365051,
4.45804909903384));
#34743=CARTESIAN_POINT('Ctrl Pts',(11.0508846894471,-0.274828280424841,
4.54517747360242));
#34744=CARTESIAN_POINT('Ctrl Pts',(11.0398650503523,-0.136819945681758,
4.59257312212411));
#34745=CARTESIAN_POINT('Ctrl Pts',(11.0288454112576,0.000503618959454472,
4.59367252935801));
#34746=CARTESIAN_POINT('Ctrl Pts',(10.9211545887425,0.000179316795020235,
4.59501533910171));
#34747=CARTESIAN_POINT('Ctrl Pts',(10.9362737475531,-0.187135527734918,
4.59427273168419));
#34748=CARTESIAN_POINT('Ctrl Pts',(10.9513929063637,-0.375104412928531,
4.49848156101044));
#34749=CARTESIAN_POINT('Ctrl Pts',(10.9665120651743,-0.484035620954107,
4.34616539940523));
#34750=CARTESIAN_POINT('Ctrl Pts',(10.982417343862,-0.598630701482551,4.1859295668894));
#34751=CARTESIAN_POINT('Ctrl Pts',(10.9983226225496,-0.625755308650954,
3.96313790162893));
#34752=CARTESIAN_POINT('Ctrl Pts',(11.0142279012372,-0.55295497039508,3.7800869107734));
#34753=CARTESIAN_POINT('Ctrl Pts',(11.0301331799248,-0.480154632139201,
3.59703591991786));
#34754=CARTESIAN_POINT('Ctrl Pts',(11.0460384586124,-0.307429348459053,
3.45372560346725));
#34755=CARTESIAN_POINT('Ctrl Pts',(11.0619437373,-0.114087262216405,3.41595799577618));
#34756=CARTESIAN_POINT('Ctrl Pts',(11.0778490159876,0.0792548240262376,
3.37819038808511));
#34757=CARTESIAN_POINT('Ctrl Pts',(11.0937542946752,0.293213712831377,3.4459654891536));
#34758=CARTESIAN_POINT('Ctrl Pts',(11.1096595733629,0.429548534313776,3.58816383989905));
#34759=CARTESIAN_POINT('Ctrl Pts',(11.1255648520505,0.565883355796175,3.7303621906445));
#34760=CARTESIAN_POINT('Ctrl Pts',(11.1414701307381,0.624594109955846,3.94698379106692));
#34761=CARTESIAN_POINT('Ctrl Pts',(11.1573754094257,0.578723302329844,4.13856516675647));
#34762=CARTESIAN_POINT('Ctrl Pts',(11.1732806881133,0.53285249470384,4.33014654244603));
#34763=CARTESIAN_POINT('Ctrl Pts',(11.1891859668009,0.382400125292158,4.49668769340272));
#34764=CARTESIAN_POINT('Ctrl Pts',(11.2050912454885,0.196447557013804,4.56171996888228));
#34765=CARTESIAN_POINT('Ctrl Pts',(11.2104456932399,0.133847376870746,4.58361282144047));
#34766=CARTESIAN_POINT('Ctrl Pts',(11.2158001409912,0.0672239414478651,
4.5940016224088));
#34767=CARTESIAN_POINT('Ctrl Pts',(11.2211545887425,0.000456638431143918,
4.59352536526061));
#34768=CARTESIAN_POINT('Origin',(4.,0.,4.));
#34769=CARTESIAN_POINT('',(11.6288454112576,-0.000389145320547679,4.59475273347735));
#34770=CARTESIAN_POINT('',(11.5211545887425,-0.0003715675665865,4.59335763259963));
#34771=CARTESIAN_POINT('',(4.,-7.27562663373442E-17,4.5941));
#34772=CARTESIAN_POINT('Ctrl Pts',(11.6288454112576,-0.000389145320547679,
4.59475273347735));
#34773=CARTESIAN_POINT('Ctrl Pts',(11.6148231159161,0.173538999407471,4.59343557735163));
#34774=CARTESIAN_POINT('Ctrl Pts',(11.6008008205746,0.348531733704351,4.51264940831536));
#34775=CARTESIAN_POINT('Ctrl Pts',(11.586778525233,0.459048433726307,4.37867598496766));
#34776=CARTESIAN_POINT('Ctrl Pts',(11.5708732465454,0.584405864209301,4.22671194604376));
#34777=CARTESIAN_POINT('Ctrl Pts',(11.5549679678578,0.626808276394098,4.00631705984067));
#34778=CARTESIAN_POINT('Ctrl Pts',(11.5390626891702,0.566786276503563,3.81868733396413));
#34779=CARTESIAN_POINT('Ctrl Pts',(11.5231574104826,0.506764276613028,3.6310576080876));
#34780=CARTESIAN_POINT('Ctrl Pts',(11.507252131795,0.344317864647159,3.47619304253762));
#34781=CARTESIAN_POINT('Ctrl Pts',(11.4913468531074,0.154035560439752,3.4252008940353));
#34782=CARTESIAN_POINT('Ctrl Pts',(11.4754415744198,-0.0362467437676612,
3.37420874553297));
#34783=CARTESIAN_POINT('Ctrl Pts',(11.4595362957322,-0.254364940216614,
3.4270890140783));
#34784=CARTESIAN_POINT('Ctrl Pts',(11.4436310170445,-0.400168380917644,
3.55956131753494));
#34785=CARTESIAN_POINT('Ctrl Pts',(11.4277257383569,-0.545971821618673,
3.69203362099157));
#34786=CARTESIAN_POINT('Ctrl Pts',(11.4118204596693,-0.619460506571779,
3.90409795935952));
#34787=CARTESIAN_POINT('Ctrl Pts',(11.3959151809817,-0.586891540696359,
4.09838336016249));
#34788=CARTESIAN_POINT('Ctrl Pts',(11.3800099022941,-0.554322574820941,
4.29266876096545));
#34789=CARTESIAN_POINT('Ctrl Pts',(11.3641046236065,-0.415695958117004,
4.46917522420345));
#34790=CARTESIAN_POINT('Ctrl Pts',(11.3481993449189,-0.234663168166497,
4.54685844933023));
#34791=CARTESIAN_POINT('Ctrl Pts',(11.3417480336984,-0.161234786808821,
4.57836740127901));
#34792=CARTESIAN_POINT('Ctrl Pts',(11.335296722478,-0.080829826651965,4.59361815176584));
#34793=CARTESIAN_POINT('Ctrl Pts',(11.3288454112576,-0.000294350894641693,
4.59325842069974));
#34794=CARTESIAN_POINT('Ctrl Pts',(11.2211545887425,0.000456638431143918,
4.59352536526061));
#34795=CARTESIAN_POINT('Ctrl Pts',(11.2317054196788,-0.131106980996848,
4.59258691018808));
#34796=CARTESIAN_POINT('Ctrl Pts',(11.2422562506151,-0.263229208150973,
4.54946171071576));
#34797=CARTESIAN_POINT('Ctrl Pts',(11.2528070815514,-0.366229002642205,
4.4690386804108));
#34798=CARTESIAN_POINT('Ctrl Pts',(11.268712360239,-0.521500226874852,4.34780171645731));
#34799=CARTESIAN_POINT('Ctrl Pts',(11.2846176389266,-0.610589908195122,
4.1418043885479));
#34800=CARTESIAN_POINT('Ctrl Pts',(11.3005229176142,-0.592591834014348,
3.94563195463032));
#34801=CARTESIAN_POINT('Ctrl Pts',(11.3164281963018,-0.574593759833574,
3.74945952071274));
#34802=CARTESIAN_POINT('Ctrl Pts',(11.3323334749894,-0.449507930151742,
3.56311198078699));
#34803=CARTESIAN_POINT('Ctrl Pts',(11.3482387536771,-0.274768466013715,
3.47215224147272));
#34804=CARTESIAN_POINT('Ctrl Pts',(11.3641440323647,-0.100029001875688,
3.38119250215845));
#34805=CARTESIAN_POINT('Ctrl Pts',(11.3800493110523,0.12436409671854,3.38562056345565));
#34806=CARTESIAN_POINT('Ctrl Pts',(11.3959545897399,0.295379012183608,3.48340324695247));
#34807=CARTESIAN_POINT('Ctrl Pts',(11.4118598684275,0.466393927648671,3.5811859304493));
#34808=CARTESIAN_POINT('Ctrl Pts',(11.4277651471151,0.584030659984583,3.77232323614575));
#34809=CARTESIAN_POINT('Ctrl Pts',(11.4436704258027,0.594275398502411,3.96905299961855));
#34810=CARTESIAN_POINT('Ctrl Pts',(11.4595757044903,0.60452013702024,4.16578276309136));
#34811=CARTESIAN_POINT('Ctrl Pts',(11.475480983178,0.507372881719984,4.36810498434052));
#34812=CARTESIAN_POINT('Ctrl Pts',(11.4913862618656,0.34743954227408,4.48312185891572));
#34813=CARTESIAN_POINT('Ctrl Pts',(11.5013090374912,0.247662438486696,4.55487707062799));
#34814=CARTESIAN_POINT('Ctrl Pts',(11.5112318131169,0.123448374926332,4.59265218509947));
#34815=CARTESIAN_POINT('Ctrl Pts',(11.5211545887425,-0.0003715675665865,
4.59335763259963));
#34816=CARTESIAN_POINT('Origin',(4.,0.,4.));
#34817=CARTESIAN_POINT('',(11.9288454112576,0.000492284285450728,4.5944814532616));
#34818=CARTESIAN_POINT('',(11.8211545887425,-0.000307672146732893,4.59488449882539));
#34819=CARTESIAN_POINT('',(4.,-7.27562663373442E-17,4.5941));
#34820=CARTESIAN_POINT('Ctrl Pts',(11.9288454112576,0.000492284285450728,
4.5944814532616));
#34821=CARTESIAN_POINT('Ctrl Pts',(11.9261600667293,0.0338400408399785,
4.59477876231094));
#34822=CARTESIAN_POINT('Ctrl Pts',(11.9234747222011,0.0671420792079604,
4.59221542322669));
#34823=CARTESIAN_POINT('Ctrl Pts',(11.9207893776729,0.0999293694653808,
4.5866302815369));
#34824=CARTESIAN_POINT('Ctrl Pts',(11.9048840989853,0.294128282668868,4.55354952256816));
#34825=CARTESIAN_POINT('Ctrl Pts',(11.8889788202977,0.470268877700486,4.41445832512751));
#34826=CARTESIAN_POINT('Ctrl Pts',(11.8730735416101,0.547474845215755,4.2332214826164));
#34827=CARTESIAN_POINT('Ctrl Pts',(11.8571682629225,0.624680812731027,4.05198464010529));
#34828=CARTESIAN_POINT('Ctrl Pts',(11.8412629842349,0.602952152729945,3.82860215252373));
#34829=CARTESIAN_POINT('Ctrl Pts',(11.8253577055472,0.492265746621211,3.66564180763548));
#34830=CARTESIAN_POINT('Ctrl Pts',(11.8094524268596,0.38157934051248,3.50268146274723));
#34831=CARTESIAN_POINT('Ctrl Pts',(11.793547148172,0.181935188296101,3.40014326055229));
#34832=CARTESIAN_POINT('Ctrl Pts',(11.7776418694844,-0.0149985615777061,
3.40510840546499));
#34833=CARTESIAN_POINT('Ctrl Pts',(11.7617365907968,-0.211932311451519,
3.41007355037768));
#34834=CARTESIAN_POINT('Ctrl Pts',(11.7458313121092,-0.406155658982761,
3.52254204239802));
#34835=CARTESIAN_POINT('Ctrl Pts',(11.7299260334216,-0.508489459897291,
3.69087310813977));
#34836=CARTESIAN_POINT('Ctrl Pts',(11.714020754734,-0.610823260811815,3.8592041738815));
#34837=CARTESIAN_POINT('Ctrl Pts',(11.6981154760463,-0.621267515109637,
4.08339781334463));
#34838=CARTESIAN_POINT('Ctrl Pts',(11.6822101973587,-0.53502666307716,4.26051379213839));
#34839=CARTESIAN_POINT('Ctrl Pts',(11.6663049186711,-0.448785811044678,
4.43762977093217));
#34840=CARTESIAN_POINT('Ctrl Pts',(11.6503996399835,-0.265859852681883,
4.56766808905658));
#34841=CARTESIAN_POINT('Ctrl Pts',(11.6344943612959,-0.070240649109886,
4.59092065229643));
#34842=CARTESIAN_POINT('Ctrl Pts',(11.6326113779498,-0.0470818155087989,
4.59367346098309));
#34843=CARTESIAN_POINT('Ctrl Pts',(11.6307283946037,-0.0237450789937817,
4.59492960773286));
#34844=CARTESIAN_POINT('Ctrl Pts',(11.6288454112576,-0.000389145320547679,
4.59475273347735));
#34845=CARTESIAN_POINT('Ctrl Pts',(11.5211545887425,-0.0003715675665865,
4.59335763259963));
#34846=CARTESIAN_POINT('Ctrl Pts',(11.5271370918045,-0.0750233800274846,
4.5937829512795));
#34847=CARTESIAN_POINT('Ctrl Pts',(11.5331195948664,-0.149531931096223,
4.58073359799715));
#34848=CARTESIAN_POINT('Ctrl Pts',(11.5391020979284,-0.218455391669058,
4.55353248138526));
#34849=CARTESIAN_POINT('Ctrl Pts',(11.555007376616,-0.40169756257477,4.48121470137836));
#34850=CARTESIAN_POINT('Ctrl Pts',(11.5709126553036,-0.545462480794654,
4.3088676134633));
#34851=CARTESIAN_POINT('Ctrl Pts',(11.5868179339912,-0.583739378074245,
4.1156257090067));
#34852=CARTESIAN_POINT('Ctrl Pts',(11.6027232126789,-0.622016275353834,
3.92238380455011));
#34853=CARTESIAN_POINT('Ctrl Pts',(11.6186284913665,-0.554805151693135,
3.70824708355197));
#34854=CARTESIAN_POINT('Ctrl Pts',(11.6345337700541,-0.412966511608993,
3.57153806891708));
#34855=CARTESIAN_POINT('Ctrl Pts',(11.6504390487417,-0.271127871524847,
3.43482905428217));
#34856=CARTESIAN_POINT('Ctrl Pts',(11.6663443274293,-0.0546617150172531,
3.37554774601052));
#34857=CARTESIAN_POINT('Ctrl Pts',(11.6822496061169,0.137039856773353,3.42091361287512));
#34858=CARTESIAN_POINT('Ctrl Pts',(11.6981548848045,0.328741428563947,3.46627947973972));
#34859=CARTESIAN_POINT('Ctrl Pts',(11.7140601634921,0.495678415637556,3.61629252174057));
#34860=CARTESIAN_POINT('Ctrl Pts',(11.7299654421798,0.56120041605148,3.80207309651931));
#34861=CARTESIAN_POINT('Ctrl Pts',(11.7458707208674,0.626722416465409,3.98785367129807));
#34862=CARTESIAN_POINT('Ctrl Pts',(11.761775999555,0.590829430219633,4.20940177885472));
#34863=CARTESIAN_POINT('Ctrl Pts',(11.7776812782426,0.470001998091193,4.36499190112672));
#34864=CARTESIAN_POINT('Ctrl Pts',(11.7921723817426,0.359917612963646,4.5067481450567));
#34865=CARTESIAN_POINT('Ctrl Pts',(11.8066634852425,0.179330777996457,4.59375393408315));
#34866=CARTESIAN_POINT('Ctrl Pts',(11.8211545887425,-0.000307672146732893,
4.59488449882539));
#34867=CARTESIAN_POINT('Origin',(4.,0.,4.));
#34868=CARTESIAN_POINT('',(12.2288454112576,0.000142795628640946,4.59314744373127));
#34869=CARTESIAN_POINT('',(12.1211545887425,0.00052868291625318,4.59430727435519));
#34870=CARTESIAN_POINT('',(4.,-7.27562663373442E-17,4.5941));
#34871=CARTESIAN_POINT('Ctrl Pts',(12.2288454112576,0.000142795628640946,
4.59314744373127));
#34872=CARTESIAN_POINT('Ctrl Pts',(12.221591738855,0.0907369315914116,4.59334157666405));
#34873=CARTESIAN_POINT('Ctrl Pts',(12.2143380664525,0.181251971066953,4.57388161006077));
#34874=CARTESIAN_POINT('Ctrl Pts',(12.2070843940499,0.261922584292681,4.53433840020651));
#34875=CARTESIAN_POINT('Ctrl Pts',(12.1911791153623,0.438810719578057,4.44763117963851));
#34876=CARTESIAN_POINT('Ctrl Pts',(12.1752738366747,0.56836661021043,4.26436322928705));
#34877=CARTESIAN_POINT('Ctrl Pts',(12.1593685579871,0.591103672269137,4.06868343852597));
#34878=CARTESIAN_POINT('Ctrl Pts',(12.1434632792995,0.613840734327844,3.87300364776488));
#34879=CARTESIAN_POINT('Ctrl Pts',(12.1275580006119,0.529758967812885,3.66491201659415));
#34880=CARTESIAN_POINT('Ctrl Pts',(12.1116527219243,0.377465162701742,3.53995541841648));
#34881=CARTESIAN_POINT('Ctrl Pts',(12.0957474432367,0.225171357590603,3.41499882023882));
#34882=CARTESIAN_POINT('Ctrl Pts',(12.0798421645491,0.00466551388328543,
3.37317725505421));
#34883=CARTESIAN_POINT('Ctrl Pts',(12.0639368858614,-0.182805413822737,
3.43369341627091));
#34884=CARTESIAN_POINT('Ctrl Pts',(12.0480316071738,-0.37027634152876,3.49420957748762));
#34885=CARTESIAN_POINT('Ctrl Pts',(12.0321263284862,-0.524712353233489,
3.65706346510565));
#34886=CARTESIAN_POINT('Ctrl Pts',(12.0162210497986,-0.575202966010955,
3.84747946371059));
#34887=CARTESIAN_POINT('Ctrl Pts',(12.000315771111,-0.625693578788423,4.03789546231555));
#34888=CARTESIAN_POINT('Ctrl Pts',(11.9844104924234,-0.572238792638624,
4.25587357190742));
#34889=CARTESIAN_POINT('Ctrl Pts',(11.9685052137358,-0.439382783876041,
4.40132746645495));
#34890=CARTESIAN_POINT('Ctrl Pts',(11.9552852795764,-0.328957325572706,
4.52222386487166));
#34891=CARTESIAN_POINT('Ctrl Pts',(11.942065345417,-0.163678510702966,4.59301780268865));
#34892=CARTESIAN_POINT('Ctrl Pts',(11.9288454112576,0.000492284285450728,
4.5944814532616));
#34893=CARTESIAN_POINT('Ctrl Pts',(11.8211545887425,-0.000307672146732893,
4.59488449882539));
#34894=CARTESIAN_POINT('Ctrl Pts',(11.8225687639301,-0.0178384446610953,
4.59499482973335));
#34895=CARTESIAN_POINT('Ctrl Pts',(11.8239829391178,-0.035360185088601,
4.59428731490513));
#34896=CARTESIAN_POINT('Ctrl Pts',(11.8253971143054,-0.0528064866265509,
4.59273302680715));
#34897=CARTESIAN_POINT('Ctrl Pts',(11.8413023929931,-0.249025661204777,
4.57525189322826));
#34898=CARTESIAN_POINT('Ctrl Pts',(11.8572076716807,-0.435702132350142,
4.45065748908313));
#34899=CARTESIAN_POINT('Ctrl Pts',(11.8731129503683,-0.527121962142897,
4.27615829360067));
#34900=CARTESIAN_POINT('Ctrl Pts',(11.8890182290559,-0.618541791935657,
4.10165909811819));
#34901=CARTESIAN_POINT('Ctrl Pts',(11.9049235077435,-0.614704980375792,
3.87725511129838));
#34902=CARTESIAN_POINT('Ctrl Pts',(11.9208287864311,-0.517373229009482,
3.70598315013913));
#34903=CARTESIAN_POINT('Ctrl Pts',(11.9367340651187,-0.420041477643178,
3.53471118897989));
#34904=CARTESIAN_POINT('Ctrl Pts',(11.9526393438063,-0.229214786470442,
3.41657125348121));
#34905=CARTESIAN_POINT('Ctrl Pts',(11.9685446224939,-0.0325126988662629,
3.4058082039356));
#34906=CARTESIAN_POINT('Ctrl Pts',(11.9844499011816,0.164189388737916,3.39504515438998));
#34907=CARTESIAN_POINT('Ctrl Pts',(12.0003551798692,0.366766872773537,3.49165899079743));
#34908=CARTESIAN_POINT('Ctrl Pts',(12.0162604585568,0.482204742918021,3.65128872687397));
#34909=CARTESIAN_POINT('Ctrl Pts',(12.0321657372444,0.597642613062508,3.81091846295053));
#34910=CARTESIAN_POINT('Ctrl Pts',(12.048071015932,0.625940869315854,4.03356409869619));
#34911=CARTESIAN_POINT('Ctrl Pts',(12.0639762946196,0.554106149607013,4.21699617753661));
#34912=CARTESIAN_POINT('Ctrl Pts',(12.0798815733072,0.482271429898174,4.40042825637702));
#34913=CARTESIAN_POINT('Ctrl Pts',(12.0957868519948,0.310303734227154,4.5446467783122));
#34914=CARTESIAN_POINT('Ctrl Pts',(12.1116921306825,0.117163353092859,4.583432699452));
#34915=CARTESIAN_POINT('Ctrl Pts',(12.1148462833691,0.0788619649798074,
4.59112427906975));
#34916=CARTESIAN_POINT('Ctrl Pts',(12.1180004360558,0.0397279339241207,
4.59466958677844));
#34917=CARTESIAN_POINT('Ctrl Pts',(12.1211545887425,0.00052868291625318,
4.59430727435519));
#34918=CARTESIAN_POINT('Origin',(4.,0.,4.));
#34919=CARTESIAN_POINT('',(12.5288454112576,-0.000545899910317726,4.59395595168017));
#34920=CARTESIAN_POINT('',(12.4211545887425,4.74932194801069E-5,4.59311952367199));
#34921=CARTESIAN_POINT('',(4.,-7.27562663373442E-17,4.5941));
#34922=CARTESIAN_POINT('Ctrl Pts',(12.5288454112576,-0.000545899910317726,
4.59395595168017));
#34923=CARTESIAN_POINT('Ctrl Pts',(12.5170234109807,0.14659828900878,4.5926299020853));
#34924=CARTESIAN_POINT('Ctrl Pts',(12.5052014107038,0.29463204299547,4.53735693360054));
#34925=CARTESIAN_POINT('Ctrl Pts',(12.493379410427,0.402483765871145,4.43832383497591));
#34926=CARTESIAN_POINT('Ctrl Pts',(12.4774741317394,0.547587104485886,4.30508504322883));
#34927=CARTESIAN_POINT('Ctrl Pts',(12.4615688530518,0.619957272242066,4.09263639239171));
#34928=CARTESIAN_POINT('Ctrl Pts',(12.4456635743641,0.586364949835353,3.89852531496775));
#34929=CARTESIAN_POINT('Ctrl Pts',(12.4297582956765,0.55277262742864,3.7044142375438));
#34930=CARTESIAN_POINT('Ctrl Pts',(12.4138530169889,0.41321781485904,3.52864073353302));
#34931=CARTESIAN_POINT('Ctrl Pts',(12.3979477383013,0.231778177981285,3.45191255961345));
#34932=CARTESIAN_POINT('Ctrl Pts',(12.3820424596137,0.0503385411035255,
3.37518438569388));
#34933=CARTESIAN_POINT('Ctrl Pts',(12.3661371809261,-0.172985920082391,
3.39750154186552));
#34934=CARTESIAN_POINT('Ctrl Pts',(12.3502319022385,-0.335654061078685,
3.50861693417539));
#34935=CARTESIAN_POINT('Ctrl Pts',(12.3343266235509,-0.498322202074975,
3.61973232648525));
#34936=CARTESIAN_POINT('Ctrl Pts',(12.3184213448632,-0.600334022881645,
3.81964595493332));
#34937=CARTESIAN_POINT('Ctrl Pts',(12.3025160661756,-0.594850011148503,
4.0165659389844));
#34938=CARTESIAN_POINT('Ctrl Pts',(12.286610787488,-0.58936599941536,4.21348592303547));
#34939=CARTESIAN_POINT('Ctrl Pts',(12.2707055088004,-0.476386155142398,
4.40741226268955));
#34940=CARTESIAN_POINT('Ctrl Pts',(12.2548002301128,-0.307786043036728,
4.50930218712431));
#34941=CARTESIAN_POINT('Ctrl Pts',(12.2461486238277,-0.216076754679914,
4.564724762732));
#34942=CARTESIAN_POINT('Ctrl Pts',(12.2374970175426,-0.107910718865932,
4.59291589733543));
#34943=CARTESIAN_POINT('Ctrl Pts',(12.2288454112576,0.000142795628640946,
4.59314744373127));
#34944=CARTESIAN_POINT('Ctrl Pts',(12.1211545887425,0.00052868291625318,
4.59430727435519));
#34945=CARTESIAN_POINT('Ctrl Pts',(12.1339057147434,-0.157940052872902,
4.59284257311225));
#34946=CARTESIAN_POINT('Ctrl Pts',(12.1466568407444,-0.317474678016714,
4.52751565545538));
#34947=CARTESIAN_POINT('Ctrl Pts',(12.1594079667453,-0.427372353356377,
4.41409399619463));
#34948=CARTESIAN_POINT('Ctrl Pts',(12.1753132454329,-0.564454612073754,
4.27261605145303));
#34949=CARTESIAN_POINT('Ctrl Pts',(12.1912185241205,-0.62430606291093,4.0563068416254));
#34950=CARTESIAN_POINT('Ctrl Pts',(12.2071238028081,-0.579445451749542,
3.8644864045766));
#34951=CARTESIAN_POINT('Ctrl Pts',(12.2230290814957,-0.534584840588155,
3.6726659675278));
#34952=CARTESIAN_POINT('Ctrl Pts',(12.2389343601834,-0.38501216742821,3.50533430325784));
#34953=CARTESIAN_POINT('Ctrl Pts',(12.254839638871,-0.199404875886796,3.43932303278057));
#34954=CARTESIAN_POINT('Ctrl Pts',(12.2707449175586,-0.0137975843453769,
3.37331176230329));
#34955=CARTESIAN_POINT('Ctrl Pts',(12.2866501962462,0.207844325577514,3.40862088561871));
#34956=CARTESIAN_POINT('Ctrl Pts',(12.3025554749338,0.363752265741203,3.52903794710619));
#34957=CARTESIAN_POINT('Ctrl Pts',(12.3184607536214,0.519660205904889,3.64945500859368));
#34958=CARTESIAN_POINT('Ctrl Pts',(12.334366032309,0.609834176309377,3.85498000825323));
#34959=CARTESIAN_POINT('Ctrl Pts',(12.3502713109967,0.592870104691008,4.05124456128685));
#34960=CARTESIAN_POINT('Ctrl Pts',(12.3661765896843,0.575906033072638,4.24750911432049));
#34961=CARTESIAN_POINT('Ctrl Pts',(12.3820818683719,0.451803919431404,4.4345132207282));
#34962=CARTESIAN_POINT('Ctrl Pts',(12.3979871470595,0.277546204023914,4.52639250633888));
#34963=CARTESIAN_POINT('Ctrl Pts',(12.4057096276205,0.192938958450368,4.57100260157974));
#34964=CARTESIAN_POINT('Ctrl Pts',(12.4134321081815,0.0965080911524262,
4.59318808505049));
#34965=CARTESIAN_POINT('Ctrl Pts',(12.4211545887425,4.74932194801069E-5,
4.59311952367199));
#34966=CARTESIAN_POINT('Origin',(4.,0.,4.));
#34967=CARTESIAN_POINT('',(12.8288454112576,0.000112157221815526,4.59505491513413));
#34968=CARTESIAN_POINT('',(12.7211545887425,-0.000546355209092884,4.59413239245978));
#34969=CARTESIAN_POINT('',(4.,-7.27562663373442E-17,4.5941));
#34970=CARTESIAN_POINT('Ctrl Pts',(12.8288454112576,0.000112157221815526,
4.59505491513413));
#34971=CARTESIAN_POINT('Ctrl Pts',(12.828360361794,0.00612048155630211,
4.59507046002904));
#34972=CARTESIAN_POINT('Ctrl Pts',(12.8278753123304,0.0121283652366354,
4.59498736156652));
#34973=CARTESIAN_POINT('Ctrl Pts',(12.8273902628668,0.0181332013859869,
4.59480429815638));
#34974=CARTESIAN_POINT('Ctrl Pts',(12.8114849841792,0.215038052543873,4.58880145767424));
#34975=CARTESIAN_POINT('Ctrl Pts',(12.7955797054916,0.408666038032992,4.47531104548453));
#34976=CARTESIAN_POINT('Ctrl Pts',(12.779674426804,0.510111378641258,4.30644305748136));
#34977=CARTESIAN_POINT('Ctrl Pts',(12.7637691481164,0.611556719249521,4.1375750694782));
#34978=CARTESIAN_POINT('Ctrl Pts',(12.7478638694288,0.620819414976937,3.9133295056616));
#34979=CARTESIAN_POINT('Ctrl Pts',(12.7319585907412,0.533646427817818,3.7366704418887));
#34980=CARTESIAN_POINT('Ctrl Pts',(12.7160533120536,0.446473440658691,3.56001137811579));
#34981=CARTESIAN_POINT('Ctrl Pts',(12.700148033366,0.26286477061301,3.43093881438659));
#34982=CARTESIAN_POINT('Ctrl Pts',(12.6842427546783,0.0671257511235207,
3.4087174113557));
#34983=CARTESIAN_POINT('Ctrl Pts',(12.6683374759907,-0.128613268365957,
3.38649600832481));
#34984=CARTESIAN_POINT('Ctrl Pts',(12.6524321973031,-0.336482637299241,
3.47112576599221));
#34985=CARTESIAN_POINT('Ctrl Pts',(12.6365269186155,-0.461037535689932,
3.62374828002683));
#34986=CARTESIAN_POINT('Ctrl Pts',(12.6206216399279,-0.585592434080627,
3.77637079406146));
#34987=CARTESIAN_POINT('Ctrl Pts',(12.6047163612403,-0.626832861928724,
3.9969860644633));
#34988=CARTESIAN_POINT('Ctrl Pts',(12.5888110825527,-0.565822959504995,
4.18429689252621));
#34989=CARTESIAN_POINT('Ctrl Pts',(12.5729058038651,-0.504813057081268,
4.37160772058911));
#34990=CARTESIAN_POINT('Ctrl Pts',(12.5570005251774,-0.341552824385721,
4.52561410631309));
#34991=CARTESIAN_POINT('Ctrl Pts',(12.5410952464898,-0.151004453301302,
4.57560283284656));
#34992=CARTESIAN_POINT('Ctrl Pts',(12.5370119680791,-0.102085973774189,
4.58843617527608));
#34993=CARTESIAN_POINT('Ctrl Pts',(12.5329286896683,-0.0513689988622793,
4.59441396466913));
#34994=CARTESIAN_POINT('Ctrl Pts',(12.5288454112576,-0.000545899910317726,
4.59395595168017));
#34995=CARTESIAN_POINT('Ctrl Pts',(12.4211545887425,4.74932194801069E-5,
4.59311952367199));
#34996=CARTESIAN_POINT('Ctrl Pts',(12.4293373868691,-0.102162877376194,
4.59304687552285));
#34997=CARTESIAN_POINT('Ctrl Pts',(12.4375201849957,-0.204406628577491,
4.5679880979308));
#34998=CARTESIAN_POINT('Ctrl Pts',(12.4457029831223,-0.292652646395614,
4.51814611323009));
#34999=CARTESIAN_POINT('Ctrl Pts',(12.4616082618099,-0.46418046423393,4.42126596969699));
#35000=CARTESIAN_POINT('Ctrl Pts',(12.4775135404976,-0.582822782736806,
4.23075121781716));
#35001=CARTESIAN_POINT('Ctrl Pts',(12.4934188191852,-0.594104068590283,
4.03407817163935));
#35002=CARTESIAN_POINT('Ctrl Pts',(12.5093240978728,-0.605385354443759,
3.83740512546155));
#35003=CARTESIAN_POINT('Ctrl Pts',(12.5252293765604,-0.509305607647849,
3.63457378498577));
#35004=CARTESIAN_POINT('Ctrl Pts',(12.541134655248,-0.34998058313236,3.51871572067214));
#35005=CARTESIAN_POINT('Ctrl Pts',(12.5570399339356,-0.19065555861687,3.4028576563585));
#35006=CARTESIAN_POINT('Ctrl Pts',(12.5729452126232,0.031914743618199,3.37397286820701));
#35007=CARTESIAN_POINT('Ctrl Pts',(12.5888504913108,0.215535456959467,3.44532402892222));
#35008=CARTESIAN_POINT('Ctrl Pts',(12.6047557699985,0.399156170300736,3.51667518963742));
#35009=CARTESIAN_POINT('Ctrl Pts',(12.6206610486861,0.543827294748204,3.68826229921932));
#35010=CARTESIAN_POINT('Ctrl Pts',(12.6365663273737,0.583121970486127,3.88129981619987));
#35011=CARTESIAN_POINT('Ctrl Pts',(12.6524716060613,0.622416646224052,4.07433733318042));
#35012=CARTESIAN_POINT('Ctrl Pts',(12.6683768847489,0.556334873252426,4.28882525755962));
#35013=CARTESIAN_POINT('Ctrl Pts',(12.6842821634365,0.415218606030559,4.42627980869829));
#35014=CARTESIAN_POINT('Ctrl Pts',(12.6965729718718,0.306170972122536,4.53249785050629));
#35015=CARTESIAN_POINT('Ctrl Pts',(12.7088637803072,0.152317016475741,4.59271595401221));
#35016=CARTESIAN_POINT('Ctrl Pts',(12.7211545887425,-0.000546355209092884,
4.59413239245978));
#35017=CARTESIAN_POINT('Origin',(4.,0.,4.));
#35018=CARTESIAN_POINT('',(13.1288454112576,0.000488576923893258,4.59361798633976));
#35019=CARTESIAN_POINT('',(13.0211545887425,0.000215375668158819,4.59498635240753));
#35020=CARTESIAN_POINT('',(4.,-7.27562663373442E-17,4.5941));
#35021=CARTESIAN_POINT('Ctrl Pts',(13.1288454112576,0.000488576923893258,
4.59361798633976));
#35022=CARTESIAN_POINT('Ctrl Pts',(13.1237920339197,0.0634769139372694,
4.59410397103046));
#35023=CARTESIAN_POINT('Ctrl Pts',(13.1187386565818,0.126326538027094,4.58487602541266));
#35024=CARTESIAN_POINT('Ctrl Pts',(13.1136852792439,0.185787091792062,4.56533540718874));
#35025=CARTESIAN_POINT('Ctrl Pts',(13.0977800005563,0.372936519850693,4.50383218710482));
#35026=CARTESIAN_POINT('Ctrl Pts',(13.0818747218686,0.526512210440984,4.34016674272733));
#35027=CARTESIAN_POINT('Ctrl Pts',(13.065969443181,0.575998703695535,4.14948732200047));
#35028=CARTESIAN_POINT('Ctrl Pts',(13.0500641644934,0.625485196950086,3.9588079012736));
#35029=CARTESIAN_POINT('Ctrl Pts',(13.0341588858058,0.570882492868891,3.74111450419737));
#35030=CARTESIAN_POINT('Ctrl Pts',(13.0182536071182,0.437261843116128,3.59636272886105));
#35031=CARTESIAN_POINT('Ctrl Pts',(13.0023483284306,0.303641193363369,3.45161095352474));
#35032=CARTESIAN_POINT('Ctrl Pts',(12.986443049743,0.0910025979390456,3.37980079992835));
#35033=CARTESIAN_POINT('Ctrl Pts',(12.9705377710554,-0.10301929613509,3.41390445256627));
#35034=CARTESIAN_POINT('Ctrl Pts',(12.9546324923678,-0.297041190209231,
3.4480081052042));
#35035=CARTESIAN_POINT('Ctrl Pts',(12.9387272136801,-0.472446382933184,
3.58802556407645));
#35036=CARTESIAN_POINT('Ctrl Pts',(12.9228219349925,-0.54869623058984,3.76966673571907));
#35037=CARTESIAN_POINT('Ctrl Pts',(12.9069166563049,-0.624946078246494,
3.95130790736168));
#35038=CARTESIAN_POINT('Ctrl Pts',(12.8910113776173,-0.602040580835857,
4.17457279177466));
#35039=CARTESIAN_POINT('Ctrl Pts',(12.8751060989297,-0.490496973717212,
4.33694759959386));
#35040=CARTESIAN_POINT('Ctrl Pts',(12.8596858697056,-0.382355015061345,
4.49437060399126));
#35041=CARTESIAN_POINT('Ctrl Pts',(12.8442656404816,-0.190898750836606,
4.59456072668396));
#35042=CARTESIAN_POINT('Ctrl Pts',(12.8288454112576,0.000112157221815526,
4.59505491513413));
#35043=CARTESIAN_POINT('Ctrl Pts',(12.7211545887425,-0.000546355209092884,
4.59413239245978));
#35044=CARTESIAN_POINT('Ctrl Pts',(12.7247690589948,-0.0455002825709059,
4.59454893744622));
#35045=CARTESIAN_POINT('Ctrl Pts',(12.7283835292471,-0.0903685417208244,
4.58988016539195));
#35046=CARTESIAN_POINT('Ctrl Pts',(12.7319979994994,-0.13398639330236,4.5798004937111));
#35047=CARTESIAN_POINT('Ctrl Pts',(12.747903278187,-0.325924363941296,4.53544544968711));
#35048=CARTESIAN_POINT('Ctrl Pts',(12.7638085568746,-0.493649543747071,
4.38631418374101));
#35049=CARTESIAN_POINT('Ctrl Pts',(12.7797138355622,-0.560149626020051,
4.20088146397168));
#35050=CARTESIAN_POINT('Ctrl Pts',(12.7956191142498,-0.626649708293032,
4.01544874420235));
#35051=CARTESIAN_POINT('Ctrl Pts',(12.8115243929374,-0.591924693033219,
3.79371457060979));
#35052=CARTESIAN_POINT('Ctrl Pts',(12.827429671625,-0.471918838153678,3.63748989490844));
#35053=CARTESIAN_POINT('Ctrl Pts',(12.8433349503126,-0.351912983274129,
3.48126521920708));
#35054=CARTESIAN_POINT('Ctrl Pts',(12.8592402290002,-0.146626288774854,
3.39055004139693));
#35055=CARTESIAN_POINT('Ctrl Pts',(12.8751455076879,0.0496822801939141,
3.40699693328572));
#35056=CARTESIAN_POINT('Ctrl Pts',(12.8910507863755,0.245990849162665,3.42344382517451));
#35057=CARTESIAN_POINT('Ctrl Pts',(12.9069560650631,0.433321292600904,3.54705278676224));
#35058=CARTESIAN_POINT('Ctrl Pts',(12.9228613437507,0.525659396179275,3.72106781235173));
#35059=CARTESIAN_POINT('Ctrl Pts',(12.9387666224383,0.617997499757654,3.89508283794124));
#35060=CARTESIAN_POINT('Ctrl Pts',(12.9546719011259,0.615343263476151,4.11950392753251));
#35061=CARTESIAN_POINT('Ctrl Pts',(12.9705771798135,0.518915400343756,4.29128641125856));
#35062=CARTESIAN_POINT('Ctrl Pts',(12.9864824585012,0.422487537211366,4.46306889498459));
#35063=CARTESIAN_POINT('Ctrl Pts',(13.0023877371888,0.232286047228094,4.58221277284539));
#35064=CARTESIAN_POINT('Ctrl Pts',(13.0182930158764,0.0356434078328121,
4.59401221668908));
#35065=CARTESIAN_POINT('Ctrl Pts',(13.0192468734984,0.0238505254767134,
4.59471984273368));
#35066=CARTESIAN_POINT('Ctrl Pts',(13.0202007311205,0.0120344772878951,
4.59504140054066));
#35067=CARTESIAN_POINT('Ctrl Pts',(13.0211545887425,0.000215375668158819,
4.59498635240753));
#35068=CARTESIAN_POINT('Origin',(4.,0.,4.));
#35069=CARTESIAN_POINT('',(13.4288454112576,-0.000323145728561625,4.59329116515504));
#35070=CARTESIAN_POINT('',(13.3211545887425,0.000436239896754628,4.59347700091179));
#35071=CARTESIAN_POINT('',(4.,-7.27562663373442E-17,4.5941));
#35072=CARTESIAN_POINT('Ctrl Pts',(13.4288454112576,-0.000323145728561625,
4.59329116515504));
#35073=CARTESIAN_POINT('Ctrl Pts',(13.4192237060453,0.11977362227264,4.59270025156928));
#35074=CARTESIAN_POINT('Ctrl Pts',(13.4096020008331,0.240190260834984,4.55734300206483));
#35075=CARTESIAN_POINT('Ctrl Pts',(13.3999802956209,0.338238798929947,4.48960747645051));
#35076=CARTESIAN_POINT('Ctrl Pts',(13.3840750169333,0.500319146323361,4.37763642888821));
#35077=CARTESIAN_POINT('Ctrl Pts',(13.3681697382457,0.601276083433826,4.17718801339723));
#35078=CARTESIAN_POINT('Ctrl Pts',(13.3522644595581,0.594754455875995,3.9802996620979));
#35079=CARTESIAN_POINT('Ctrl Pts',(13.3363591808704,0.588232828318166,3.78341131079859));
#35080=CARTESIAN_POINT('Ctrl Pts',(13.3204539021828,0.474232636092054,3.59008302369095));
#35081=CARTESIAN_POINT('Ctrl Pts',(13.3045486234952,0.305097944517489,3.48908297116948));
#35082=CARTESIAN_POINT('Ctrl Pts',(13.2886433448076,0.135963252942929,3.388082918648));
#35083=CARTESIAN_POINT('Ctrl Pts',(13.27273806612,-0.0883059379800925,3.3794111007127));
#35084=CARTESIAN_POINT('Ctrl Pts',(13.2568327874324,-0.264734703826722,
3.46704924928509));
#35085=CARTESIAN_POINT('Ctrl Pts',(13.2409275087448,-0.441163469673367,
3.55468739785749));
#35086=CARTESIAN_POINT('Ctrl Pts',(13.2250222300572,-0.569751810443623,
3.7386355129376));
#35087=CARTESIAN_POINT('Ctrl Pts',(13.2091169513696,-0.591457400179852,
3.9344324022836));
#35088=CARTESIAN_POINT('Ctrl Pts',(13.1932116726819,-0.613162989916079,
4.1302292916296));
#35089=CARTESIAN_POINT('Ctrl Pts',(13.1773063939943,-0.527985828618295,
4.33787495524147));
#35090=CARTESIAN_POINT('Ctrl Pts',(13.1614011153067,-0.375035665205916,
4.46202728915223));
#35091=CARTESIAN_POINT('Ctrl Pts',(13.150549213957,-0.270680367988337,4.54673431669939));
#35092=CARTESIAN_POINT('Ctrl Pts',(13.1396973126073,-0.134776053786733,
4.59257435599745));
#35093=CARTESIAN_POINT('Ctrl Pts',(13.1288454112576,0.000488576923893258,
4.59361798633976));
#35094=CARTESIAN_POINT('Ctrl Pts',(13.0211545887425,0.000215375668158819,
4.59498635240753));
#35095=CARTESIAN_POINT('Ctrl Pts',(13.0361060098081,-0.185045360160338,
4.59412349007018));
#35096=CARTESIAN_POINT('Ctrl Pts',(13.0510574308736,-0.371056311319581,
4.5007301079696));
#35097=CARTESIAN_POINT('Ctrl Pts',(13.0660088519392,-0.480360474535337,
4.35124746348123));
#35098=CARTESIAN_POINT('Ctrl Pts',(13.0819141306268,-0.596637928700896,
4.19222825660313));
#35099=CARTESIAN_POINT('Ctrl Pts',(13.0978194093145,-0.626109048224722,
3.96973483302036));
#35100=CARTESIAN_POINT('Ctrl Pts',(13.1137246880021,-0.555241941841719,
3.78592675992164));
#35101=CARTESIAN_POINT('Ctrl Pts',(13.1296299666897,-0.484374835458714,
3.60211868682292));
#35102=CARTESIAN_POINT('Ctrl Pts',(13.1455352453773,-0.313169503168878,
3.45699596420825));
#35103=CARTESIAN_POINT('Ctrl Pts',(13.1614405240649,-0.120236190459409,
3.4171928066662));
#35104=CARTESIAN_POINT('Ctrl Pts',(13.1773458027525,0.0726971222500488,
3.37738964912416));
#35105=CARTESIAN_POINT('Ctrl Pts',(13.1932510814401,0.287358415379145,3.44290605665475));
#35106=CARTESIAN_POINT('Ctrl Pts',(13.2091563601277,0.425184304693362,3.58365966669054));
#35107=CARTESIAN_POINT('Ctrl Pts',(13.2250616388154,0.563010194007583,3.72441327672633));
#35108=CARTESIAN_POINT('Ctrl Pts',(13.240966917503,0.624000679506934,3.94040408926733));
#35109=CARTESIAN_POINT('Ctrl Pts',(13.2568721961906,0.580151510544767,4.13245826101242));
#35110=CARTESIAN_POINT('Ctrl Pts',(13.2727774748782,0.536302341582597,4.32451243275751));
#35111=CARTESIAN_POINT('Ctrl Pts',(13.2886827535658,0.387613518158899,4.49262996370669));
#35112=CARTESIAN_POINT('Ctrl Pts',(13.3045880322534,0.202356657484476,4.55961839611428));
#35113=CARTESIAN_POINT('Ctrl Pts',(13.3101102177498,0.13803695776657,4.58287624384712));
#35114=CARTESIAN_POINT('Ctrl Pts',(13.3156324032461,0.0693092633201986,
4.59394375907155));
#35115=CARTESIAN_POINT('Ctrl Pts',(13.3211545887425,0.000436239896754628,
4.59347700091179));
#35116=CARTESIAN_POINT('Origin',(4.,0.,4.));
#35117=CARTESIAN_POINT('',(13.7288454112576,-0.000361622974213827,4.59480268714608));
#35118=CARTESIAN_POINT('',(13.6211545887425,-0.000396530615921017,4.59339874939382));
#35119=CARTESIAN_POINT('',(4.,-7.27562663373442E-17,4.5941));
#35120=CARTESIAN_POINT('Ctrl Pts',(13.7288454112576,-0.000361622974213827,
4.59480268714608));
#35121=CARTESIAN_POINT('Ctrl Pts',(13.714655378171,0.175608319374377,4.59354294412002));
#35122=CARTESIAN_POINT('Ctrl Pts',(13.7004653450845,0.352610168065205,4.51056419690263));
#35123=CARTESIAN_POINT('Ctrl Pts',(13.6862753119979,0.463013835099274,4.37381700684221));
#35124=CARTESIAN_POINT('Ctrl Pts',(13.6703700333103,0.586762742631886,4.22054025587244));
#35125=CARTESIAN_POINT('Ctrl Pts',(13.6544647546227,0.626840040937572,3.99971072753873));
#35126=CARTESIAN_POINT('Ctrl Pts',(13.6385594759351,0.564843930165024,3.81272399872504));
#35127=CARTESIAN_POINT('Ctrl Pts',(13.6226541972475,0.502847819392478,3.62573726991136));
#35128=CARTESIAN_POINT('Ctrl Pts',(13.6067489185599,0.338778299541704,3.4725933406177));
#35129=CARTESIAN_POINT('Ctrl Pts',(13.5908436398723,0.147969152919217,3.42360942419035));
#35130=CARTESIAN_POINT('Ctrl Pts',(13.5749383611846,-0.0428399937032757,
3.37462550776301));
#35131=CARTESIAN_POINT('Ctrl Pts',(13.559033082497,-0.260388767097474,3.42980160420198));
#35132=CARTESIAN_POINT('Ctrl Pts',(13.5431278038094,-0.404787974250376,
3.56380318433064));
#35133=CARTESIAN_POINT('Ctrl Pts',(13.5272225251218,-0.549187181403275,
3.6978047644593));
#35134=CARTESIAN_POINT('Ctrl Pts',(13.5113172464342,-0.620436822314871,
3.91063182827765));
#35135=CARTESIAN_POINT('Ctrl Pts',(13.4954119677466,-0.585822076202281,
4.10456319205082));
#35136=CARTESIAN_POINT('Ctrl Pts',(13.479506689059,-0.551207330089691,4.298494555824));
#35137=CARTESIAN_POINT('Ctrl Pts',(13.4636014103714,-0.410728196952908,
4.47353021955202));
#35138=CARTESIAN_POINT('Ctrl Pts',(13.4476961316837,-0.228886751546343,
4.54930121159921));
#35139=CARTESIAN_POINT('Ctrl Pts',(13.4414125582084,-0.15704808052867,4.57923546205676));
#35140=CARTESIAN_POINT('Ctrl Pts',(13.435128984733,-0.0787538239969463,
4.5936770685736));
#35141=CARTESIAN_POINT('Ctrl Pts',(13.4288454112576,-0.000323145728561625,
4.59329116515504));
#35142=CARTESIAN_POINT('Ctrl Pts',(13.3211545887425,0.000436239896754628,
4.59347700091179));
#35143=CARTESIAN_POINT('Ctrl Pts',(13.3315376819337,-0.129062311182503,
4.59259937855127));
#35144=CARTESIAN_POINT('Ctrl Pts',(13.341920775125,-0.259074650003773,4.55094414667863));
#35145=CARTESIAN_POINT('Ctrl Pts',(13.3523038683163,-0.361265427801182,
4.47287234722855));
#35146=CARTESIAN_POINT('Ctrl Pts',(13.3682091470039,-0.517805754487323,
4.35327853206923));
#35147=CARTESIAN_POINT('Ctrl Pts',(13.3841144256915,-0.609061509934468,
4.14823156788458));
#35148=CARTESIAN_POINT('Ctrl Pts',(13.4000197043791,-0.593131911953917,
3.95188034580653));
#35149=CARTESIAN_POINT('Ctrl Pts',(13.4159249830667,-0.577202313973367,
3.75552912372848));
#35150=CARTESIAN_POINT('Ctrl Pts',(13.4318302617543,-0.454087362565127,
3.56787364375704));
#35151=CARTESIAN_POINT('Ctrl Pts',(13.4477355404419,-0.280316234851803,
3.47507736324643));
#35152=CARTESIAN_POINT('Ctrl Pts',(13.4636408191295,-0.106545107138479,
3.38228108273583));
#35153=CARTESIAN_POINT('Ctrl Pts',(13.4795460978172,0.117882196879929,3.38434400168606));
#35154=CARTESIAN_POINT('Ctrl Pts',(13.4954513765048,0.2899181539344,3.48031891499009));
#35155=CARTESIAN_POINT('Ctrl Pts',(13.5113566551924,0.461954110988876,3.57629382829412));
#35156=CARTESIAN_POINT('Ctrl Pts',(13.52726193388,0.581598721079409,3.76618073595195));
#35157=CARTESIAN_POINT('Ctrl Pts',(13.5431672125676,0.593916240998451,3.96279160341967));
#35158=CARTESIAN_POINT('Ctrl Pts',(13.5590724912552,0.606233760917493,4.15940247088739));
#35159=CARTESIAN_POINT('Ctrl Pts',(13.5749777699428,0.511224190665043,4.362737298165));
#35160=CARTESIAN_POINT('Ctrl Pts',(13.5908830486304,0.352511905377589,4.47943333495374));
#35161=CARTESIAN_POINT('Ctrl Pts',(13.6009735620011,0.251822790258117,4.55346680161908));
#35162=CARTESIAN_POINT('Ctrl Pts',(13.6110640753718,0.125494626822297,4.59262991567553));
#35163=CARTESIAN_POINT('Ctrl Pts',(13.6211545887425,-0.000396530615921017,
4.59339874939382));
#35164=CARTESIAN_POINT('Origin',(4.,0.,4.));
#35165=CARTESIAN_POINT('',(14.0288454112576,0.000507412974116619,4.59441995931617));
#35166=CARTESIAN_POINT('',(13.9211545887425,-0.000275297881949146,4.59492513410986));
#35167=CARTESIAN_POINT('',(4.,-7.27562663373442E-17,4.5941));
#35168=CARTESIAN_POINT('Ctrl Pts',(14.0288454112576,0.000507412974116619,
4.59441995931617));
#35169=CARTESIAN_POINT('Ctrl Pts',(14.0259923289843,0.0359476882196221,
4.59474138052009));
#35170=CARTESIAN_POINT('Ctrl Pts',(14.0231392467111,0.0713355155074759,
4.59184535342408));
#35171=CARTESIAN_POINT('Ctrl Pts',(14.0202861644378,0.106106362061302,4.58554453803953));
#35172=CARTESIAN_POINT('Ctrl Pts',(14.0043808857502,0.299945849210873,4.55041893875697));
#35173=CARTESIAN_POINT('Ctrl Pts',(13.9884756070626,0.474610768799237,4.40947910659883));
#35174=CARTESIAN_POINT('Ctrl Pts',(13.972570328375,0.549902379214768,4.22743864981956));
#35175=CARTESIAN_POINT('Ctrl Pts',(13.9566650496873,0.625193989630293,4.04539819304031));
#35176=CARTESIAN_POINT('Ctrl Pts',(13.9407597709997,0.601112290873006,3.82225711163994));
#35177=CARTESIAN_POINT('Ctrl Pts',(13.9248544923121,0.488714580199595,3.66047234987686));
#35178=CARTESIAN_POINT('Ctrl Pts',(13.9089492136245,0.376316869526181,3.49868758811377));
#35179=CARTESIAN_POINT('Ctrl Pts',(13.8930439349369,0.175603146936639,3.39825914598798));
#35180=CARTESIAN_POINT('Ctrl Pts',(13.8771386562493,-0.0212673376532481,
3.40529951534663));
#35181=CARTESIAN_POINT('Ctrl Pts',(13.8612333775617,-0.218137822243141,
3.41233988470529));
#35182=CARTESIAN_POINT('Ctrl Pts',(13.8453280988741,-0.411165068833379,
3.52684906554841));
#35183=CARTESIAN_POINT('Ctrl Pts',(13.8294228201864,-0.511719132099071,
3.69624928651676));
#35184=CARTESIAN_POINT('Ctrl Pts',(13.8135175414988,-0.612273195364761,
3.8656495074851));
#35185=CARTESIAN_POINT('Ctrl Pts',(13.7976122628112,-0.62035407530591,4.08994076857866));
#35186=CARTESIAN_POINT('Ctrl Pts',(13.7817069841236,-0.532251373727382,
4.26613801168402));
#35187=CARTESIAN_POINT('Ctrl Pts',(13.765801705436,-0.44414867214885,4.44233525478938));
#35188=CARTESIAN_POINT('Ctrl Pts',(13.7498964267484,-0.259862389050636,
4.57043847990653));
#35189=CARTESIAN_POINT('Ctrl Pts',(13.7339911480608,-0.0640089891217576,
4.59162810566218));
#35190=CARTESIAN_POINT('Ctrl Pts',(13.7322759024597,-0.0428879079209441,
4.59391322201126));
#35191=CARTESIAN_POINT('Ctrl Pts',(13.7305606568586,-0.0216323041412813,
4.594954960835));
#35192=CARTESIAN_POINT('Ctrl Pts',(13.7288454112576,-0.000361622974213827,
4.59480268714608));
#35193=CARTESIAN_POINT('Ctrl Pts',(13.6211545887425,-0.000396530615921017,
4.59339874939382));
#35194=CARTESIAN_POINT('Ctrl Pts',(13.6269693540594,-0.0729426448807452,
4.59384179797573));
#35195=CARTESIAN_POINT('Ctrl Pts',(13.6327841193764,-0.145343639818557,
4.58153501668255));
#35196=CARTESIAN_POINT('Ctrl Pts',(13.6385988846933,-0.212609537044371,
4.5558040579697));
#35197=CARTESIAN_POINT('Ctrl Pts',(13.6545041633809,-0.396603693856438,
4.48542149789704));
#35198=CARTESIAN_POINT('Ctrl Pts',(13.6704094420685,-0.542177007158105,
4.31459913145184));
#35199=CARTESIAN_POINT('Ctrl Pts',(13.6863147207561,-0.582488370180261,
4.12177136240739));
#35200=CARTESIAN_POINT('Ctrl Pts',(13.7022199994437,-0.622799733202417,
3.92894359336294));
#35201=CARTESIAN_POINT('Ctrl Pts',(13.7181252781313,-0.557849145945042,
3.71411042171923));
#35202=CARTESIAN_POINT('Ctrl Pts',(13.734030556819,-0.417459170243993,3.57591415105311));
#35203=CARTESIAN_POINT('Ctrl Pts',(13.7499358355066,-0.277069194542941,
3.43771788038699));
#35204=CARTESIAN_POINT('Ctrl Pts',(13.7658411141942,-0.0612398303982075,
3.37615851069845));
#35205=CARTESIAN_POINT('Ctrl Pts',(13.7817463928818,0.130929209162332,3.41950150018632));
#35206=CARTESIAN_POINT('Ctrl Pts',(13.7976516715694,0.323098248722867,3.46284448967418));
#35207=CARTESIAN_POINT('Ctrl Pts',(13.813556950257,0.491606963699209,3.61108983833845));
#35208=CARTESIAN_POINT('Ctrl Pts',(13.8294622289446,0.559083281190044,3.79616955381596));
#35209=CARTESIAN_POINT('Ctrl Pts',(13.8453675076322,0.62655959868088,3.98124926929349));
#35210=CARTESIAN_POINT('Ctrl Pts',(13.8612727863198,0.593003518686204,4.20316335158427));
#35211=CARTESIAN_POINT('Ctrl Pts',(13.8771780650075,0.4738225734989,4.36001824251097));
#35212=CARTESIAN_POINT('Ctrl Pts',(13.8918369062525,0.363981395029584,4.50458099992985));
#35213=CARTESIAN_POINT('Ctrl Pts',(13.9064957474975,0.181409709145346,4.59388191268165));
#35214=CARTESIAN_POINT('Ctrl Pts',(13.9211545887425,-0.000275297881949146,
4.59492513410986));
#35215=CARTESIAN_POINT('Origin',(4.,0.,4.));
#35216=CARTESIAN_POINT('',(14.3288454112576,0.000109044058801022,4.5931342436645));
#35217=CARTESIAN_POINT('',(14.2211545887425,0.000537210645871958,4.59424369460725));
#35218=CARTESIAN_POINT('',(4.,-7.27562663373442E-17,4.5941));
#35219=CARTESIAN_POINT('Ctrl Pts',(14.3288454112576,0.000109044058801022,
4.5931342436645));
#35220=CARTESIAN_POINT('Ctrl Pts',(14.32142400111,0.0928032711674493,4.59328573107644));
#35221=CARTESIAN_POINT('Ctrl Pts',(14.3140025909624,0.185434358886594,4.57287353691408));
#35222=CARTESIAN_POINT('Ctrl Pts',(14.3065811808148,0.267539471941071,4.53154830171049));
#35223=CARTESIAN_POINT('Ctrl Pts',(14.2906759021272,0.443503969097433,4.44298165875801));
#35224=CARTESIAN_POINT('Ctrl Pts',(14.2747706234396,0.571121189235106,4.25835848700565));
#35225=CARTESIAN_POINT('Ctrl Pts',(14.258865344752,0.591794703906212,4.06244993615984));
#35226=CARTESIAN_POINT('Ctrl Pts',(14.2429600660644,0.612468218577319,3.86654138531401));
#35227=CARTESIAN_POINT('Ctrl Pts',(14.2270547873768,0.526198027781844,3.65934745537473));
#35228=CARTESIAN_POINT('Ctrl Pts',(14.2111495086891,0.372595753342289,3.53600283331781));
#35229=CARTESIAN_POINT('Ctrl Pts',(14.1952442300015,0.218993478902743,3.4126582112609));
#35230=CARTESIAN_POINT('Ctrl Pts',(14.1793389513139,-0.00194087918087354,
3.37316289708635));
#35231=CARTESIAN_POINT('Ctrl Pts',(14.1634336726263,-0.18876361063844,3.43565146815417));
#35232=CARTESIAN_POINT('Ctrl Pts',(14.1475283939387,-0.375586342096006,
3.49814003922198));
#35233=CARTESIAN_POINT('Ctrl Pts',(14.1316231152511,-0.528297446927522,
3.66261249553216));
#35234=CARTESIAN_POINT('Ctrl Pts',(14.1157178365635,-0.576778446468407,
3.85355004340287));
#35235=CARTESIAN_POINT('Ctrl Pts',(14.0998125578759,-0.625259446009293,
4.04448759127359));
#35236=CARTESIAN_POINT('Ctrl Pts',(14.0839072791882,-0.569510340259543,
4.26189023070484));
#35237=CARTESIAN_POINT('Ctrl Pts',(14.0680020005006,-0.435128760029281,
4.40593586721696));
#35238=CARTESIAN_POINT('Ctrl Pts',(14.0549498040863,-0.324852491748397,
4.52414265738481));
#35239=CARTESIAN_POINT('Ctrl Pts',(14.0418976076719,-0.161623710204441,
4.5929495310973));
#35240=CARTESIAN_POINT('Ctrl Pts',(14.0288454112576,0.000507412974116619,
4.59441995931617));
#35241=CARTESIAN_POINT('Ctrl Pts',(13.9211545887425,-0.000275297881949146,
4.59492513410986));
#35242=CARTESIAN_POINT('Ctrl Pts',(13.9224010261851,-0.015723926578741,
4.59501383895544));
#35243=CARTESIAN_POINT('Ctrl Pts',(13.9236474636277,-0.0311661445373128,
4.59446443570748));
#35244=CARTESIAN_POINT('Ctrl Pts',(13.9248939010703,-0.0465566941337027,
4.59325663951544));
#35245=CARTESIAN_POINT('Ctrl Pts',(13.9407991797579,-0.242949206199084,
4.5778444460306));
#35246=CARTESIAN_POINT('Ctrl Pts',(13.9567044584455,-0.430928419949921,
4.4552243594983));
#35247=CARTESIAN_POINT('Ctrl Pts',(13.9726097371331,-0.524182233176515,
4.28169833602613));
#35248=CARTESIAN_POINT('Ctrl Pts',(13.9885150158207,-0.617436046403107,
4.10817231255396));
#35249=CARTESIAN_POINT('Ctrl Pts',(14.0044202945084,-0.615964459105464,
3.88374035214192));
#35250=CARTESIAN_POINT('Ctrl Pts',(14.020325573196,-0.52044316191294,3.71145211607799));
#35251=CARTESIAN_POINT('Ctrl Pts',(14.0362308518836,-0.424921864720413,
3.53916388001405));
#35252=CARTESIAN_POINT('Ctrl Pts',(14.0521361305712,-0.235350857633014,
3.41901936829824));
#35253=CARTESIAN_POINT('Ctrl Pts',(14.0680414092588,-0.0387731270173405,
3.40618385781531));
#35254=CARTESIAN_POINT('Ctrl Pts',(14.0839466879464,0.157804603598333,3.39334834733239));
#35255=CARTESIAN_POINT('Ctrl Pts',(14.0998519666341,0.361389057742269,3.48782183808236));
#35256=CARTESIAN_POINT('Ctrl Pts',(14.1157572453217,0.478502867019537,3.64622609995664));
#35257=CARTESIAN_POINT('Ctrl Pts',(14.1316625240093,0.595616676296804,3.80463036183091));
#35258=CARTESIAN_POINT('Ctrl Pts',(14.1475678026969,0.626259840707404,4.02696539482948));
#35259=CARTESIAN_POINT('Ctrl Pts',(14.1634730813845,0.556362315559365,4.21114435801894));
#35260=CARTESIAN_POINT('Ctrl Pts',(14.1793783600721,0.486464790411328,4.3953233212084));
#35261=CARTESIAN_POINT('Ctrl Pts',(14.1952836387597,0.316026575704654,4.54134621458875));
#35262=CARTESIAN_POINT('Ctrl Pts',(14.2111889174473,0.123305688986428,4.58216550323889));
#35263=CARTESIAN_POINT('Ctrl Pts',(14.2145108078791,0.0830550475387342,
4.59069079896363));
#35264=CARTESIAN_POINT('Ctrl Pts',(14.2178326983108,0.0418324306113591,
4.59462708830176));
#35265=CARTESIAN_POINT('Ctrl Pts',(14.2211545887425,0.000537210645871958,
4.59424369460725));
#35266=CARTESIAN_POINT('Origin',(4.,0.,4.));
#35267=CARTESIAN_POINT('',(14.6288454112575,-0.000548182068839831,4.59401855345973));
#35268=CARTESIAN_POINT('',(14.5211545887425,1.28950532977596E-5,4.59311636453746));
#35269=CARTESIAN_POINT('',(4.,-7.27562663373442E-17,4.5941));
#35270=CARTESIAN_POINT('Ctrl Pts',(14.6288454112575,-0.000548182068839831,
4.59401855345973));
#35271=CARTESIAN_POINT('Ctrl Pts',(14.6168556732357,0.148643716013534,4.59265593252186));
#35272=CARTESIAN_POINT('Ctrl Pts',(14.6048659352138,0.29876355451001,4.53564313143304));
#35273=CARTESIAN_POINT('Ctrl Pts',(14.5928761971919,0.407080942069735,4.43405768361063));
#35274=CARTESIAN_POINT('Ctrl Pts',(14.5769709185042,0.55077200793829,4.29929703619113));
#35275=CARTESIAN_POINT('Ctrl Pts',(14.5610656398166,0.620899143473568,4.08609746938767));
#35276=CARTESIAN_POINT('Ctrl Pts',(14.545160361129,0.585262934872208,3.89235120454656));
#35277=CARTESIAN_POINT('Ctrl Pts',(14.5292550824414,0.549626726270847,3.69860493970543));
#35278=CARTESIAN_POINT('Ctrl Pts',(14.5133498037538,0.408227173532835,3.52431197682665));
#35279=CARTESIAN_POINT('Ctrl Pts',(14.4974445250662,0.225988969153725,3.44950027073699));
#35280=CARTESIAN_POINT('Ctrl Pts',(14.4815392463786,0.04375076477463,3.37468856464734));
#35281=CARTESIAN_POINT('Ctrl Pts',(14.465633967691,-0.179326091245555,3.39935811534679));
#35282=CARTESIAN_POINT('Ctrl Pts',(14.4497286890033,-0.340814144225853,
3.51218170883678));
#35283=CARTESIAN_POINT('Ctrl Pts',(14.4338234103157,-0.50230219720616,3.62500530232677));
#35284=CARTESIAN_POINT('Ctrl Pts',(14.4179181316281,-0.602201447146573,
3.82598293860731));
#35285=CARTESIAN_POINT('Ctrl Pts',(14.4020128529405,-0.594642384863179,
4.02283418976097));
#35286=CARTESIAN_POINT('Ctrl Pts',(14.3861075742529,-0.587083322579785,
4.21968544091462));
#35287=CARTESIAN_POINT('Ctrl Pts',(14.3702022955653,-0.47206594807259,4.4124103069414));
#35288=CARTESIAN_POINT('Ctrl Pts',(14.3542970168777,-0.302401373731467,
4.51251768287848));
#35289=CARTESIAN_POINT('Ctrl Pts',(14.3458131483376,-0.211902365642262,
4.565914912441));
#35290=CARTESIAN_POINT('Ctrl Pts',(14.3373292797976,-0.10585540495725,4.59296106912451));
#35291=CARTESIAN_POINT('Ctrl Pts',(14.3288454112576,0.000109044058801022,
4.5931342436645));
#35292=CARTESIAN_POINT('Ctrl Pts',(14.2211545887425,0.000537210645871958,
4.59424369460725));
#35293=CARTESIAN_POINT('Ctrl Pts',(14.2337379769984,-0.155889919212927,
4.59279139152499));
#35294=CARTESIAN_POINT('Ctrl Pts',(14.2463213652543,-0.313358837143528,
4.52935553548989));
#35295=CARTESIAN_POINT('Ctrl Pts',(14.2589047535102,-0.422984449084643,
4.4185751090669));
#35296=CARTESIAN_POINT('Ctrl Pts',(14.2748100321978,-0.561550141707708,
4.27854974232482));
#35297=CARTESIAN_POINT('Ctrl Pts',(14.2907153108854,-0.623677968224056,
4.06288332492072));
#35298=CARTESIAN_POINT('Ctrl Pts',(14.306620589573,-0.580841459108965,3.87060075163287));
#35299=CARTESIAN_POINT('Ctrl Pts',(14.3225258682606,-0.538004949993874,
3.67831817834502));
#35300=CARTESIAN_POINT('Ctrl Pts',(14.3384311469482,-0.390204105247342,
3.50941944917344));
#35301=CARTESIAN_POINT('Ctrl Pts',(14.3543364256359,-0.205302819838896,
3.44145571503774));
#35302=CARTESIAN_POINT('Ctrl Pts',(14.3702417043235,-0.0204015344304391,
3.37349198090203));
#35303=CARTESIAN_POINT('Ctrl Pts',(14.3861469830111,0.201600191639931,3.40646324180223));
#35304=CARTESIAN_POINT('Ctrl Pts',(14.4020522616987,0.358768557879186,3.52523048963197));
#35305=CARTESIAN_POINT('Ctrl Pts',(14.4179575403863,0.515936924118427,3.6439977374617));
#35306=CARTESIAN_POINT('Ctrl Pts',(14.4338628190739,0.608271930526566,3.84856097222098));
#35307=CARTESIAN_POINT('Ctrl Pts',(14.4497680977615,0.59337724853295,4.04499341086509));
#35308=CARTESIAN_POINT('Ctrl Pts',(14.4656733764491,0.578482566539332,4.2414258495092));
#35309=CARTESIAN_POINT('Ctrl Pts',(14.4815786551367,0.456358196143958,4.42972749203816));
#35310=CARTESIAN_POINT('Ctrl Pts',(14.4974839338244,0.283078481576349,4.52343819058819));
#35311=CARTESIAN_POINT('Ctrl Pts',(14.5053741521304,0.197118668938093,4.56992576768087));
#35312=CARTESIAN_POINT('Ctrl Pts',(14.5132643704364,0.0985699939877532,
4.59313537862966));
#35313=CARTESIAN_POINT('Ctrl Pts',(14.5211545887425,1.28950532977596E-5,
4.59311636453746));
#35314=CARTESIAN_POINT('Origin',(4.,0.,4.));
#35315=CARTESIAN_POINT('',(14.9288454112575,0.000149915246051877,4.59503491979621));
#35316=CARTESIAN_POINT('',(14.8211545887425,-0.000542004001680995,4.59419620878869));
#35317=CARTESIAN_POINT('',(4.,-7.27562663373442E-17,4.5941));
#35318=CARTESIAN_POINT('Ctrl Pts',(14.9288454112575,0.000149915246051877,
4.59503491979621));
#35319=CARTESIAN_POINT('Ctrl Pts',(14.9281926240489,0.00823674021970066,
4.59506221957623));
#35320=CARTESIAN_POINT('Ctrl Pts',(14.9275398368403,0.0163225255999611,
4.59491168338633));
#35321=CARTESIAN_POINT('Ctrl Pts',(14.9268870496317,0.0244008833477238,
4.59458015690877));
#35322=CARTESIAN_POINT('Ctrl Pts',(14.9109817709441,0.221231534471853,4.58650245417764));
#35323=CARTESIAN_POINT('Ctrl Pts',(14.8950764922565,0.413652681988333,4.47097768448731));
#35324=CARTESIAN_POINT('Ctrl Pts',(14.8791712135689,0.513312675625014,4.30104993462962));
#35325=CARTESIAN_POINT('Ctrl Pts',(14.8632659348813,0.612972669261697,4.13112218477192));
#35326=CARTESIAN_POINT('Ctrl Pts',(14.8473606561937,0.619871509018575,3.90679145474687));
#35327=CARTESIAN_POINT('Ctrl Pts',(14.831455377506,0.530841539545133,3.73106092513143));
#35328=CARTESIAN_POINT('Ctrl Pts',(14.8155500988184,0.441811570071688,3.55533039551599));
#35329=CARTESIAN_POINT('Ctrl Pts',(14.7996448201308,0.256852791367914,3.42820006631018));
#35330=CARTESIAN_POINT('Ctrl Pts',(14.7837395414432,0.0608904496539635,
3.40804280624462));
#35331=CARTESIAN_POINT('Ctrl Pts',(14.7678342627556,-0.135071892059981,
3.38788554617906));
#35332=CARTESIAN_POINT('Ctrl Pts',(14.751928984068,-0.342037796784102,3.47470135525375));
#35333=CARTESIAN_POINT('Ctrl Pts',(14.7360237053804,-0.464977277074429,
3.62862808681558));
#35334=CARTESIAN_POINT('Ctrl Pts',(14.7201184266927,-0.587916757364756,
3.78255481837741));
#35335=CARTESIAN_POINT('Ctrl Pts',(14.7042131480052,-0.62682981322129,4.00359247242638));
#35336=CARTESIAN_POINT('Ctrl Pts',(14.6883078693175,-0.56384921567034,4.19024990955517));
#35337=CARTESIAN_POINT('Ctrl Pts',(14.6724025906299,-0.500868618119389,
4.37690734668397));
#35338=CARTESIAN_POINT('Ctrl Pts',(14.6564973119423,-0.335994367160947,
4.52918456689258));
#35339=CARTESIAN_POINT('Ctrl Pts',(14.6405920332547,-0.144929743580805,
4.57716231297912));
#35340=CARTESIAN_POINT('Ctrl Pts',(14.636676492589,-0.097893704910838,4.5889734116427));
#35341=CARTESIAN_POINT('Ctrl Pts',(14.6327609519233,-0.0492704262804658,
4.59446355048005));
#35342=CARTESIAN_POINT('Ctrl Pts',(14.6288454112575,-0.000548182068839831,
4.59401855345973));
#35343=CARTESIAN_POINT('Ctrl Pts',(14.5211545887425,1.28950532977596E-5,
4.59311636453746));
#35344=CARTESIAN_POINT('Ctrl Pts',(14.5291696491241,-0.100103612291989,
4.59309704959697));
#35345=CARTESIAN_POINT('Ctrl Pts',(14.5371847095056,-0.200228812305367,
4.56910822985942));
#35346=CARTESIAN_POINT('Ctrl Pts',(14.5451997698872,-0.287175610734119,
4.52120162576233));
#35347=CARTESIAN_POINT('Ctrl Pts',(14.5611050485748,-0.459714929737158,
4.42613460781534));
#35348=CARTESIAN_POINT('Ctrl Pts',(14.5770103272624,-0.580358509003398,
4.23688081735026));
#35349=CARTESIAN_POINT('Ctrl Pts',(14.59291560595,-0.593711920942704,4.04033758828107));
#35350=CARTESIAN_POINT('Ctrl Pts',(14.6088208846377,-0.607065332882009,
3.84379435921188));
#35351=CARTESIAN_POINT('Ctrl Pts',(14.6247261633253,-0.513128577494387,
3.63996169153858));
#35352=CARTESIAN_POINT('Ctrl Pts',(14.6406314420129,-0.35503343871745,3.52243092280774));
#35353=CARTESIAN_POINT('Ctrl Pts',(14.6565367207005,-0.196938299940509,
3.40490015407689));
#35354=CARTESIAN_POINT('Ctrl Pts',(14.6724419993881,0.025315222225754,3.37367128428849));
#35355=CARTESIAN_POINT('Ctrl Pts',(14.6883472780757,0.209677713173688,3.44308328926485));
#35356=CARTESIAN_POINT('Ctrl Pts',(14.7042525567633,0.394040204121622,3.51249529424121));
#35357=CARTESIAN_POINT('Ctrl Pts',(14.720157835451,0.540511663851219,3.68254817398232));
#35358=CARTESIAN_POINT('Ctrl Pts',(14.7360631141386,0.581838594751101,3.87516084045512));
#35359=CARTESIAN_POINT('Ctrl Pts',(14.7519683928262,0.623165525650983,4.06777350692792));
#35360=CARTESIAN_POINT('Ctrl Pts',(14.7678736715138,0.559347927721136,4.2829459601324));
#35361=CARTESIAN_POINT('Ctrl Pts',(14.7837789502014,0.419688142031033,4.42188011275284));
#35362=CARTESIAN_POINT('Ctrl Pts',(14.7962374963817,0.310293146587505,4.53070672248707));
#35363=CARTESIAN_POINT('Ctrl Pts',(14.8086960425621,0.154364940471616,4.59275708529138));
#35364=CARTESIAN_POINT('Ctrl Pts',(14.8211545887425,-0.000542004001680995,
4.59419620878869));
#35365=CARTESIAN_POINT('Origin',(4.,0.,4.));
#35366=CARTESIAN_POINT('',(15.2288454112576,0.000471544078774977,4.59356550157774));
#35367=CARTESIAN_POINT('',(15.1211545887425,0.000250233060073018,4.59495282954609));
#35368=CARTESIAN_POINT('',(4.,-7.27562663373442E-17,4.5941));
#35369=CARTESIAN_POINT('Ctrl Pts',(15.2288454112576,0.000471544078774977,
4.59356550157774));
#35370=CARTESIAN_POINT('Ctrl Pts',(15.2236242961746,0.0655651715058866,
4.59404721416646));
#35371=CARTESIAN_POINT('Ctrl Pts',(15.2184031810917,0.130516835945995,4.58418155789741));
#35372=CARTESIAN_POINT('Ctrl Pts',(15.2131820660088,0.191734887706884,4.56334598510492));
#35373=CARTESIAN_POINT('Ctrl Pts',(15.1972767873211,0.378225734681762,4.49987379829874));
#35374=CARTESIAN_POINT('Ctrl Pts',(15.1813715086335,0.530068013118856,4.33459889729257));
#35375=CARTESIAN_POINT('Ctrl Pts',(15.1654662299459,0.577542172676889,4.143408524424));
#35376=CARTESIAN_POINT('Ctrl Pts',(15.1495609512583,0.625016332234921,3.95221815155542));
#35377=CARTESIAN_POINT('Ctrl Pts',(15.1336556725707,0.568122372913892,3.73511230682445));
#35378=CARTESIAN_POINT('Ctrl Pts',(15.1177503938831,0.432983593849097,3.59177680914072));
#35379=CARTESIAN_POINT('Ctrl Pts',(15.1018451151955,0.297844814784303,3.44844131145699));
#35380=CARTESIAN_POINT('Ctrl Pts',(15.0859398365078,0.0844612159757424,
3.37887616082051));
#35381=CARTESIAN_POINT('Ctrl Pts',(15.0700345578202,-0.109190481519281,
3.41502273134472));
#35382=CARTESIAN_POINT('Ctrl Pts',(15.0541292791326,-0.302842179014298,
3.45116930186893));
#35383=CARTESIAN_POINT('Ctrl Pts',(15.038224000445,-0.47676197519578,3.59302759355383));
#35384=CARTESIAN_POINT('Ctrl Pts',(15.0223187217574,-0.551093257596978,
3.77546228038711));
#35385=CARTESIAN_POINT('Ctrl Pts',(15.0064134430698,-0.625424539998176,
3.95789696722038));
#35386=CARTESIAN_POINT('Ctrl Pts',(14.9905081643822,-0.600167308619091,
4.18090804920204));
#35387=CARTESIAN_POINT('Ctrl Pts',(14.9746028856946,-0.486918615563658,
4.34209827230691));
#35388=CARTESIAN_POINT('Ctrl Pts',(14.9593503942156,-0.378317895025423,
4.49667289829699));
#35389=CARTESIAN_POINT('Ctrl Pts',(14.9440979027365,-0.188800216398263,
4.59439705548643));
#35390=CARTESIAN_POINT('Ctrl Pts',(14.9288454112575,0.000149915246051877,
4.59503491979621));
#35391=CARTESIAN_POINT('Ctrl Pts',(14.8211545887425,-0.000542004001680995,
4.59419620878869));
#35392=CARTESIAN_POINT('Ctrl Pts',(14.8246013212497,-0.0433979515083632,
4.5945943510493));
#35393=CARTESIAN_POINT('Ctrl Pts',(14.828048053757,-0.0861757330942537,
4.59035339483295));
#35394=CARTESIAN_POINT('Ctrl Pts',(14.8314947862642,-0.127868389248254,
4.58118038604969));
#35395=CARTESIAN_POINT('Ctrl Pts',(14.8474000649518,-0.320263161387096,
4.5388506546897));
#35396=CARTESIAN_POINT('Ctrl Pts',(14.8633053436395,-0.489550732214419,
4.39149533993331));
#35397=CARTESIAN_POINT('Ctrl Pts',(14.8792106223271,-0.558001411172811,
4.20677376822741));
#35398=CARTESIAN_POINT('Ctrl Pts',(14.8951159010147,-0.6264520901312,4.0220521965215));
#35399=CARTESIAN_POINT('Ctrl Pts',(14.9110211797023,-0.594065877220663,
3.79996436786608));
#35400=CARTESIAN_POINT('Ctrl Pts',(14.9269264583899,-0.475713151262041,
3.64248361741852));
#35401=CARTESIAN_POINT('Ctrl Pts',(14.9428317370775,-0.357360425303418,
3.48500286697096));
#35402=CARTESIAN_POINT('Ctrl Pts',(14.9587370157651,-0.153041186296697,
3.39212919473125));
#35403=CARTESIAN_POINT('Ctrl Pts',(14.9746422944528,0.0434298152403689,
3.40650626183085));
#35404=CARTESIAN_POINT('Ctrl Pts',(14.9905475731404,0.239900816777435,3.42088332893044));
#35405=CARTESIAN_POINT('Ctrl Pts',(15.006452851828,0.428523580844854,3.54251113536931));
#35406=CARTESIAN_POINT('Ctrl Pts',(15.0223581305156,0.522690514153935,3.71554333807889));
#35407=CARTESIAN_POINT('Ctrl Pts',(15.0382634092032,0.616857447463019,3.88857554078846));
#35408=CARTESIAN_POINT('Ctrl Pts',(15.0541686878908,0.616568550013756,4.11301213976874));
#35409=CARTESIAN_POINT('Ctrl Pts',(15.0700739665784,0.521956471292605,4.28580134389743));
#35410=CARTESIAN_POINT('Ctrl Pts',(15.085979245266,0.427344392571456,4.45859054802613));
#35411=CARTESIAN_POINT('Ctrl Pts',(15.1018845239536,0.238409132578427,4.57973235730324));
#35412=CARTESIAN_POINT('Ctrl Pts',(15.1177898026413,0.0419017695106382,
4.59360357799603));
#35413=CARTESIAN_POINT('Ctrl Pts',(15.1189113980083,0.0280446248267054,
4.59458173733358));
#35414=CARTESIAN_POINT('Ctrl Pts',(15.1200329933754,0.0141498265549413,
4.59502647517791));
#35415=CARTESIAN_POINT('Ctrl Pts',(15.1211545887425,0.000250233060073018,
4.59495282954609));
#35416=CARTESIAN_POINT('Origin',(4.,0.,4.));
#35417=CARTESIAN_POINT('',(15.5288454112575,-0.000350670266729247,4.59332700645389));
#35418=CARTESIAN_POINT('',(15.4211545887425,0.000414092275955974,4.59343115273787));
#35419=CARTESIAN_POINT('',(4.,-7.27562663373442E-17,4.5941));
#35420=CARTESIAN_POINT('Ctrl Pts',(15.5288454112575,-0.000350670266729247,
4.59332700645389));
#35421=CARTESIAN_POINT('Ctrl Pts',(15.5190559683003,0.121821298278883,4.59267222728074));
#35422=CARTESIAN_POINT('Ctrl Pts',(15.509266525343,0.244354036528086,4.55597946496206));
#35423=CARTESIAN_POINT('Ctrl Pts',(15.4994770823858,0.343380025451582,4.48601555964668));
#35424=CARTESIAN_POINT('Ctrl Pts',(15.4835718036982,0.504271299656008,4.37234255322809));
#35425=CARTESIAN_POINT('Ctrl Pts',(15.4676665250105,0.603110088323456,4.17084127710728));
#35426=CARTESIAN_POINT('Ctrl Pts',(15.4517612463229,0.594513801222153,3.97403259246294));
#35427=CARTESIAN_POINT('Ctrl Pts',(15.4358559676353,0.58591751412085,3.7772239078186));
#35428=CARTESIAN_POINT('Ctrl Pts',(15.4199506889477,0.469886151250777,3.58510781465072));
#35429=CARTESIAN_POINT('Ctrl Pts',(15.4040454102601,0.299696405559752,3.48589589518039));
#35430=CARTESIAN_POINT('Ctrl Pts',(15.3881401315725,0.129506659868722,3.38668397571006));
#35431=CARTESIAN_POINT('Ctrl Pts',(15.3722348528849,-0.0948414686432761,
3.38037622993726));
#35432=CARTESIAN_POINT('Ctrl Pts',(15.3563295741973,-0.270336810750117,
3.46986890786216));
#35433=CARTESIAN_POINT('Ctrl Pts',(15.3404242955096,-0.445832152856957,
3.55936158578705));
#35434=CARTESIAN_POINT('Ctrl Pts',(15.324519016822,-0.572474708558633,3.74465468740961));
#35435=CARTESIAN_POINT('Ctrl Pts',(15.3086137381344,-0.592115574081638,
3.94066945956945));
#35436=CARTESIAN_POINT('Ctrl Pts',(15.2927084594468,-0.611756439604643,
4.13668423172929));
#35437=CARTESIAN_POINT('Ctrl Pts',(15.2768031807592,-0.524395614948954,
4.3434206744264));
#35438=CARTESIAN_POINT('Ctrl Pts',(15.2608979020716,-0.370145494864779,
4.46595415947185));
#35439=CARTESIAN_POINT('Ctrl Pts',(15.2502137384669,-0.266529987624151,
4.54826443060822));
#35440=CARTESIAN_POINT('Ctrl Pts',(15.2395295748622,-0.13273198696893,4.59257975504152));
#35441=CARTESIAN_POINT('Ctrl Pts',(15.2288454112576,0.000471544078774977,
4.59356550157774));
#35442=CARTESIAN_POINT('Ctrl Pts',(15.1211545887425,0.000250233060073018,
4.59495282954609));
#35443=CARTESIAN_POINT('Ctrl Pts',(15.135938272063,-0.18295950063263,4.59398211075496));
#35444=CARTESIAN_POINT('Ctrl Pts',(15.1507219553836,-0.367002343096231,
4.50294888365168));
#35445=CARTESIAN_POINT('Ctrl Pts',(15.1655056387041,-0.476631971954554,
4.35629051265579));
#35446=CARTESIAN_POINT('Ctrl Pts',(15.1814109173917,-0.594578884209397,
4.19850559451431));
#35447=CARTESIAN_POINT('Ctrl Pts',(15.1973161960793,-0.626393242576541,
3.97633512612291));
#35448=CARTESIAN_POINT('Ctrl Pts',(15.2132214747669,-0.557467239648298,
3.79179038730953));
#35449=CARTESIAN_POINT('Ctrl Pts',(15.2291267534545,-0.488541236720055,
3.60724564849615));
#35450=CARTESIAN_POINT('Ctrl Pts',(15.2450320321422,-0.318874872496425,
3.46032663926078));
#35451=CARTESIAN_POINT('Ctrl Pts',(15.2609373108298,-0.126371763436977,
3.41849235301362));
#35452=CARTESIAN_POINT('Ctrl Pts',(15.2768425895174,0.0661313456224706,
3.37665806676646));
#35453=CARTESIAN_POINT('Ctrl Pts',(15.292747868205,0.281471199517752,3.4399085035075));
#35454=CARTESIAN_POINT('Ctrl Pts',(15.3086531468926,0.420772847618048,3.57920173859056));
#35455=CARTESIAN_POINT('Ctrl Pts',(15.3245584255802,0.560074495718348,3.71849497367363));
#35456=CARTESIAN_POINT('Ctrl Pts',(15.3404637042678,0.623337938023671,3.9338310070987));
#35457=CARTESIAN_POINT('Ctrl Pts',(15.3563689829554,0.581515278282945,4.12633664243329));
#35458=CARTESIAN_POINT('Ctrl Pts',(15.3722742616431,0.53969261854222,4.31884227776789));
#35459=CARTESIAN_POINT('Ctrl Pts',(15.3881795403307,0.392783856755445,4.48851751501199));
#35460=CARTESIAN_POINT('Ctrl Pts',(15.4040848190183,0.208243281137944,4.55745466359042));
#35461=CARTESIAN_POINT('Ctrl Pts',(15.4097747422597,0.142226097106806,4.58211610408423));
#35462=CARTESIAN_POINT('Ctrl Pts',(15.4154646655011,0.0713929250243718,
4.593885435962));
#35463=CARTESIAN_POINT('Ctrl Pts',(15.4211545887425,0.000414092275955974,
4.59343115273787));
#35464=CARTESIAN_POINT('Origin',(4.,0.,4.));
#35465=CARTESIAN_POINT('',(15.8288454112575,-0.000332254705457391,4.59484959654372));
#35466=CARTESIAN_POINT('',(15.7211545887425,-0.000419917270904514,4.59344262983929));
#35467=CARTESIAN_POINT('',(4.,-7.27562663373442E-17,4.5941));
#35468=CARTESIAN_POINT('Ctrl Pts',(15.8288454112575,-0.000332254705457391,
4.59484959654372));
#35469=CARTESIAN_POINT('Ctrl Pts',(15.814487640426,0.177680873019276,4.5936575613883));
#35470=CARTESIAN_POINT('Ctrl Pts',(15.8001298695944,0.356683508224643,4.50844978272675));
#35471=CARTESIAN_POINT('Ctrl Pts',(15.7857720987628,0.466927807092597,4.36891650689757));
#35472=CARTESIAN_POINT('Ctrl Pts',(15.7698668200752,0.589054446233417,4.21434406913608));
#35473=CARTESIAN_POINT('Ctrl Pts',(15.7539615413876,0.626802179063893,3.99310442736787));
#35474=CARTESIAN_POINT('Ctrl Pts',(15.7380562627,0.562838843643149,3.80678146521555));
#35475=CARTESIAN_POINT('Ctrl Pts',(15.7221509840123,0.498875508222402,3.62045850306322));
#35476=CARTESIAN_POINT('Ctrl Pts',(15.7062457053247,0.333201104550436,3.46905222052678));
#35477=CARTESIAN_POINT('Ctrl Pts',(15.6903404266371,0.141886309687413,3.42208197707538));
#35478=CARTESIAN_POINT('Ctrl Pts',(15.6744351479495,-0.0494284851756215,
3.37511173362399));
#35479=CARTESIAN_POINT('Ctrl Pts',(15.6585298692619,-0.266383671229707,
3.43257752925765));
#35480=CARTESIAN_POINT('Ctrl Pts',(15.6426245905743,-0.409362605655794,
3.5680935017987));
#35481=CARTESIAN_POINT('Ctrl Pts',(15.6267193118867,-0.552341540081869,
3.70360947433975));
#35482=CARTESIAN_POINT('Ctrl Pts',(15.6108140331991,-0.621344222879956,
3.9171756237882));
#35483=CARTESIAN_POINT('Ctrl Pts',(15.5949087545115,-0.584687541371933,
4.11073140955597));
#35484=CARTESIAN_POINT('Ctrl Pts',(15.5790034758238,-0.548030859863907,
4.30428719532377));
#35485=CARTESIAN_POINT('Ctrl Pts',(15.5630981971362,-0.405714814049763,
4.47783261741089));
#35486=CARTESIAN_POINT('Ctrl Pts',(15.5471929184486,-0.223084911271984,
4.55168296009627));
#35487=CARTESIAN_POINT('Ctrl Pts',(15.5410770827183,-0.152860773312716,
4.58007960584922));
#35488=CARTESIAN_POINT('Ctrl Pts',(15.5349612469879,-0.0766761255292402,
4.5937360717991));
#35489=CARTESIAN_POINT('Ctrl Pts',(15.5288454112575,-0.000350670266729247,
4.59332700645389));
#35490=CARTESIAN_POINT('Ctrl Pts',(15.4211545887425,0.000414092275955974,
4.59343115273787));
#35491=CARTESIAN_POINT('Ctrl Pts',(15.4313699441887,-0.12701715326484,4.59261555920332));
#35492=CARTESIAN_POINT('Ctrl Pts',(15.4415852996349,-0.254917899718674,
4.55240018390688));
#35493=CARTESIAN_POINT('Ctrl Pts',(15.4518006550811,-0.356261725310785,
4.47665348962993));
#35494=CARTESIAN_POINT('Ctrl Pts',(15.4677059337687,-0.514053766693778,
4.35871610717824));
#35495=CARTESIAN_POINT('Ctrl Pts',(15.4836112124564,-0.607465460011524,
4.15464228236211));
#35496=CARTESIAN_POINT('Ctrl Pts',(15.499516491144,-0.593606107615349,3.95813408188558));
#35497=CARTESIAN_POINT('Ctrl Pts',(15.5154217698316,-0.579746755219174,
3.76162588140906));
#35498=CARTESIAN_POINT('Ctrl Pts',(15.5313270485192,-0.458616357109098,
3.57268330527213));
#35499=CARTESIAN_POINT('Ctrl Pts',(15.5472323272068,-0.285832867492734,
3.47806079093568));
#35500=CARTESIAN_POINT('Ctrl Pts',(15.5631376058944,-0.113049377876356,
3.38343827659922));
#35501=CARTESIAN_POINT('Ctrl Pts',(15.579042884582,0.111387203246309,3.38313582406324));
#35502=CARTESIAN_POINT('Ctrl Pts',(15.5949481632696,0.284425092952457,3.47729230673655));
#35503=CARTESIAN_POINT('Ctrl Pts',(15.6108534419572,0.457462982658595,3.57144878940986));
#35504=CARTESIAN_POINT('Ctrl Pts',(15.6267587206449,0.579102180948212,3.76006420729246));
#35505=CARTESIAN_POINT('Ctrl Pts',(15.6426639993325,0.593491114096805,3.95653434015292));
#35506=CARTESIAN_POINT('Ctrl Pts',(15.6585692780201,0.607880047245398,4.15300447301339));
#35507=CARTESIAN_POINT('Ctrl Pts',(15.6744745567077,0.515018715252963,4.35732932085173));
#35508=CARTESIAN_POINT('Ctrl Pts',(15.6903798353953,0.357545113131455,4.47569155781202));
#35509=CARTESIAN_POINT('Ctrl Pts',(15.700638086511,0.255981111243369,4.55203033647815));
#35510=CARTESIAN_POINT('Ctrl Pts',(15.7108963376268,0.127540214881222,4.59261107697802));
#35511=CARTESIAN_POINT('Ctrl Pts',(15.7211545887425,-0.000419917270904514,
4.59344262983929));
#35512=CARTESIAN_POINT('Origin',(4.,0.,4.));
#35513=CARTESIAN_POINT('',(16.1288454112575,0.000520203518568921,4.59435747030618));
#35514=CARTESIAN_POINT('',(16.0211545887425,-0.00024144267326323,4.59496181546483));
#35515=CARTESIAN_POINT('',(4.,-7.27562663373442E-17,4.5941));
#35516=CARTESIAN_POINT('Ctrl Pts',(16.1288454112575,0.000520203518568921,
4.59435747030618));
#35517=CARTESIAN_POINT('Ctrl Pts',(16.1258245912393,0.0380542554257849,
4.59470210862833));
#35518=CARTESIAN_POINT('Ctrl Pts',(16.122803771221,0.0755288363057283,4.59145263304759));
#35519=CARTESIAN_POINT('Ctrl Pts',(16.1197829512027,0.112271568866026,4.58439375503351));
#35520=CARTESIAN_POINT('Ctrl Pts',(16.1038776725151,0.305730099191281,4.54722721702202));
#35521=CARTESIAN_POINT('Ctrl Pts',(16.0879723938275,0.478899942385972,4.40445440507416));
#35522=CARTESIAN_POINT('Ctrl Pts',(16.0720671151398,0.55226883266698,4.22163055421683));
#35523=CARTESIAN_POINT('Ctrl Pts',(16.0561618364522,0.625637722947984,4.03880670335952));
#35524=CARTESIAN_POINT('Ctrl Pts',(16.0402565577646,0.599205660315318,3.81593181359275));
#35525=CARTESIAN_POINT('Ctrl Pts',(16.024351279077,0.485109129681553,3.65534060523843));
#35526=CARTESIAN_POINT('Ctrl Pts',(16.0084460003894,0.371012599047788,3.4947493968841));
#35527=CARTESIAN_POINT('Ctrl Pts',(15.9925407217018,0.169251600412921,3.39644186994223));
#35528=CARTESIAN_POINT('Ctrl Pts',(15.9766354430142,-0.0275337514538456,
3.40555668173602));
#35529=CARTESIAN_POINT('Ctrl Pts',(15.9607301643265,-0.224319103320618,
3.41467149352982));
#35530=CARTESIAN_POINT('Ctrl Pts',(15.9448248856389,-0.416128808419276,
3.53120864405929));
#35531=CARTESIAN_POINT('Ctrl Pts',(15.9289196069513,-0.514891964967956,
3.70165920408156));
#35532=CARTESIAN_POINT('Ctrl Pts',(15.9130143282637,-0.613655121516638,
3.87210976410384));
#35533=CARTESIAN_POINT('Ctrl Pts',(15.8971090495761,-0.619371729515322,
4.09647373361892));
#35534=CARTESIAN_POINT('Ctrl Pts',(15.8812037708885,-0.52941696442075,4.27173266988224));
#35535=CARTESIAN_POINT('Ctrl Pts',(15.8652984922009,-0.439462199326184,
4.44699160614554));
#35536=CARTESIAN_POINT('Ctrl Pts',(15.8493932135132,-0.25383606113837,4.57314550915708));
#35537=CARTESIAN_POINT('Ctrl Pts',(15.8334879348256,-0.0577702193188812,
4.59226984378546));
#35538=CARTESIAN_POINT('Ctrl Pts',(15.8319404269696,-0.0386939468137543,
4.59413055045147));
#35539=CARTESIAN_POINT('Ctrl Pts',(15.8303929191136,-0.0195188482833839,
4.59497807636063));
#35540=CARTESIAN_POINT('Ctrl Pts',(15.8288454112575,-0.000332254705457391,
4.59484959654372));
#35541=CARTESIAN_POINT('Ctrl Pts',(15.7211545887425,-0.000419917270904514,
4.59344262983929));
#35542=CARTESIAN_POINT('Ctrl Pts',(15.7268016163144,-0.0708602278282204,
4.59390038836772));
#35543=CARTESIAN_POINT('Ctrl Pts',(15.7324486438863,-0.141154849878182,
4.58231274148771));
#35544=CARTESIAN_POINT('Ctrl Pts',(15.7380956714582,-0.206740066761224,
4.55801389847688));
#35545=CARTESIAN_POINT('Ctrl Pts',(15.7540009501458,-0.391465772281827,
4.48957437609924));
#35546=CARTESIAN_POINT('Ctrl Pts',(15.7699062288334,-0.538831311072463,
4.32029570526172));
#35547=CARTESIAN_POINT('Ctrl Pts',(15.785811507521,-0.58117266224226,4.12790349002296));
#35548=CARTESIAN_POINT('Ctrl Pts',(15.8017167862086,-0.62351401341206,3.93551127478418));
#35549=CARTESIAN_POINT('Ctrl Pts',(15.8176220648962,-0.560831176961022,
3.72000551514415));
#35550=CARTESIAN_POINT('Ctrl Pts',(15.8335273435838,-0.421905459495345,
3.58033733863277));
#35551=CARTESIAN_POINT('Ctrl Pts',(15.8494326222715,-0.282979742029676,
3.44066916212139));
#35552=CARTESIAN_POINT('Ctrl Pts',(15.8653379009591,-0.0678111435493865,
3.37683856873865));
#35553=CARTESIAN_POINT('Ctrl Pts',(15.8812431796467,0.124804018556085,3.41815386651619));
#35554=CARTESIAN_POINT('Ctrl Pts',(15.8971484583343,0.317419180661557,3.45946916429373));
#35555=CARTESIAN_POINT('Ctrl Pts',(15.9130537370219,0.487480906392202,3.60593035323155));
#35556=CARTESIAN_POINT('Ctrl Pts',(15.9289590157095,0.556904046010802,3.79028865163133));
#35557=CARTESIAN_POINT('Ctrl Pts',(15.9448642943971,0.6263271856294,3.9746469500311));
#35558=CARTESIAN_POINT('Ctrl Pts',(15.9607695730847,0.595111739135951,4.19690235789283));
#35559=CARTESIAN_POINT('Ctrl Pts',(15.9766748517723,0.477590518943614,4.35500459477727));
#35560=CARTESIAN_POINT('Ctrl Pts',(15.9915014307624,0.368039615220995,4.50238430120742));
#35561=CARTESIAN_POINT('Ctrl Pts',(16.0063280097524,0.18349252241573,4.59401752470064));
#35562=CARTESIAN_POINT('Ctrl Pts',(16.0211545887425,-0.00024144267326323,
4.59496181546483));
#35563=CARTESIAN_POINT('Origin',(4.,0.,4.));
#35564=CARTESIAN_POINT('',(16.4288454112575,7.48704377684928E-5,4.59312461313858));
#35565=CARTESIAN_POINT('',(16.3211545887425,0.000543344619121817,4.59417988242975));
#35566=CARTESIAN_POINT('',(4.,-7.27562663373442E-17,4.5941));
#35567=CARTESIAN_POINT('Ctrl Pts',(16.4288454112575,7.48704377684928E-5,
4.59312461313858));
#35568=CARTESIAN_POINT('Ctrl Pts',(16.4212562633649,0.0948679978941589,
4.5932308806522));
#35569=CARTESIAN_POINT('Ctrl Pts',(16.4136671154723,0.189615837117123,4.57184094704105));
#35570=CARTESIAN_POINT('Ctrl Pts',(16.4060779675797,0.273126642574496,4.52869916135151));
#35571=CARTESIAN_POINT('Ctrl Pts',(16.3901726888921,0.448147956300534,4.43828293357696));
#35572=CARTESIAN_POINT('Ctrl Pts',(16.3742674102045,0.573812330828296,4.25232504748949));
#35573=CARTESIAN_POINT('Ctrl Pts',(16.3583621315169,0.592420001795879,4.05620949715111));
#35574=CARTESIAN_POINT('Ctrl Pts',(16.3424568528292,0.611027672763462,3.86009394681272));
#35575=CARTESIAN_POINT('Ctrl Pts',(16.3265515741416,0.522578640170867,3.6538207322234));
#35576=CARTESIAN_POINT('Ctrl Pts',(16.310646295454,0.367684957814641,3.53210178682255));
#35577=CARTESIAN_POINT('Ctrl Pts',(16.2947410167664,0.212791275458425,3.4103828414217));
#35578=CARTESIAN_POINT('Ctrl Pts',(16.2788357380788,-0.00854705666138705,
3.3732181652093));
#35579=CARTESIAN_POINT('Ctrl Pts',(16.2629304593912,-0.19470084048803,3.43767220519428));
#35580=CARTESIAN_POINT('Ctrl Pts',(16.2470251807036,-0.380854624314662,
3.50212624517926));
#35581=CARTESIAN_POINT('Ctrl Pts',(16.231119902016,-0.531823859848111,3.66819900136163));
#35582=CARTESIAN_POINT('Ctrl Pts',(16.2152146233283,-0.578289861113055,
3.85963689006134));
#35583=CARTESIAN_POINT('Ctrl Pts',(16.1993093446407,-0.624755862378002,
4.05107477876107));
#35584=CARTESIAN_POINT('Ctrl Pts',(16.1834040659531,-0.566718629374431,
4.26787779997815));
#35585=CARTESIAN_POINT('Ctrl Pts',(16.1674987872655,-0.430826404144746,
4.41049917854914));
#35586=CARTESIAN_POINT('Ctrl Pts',(16.1546143285962,-0.320743594918802,
4.52603310245269));
#35587=CARTESIAN_POINT('Ctrl Pts',(16.1417298699269,-0.159570744489656,
4.592887512417));
#35588=CARTESIAN_POINT('Ctrl Pts',(16.1288454112575,0.000520203518568921,
4.59435747030618));
#35589=CARTESIAN_POINT('Ctrl Pts',(16.0211545887425,-0.00024144267326323,
4.59496181546483));
#35590=CARTESIAN_POINT('Ctrl Pts',(16.0222332884401,-0.0136089074611732,
4.59503051682625));
#35591=CARTESIAN_POINT('Ctrl Pts',(16.0233119881376,-0.0269720681925484,
4.59461918253551));
#35592=CARTESIAN_POINT('Ctrl Pts',(16.0243906878352,-0.0403017303441999,
4.59371435609144));
#35593=CARTESIAN_POINT('Ctrl Pts',(16.0402959665228,-0.236845765548457,
4.58037281461397));
#35594=CARTESIAN_POINT('Ctrl Pts',(16.0562012452104,-0.426106842065734,
4.45974066575184));
#35595=CARTESIAN_POINT('Ctrl Pts',(16.072106523898,-0.521184280535122,4.2872070887372));
#35596=CARTESIAN_POINT('Ctrl Pts',(16.0880118025856,-0.616261719004504,
4.11467351172257));
#35597=CARTESIAN_POINT('Ctrl Pts',(16.1039170812732,-0.61715551942601,3.89023850655542));
#35598=CARTESIAN_POINT('Ctrl Pts',(16.1198223599609,-0.523455286459661,
3.71695313254649));
#35599=CARTESIAN_POINT('Ctrl Pts',(16.1357276386485,-0.429755053493313,
3.54366775853756));
#35600=CARTESIAN_POINT('Ctrl Pts',(16.1516329173361,-0.241460787139106,
3.42153201568684));
#35601=CARTESIAN_POINT('Ctrl Pts',(16.1675381960237,-0.045029248433429,
3.40662546997421));
#35602=CARTESIAN_POINT('Ctrl Pts',(16.1834434747113,0.151402290272254,3.39171892426158));
#35603=CARTESIAN_POINT('Ctrl Pts',(16.1993487533989,0.355971101329402,3.48404157568705));
#35604=CARTESIAN_POINT('Ctrl Pts',(16.2152540320865,0.474747841293266,3.64120276856532));
#35605=CARTESIAN_POINT('Ctrl Pts',(16.2311593107741,0.593524581257127,3.79836396144359));
#35606=CARTESIAN_POINT('Ctrl Pts',(16.2470645894618,0.626509250127697,4.02036369577466));
#35607=CARTESIAN_POINT('Ctrl Pts',(16.2629698681494,0.558556683425868,4.20526908558792));
#35608=CARTESIAN_POINT('Ctrl Pts',(16.278875146837,0.490604116724039,4.39017447540119));
#35609=CARTESIAN_POINT('Ctrl Pts',(16.2947804255246,0.32171431444981,4.53798552069667));
#35610=CARTESIAN_POINT('Ctrl Pts',(16.3106857042122,0.129434328669215,4.58083364284428));
#35611=CARTESIAN_POINT('Ctrl Pts',(16.314175332389,0.0872479785030607,4.5902345478711));
#35612=CARTESIAN_POINT('Ctrl Pts',(16.3176649605657,0.0439357035691123,
4.5945828907904));
#35613=CARTESIAN_POINT('Ctrl Pts',(16.3211545887425,0.000543344619121817,
4.59417988242975));
#35614=CARTESIAN_POINT('Origin',(4.,0.,4.));
#35615=CARTESIAN_POINT('',(16.7288454112575,-0.000548108868865471,4.59408180714414));
#35616=CARTESIAN_POINT('',(16.6211545887425,-2.1752937549985E-5,4.5931168278739));
#35617=CARTESIAN_POINT('',(4.,-7.27562663373442E-17,4.5941));
#35618=CARTESIAN_POINT('Ctrl Pts',(16.7288454112575,-0.000548108868865471,
4.59408180714414));
#35619=CARTESIAN_POINT('Ctrl Pts',(16.7166879354906,0.15068989439403,4.59268722311157));
#35620=CARTESIAN_POINT('Ctrl Pts',(16.7045304597237,0.302891836883802,4.53390177381835));
#35621=CARTESIAN_POINT('Ctrl Pts',(16.6923729839567,0.411632901649024,4.42974331917764));
#35622=CARTESIAN_POINT('Ctrl Pts',(16.6764677052691,0.553895734249677,4.29347578465895));
#35623=CARTESIAN_POINT('Ctrl Pts',(16.6605624265815,0.621772048174623,4.07954898308531));
#35624=CARTESIAN_POINT('Ctrl Pts',(16.6446571478939,0.58409591167956,3.88618905124272));
#35625=CARTESIAN_POINT('Ctrl Pts',(16.6287518692063,0.546419775184499,3.69282911940014));
#35626=CARTESIAN_POINT('Ctrl Pts',(16.6128465905187,0.403191188269443,3.52003605728863));
#35627=CARTESIAN_POINT('Ctrl Pts',(16.596941311831,0.220174658543969,3.44714912875817));
#35628=CARTESIAN_POINT('Ctrl Pts',(16.5810360331434,0.0371581288184754,
3.37426220022769));
#35629=CARTESIAN_POINT('Ctrl Pts',(16.5651307544558,-0.185646343717467,
3.40128140527831));
#35630=CARTESIAN_POINT('Ctrl Pts',(16.5492254757682,-0.34593637135519,3.51580066803907));
#35631=CARTESIAN_POINT('Ctrl Pts',(16.5333201970806,-0.506226398992903,
3.63031993079982));
#35632=CARTESIAN_POINT('Ctrl Pts',(16.517414918393,-0.604001981732426,3.83233925127069));
#35633=CARTESIAN_POINT('Ctrl Pts',(16.5015096397054,-0.594368708523554,
4.02909990422408));
#35634=CARTESIAN_POINT('Ctrl Pts',(16.4856043610178,-0.584735435314682,
4.22586055717748));
#35635=CARTESIAN_POINT('Ctrl Pts',(16.4696990823301,-0.467693306157413,
4.4173625426134));
#35636=CARTESIAN_POINT('Ctrl Pts',(16.4537938036425,-0.296983115116624,
4.51567625060054));
#35637=CARTESIAN_POINT('Ctrl Pts',(16.4454776728475,-0.20772669247752,4.56707991793767));
#35638=CARTESIAN_POINT('Ctrl Pts',(16.4371615420525,-0.103798720846626,
4.59300816600183));
#35639=CARTESIAN_POINT('Ctrl Pts',(16.4288454112575,7.48704377684928E-5,
4.59312461313858));
#35640=CARTESIAN_POINT('Ctrl Pts',(16.3211545887425,0.000543344619121817,
4.59417988242975));
#35641=CARTESIAN_POINT('Ctrl Pts',(16.3335702392533,-0.153841115924154,
4.59274603025257));
#35642=CARTESIAN_POINT('Ctrl Pts',(16.3459858897642,-0.309239316255332,
4.53116741914846));
#35643=CARTESIAN_POINT('Ctrl Pts',(16.3584015402751,-0.418549561707542,
4.42300972860235));
#35644=CARTESIAN_POINT('Ctrl Pts',(16.3743068189627,-0.558583297016706,
4.28445249321304));
#35645=CARTESIAN_POINT('Ctrl Pts',(16.3902120976503,-0.622980598348072,
4.06945282343469));
#35646=CARTESIAN_POINT('Ctrl Pts',(16.4061173763379,-0.582172949355422,
3.87672947174358));
#35647=CARTESIAN_POINT('Ctrl Pts',(16.4220226550255,-0.541365300362771,
3.68400612005246));
#35648=CARTESIAN_POINT('Ctrl Pts',(16.4379279337131,-0.395352701046104,
3.5135590864486));
#35649=CARTESIAN_POINT('Ctrl Pts',(16.4538332124007,-0.211177959727979,
3.44365043774355));
#35650=CARTESIAN_POINT('Ctrl Pts',(16.4697384910883,-0.0270032184098532,
3.37374178903851));
#35651=CARTESIAN_POINT('Ctrl Pts',(16.485643769776,0.195333664909731,3.40437152523229));
#35652=CARTESIAN_POINT('Ctrl Pts',(16.5015490484636,0.353744999708243,3.52147576730199));
#35653=CARTESIAN_POINT('Ctrl Pts',(16.5174543271512,0.512156334506764,3.63858000937169));
#35654=CARTESIAN_POINT('Ctrl Pts',(16.5333596058388,0.606642120784206,3.84215875731731));
#35655=CARTESIAN_POINT('Ctrl Pts',(16.5492648845264,0.59381848284593,4.03873726278877));
#35656=CARTESIAN_POINT('Ctrl Pts',(16.565170163214,0.580994844907655,4.23531576826023));
#35657=CARTESIAN_POINT('Ctrl Pts',(16.5810754419016,0.460861782753675,4.42489403125753));
#35658=CARTESIAN_POINT('Ctrl Pts',(16.5969807205892,0.288579316114369,4.52042573380721));
#35659=CARTESIAN_POINT('Ctrl Pts',(16.6050386766403,0.201297315476928,4.56882414767653));
#35660=CARTESIAN_POINT('Ctrl Pts',(16.6130966326914,0.100630370301649,4.59308406930439));
#35661=CARTESIAN_POINT('Ctrl Pts',(16.6211545887425,-2.1752937549985E-5,
4.5931168278739));
#35662=CARTESIAN_POINT('Origin',(4.,0.,4.));
#35663=CARTESIAN_POINT('',(17.0288454112575,0.000186802344652959,4.59500977980842));
#35664=CARTESIAN_POINT('',(16.9211545887425,-0.000535257393875686,4.59425998651214));
#35665=CARTESIAN_POINT('',(4.,-7.27562663373442E-17,4.5941));
#35666=CARTESIAN_POINT('Ctrl Pts',(17.0288454112575,0.000186802344652959,
4.59500977980842));
#35667=CARTESIAN_POINT('Ctrl Pts',(17.0280248863039,0.0103527338555297,
4.59505157132578));
#35668=CARTESIAN_POINT('Ctrl Pts',(17.0272043613502,0.0205166685362397,
4.5948136789481));
#35669=CARTESIAN_POINT('Ctrl Pts',(17.0263838363966,0.0306658549750798,
4.59428997251885));
#35670=CARTESIAN_POINT('Ctrl Pts',(17.010478557709,0.227400443050786,4.58413830477164));
#35671=CARTESIAN_POINT('Ctrl Pts',(16.9945732790214,0.418593379366704,4.46659200952389));
#35672=CARTESIAN_POINT('Ctrl Pts',(16.9786680003338,0.516456956272638,4.29562337257973));
#35673=CARTESIAN_POINT('Ctrl Pts',(16.9627627216462,0.614320533178566,4.12465473563558));
#35674=CARTESIAN_POINT('Ctrl Pts',(16.9468574429585,0.618854750674521,3.90026375699502));
#35675=CARTESIAN_POINT('Ctrl Pts',(16.9309521642709,0.527977687913284,3.72548128085037));
#35676=CARTESIAN_POINT('Ctrl Pts',(16.9150468855833,0.437100625152047,3.55069880470573));
#35677=CARTESIAN_POINT('Ctrl Pts',(16.8991416068957,0.25081228213362,3.42552483105699));
#35678=CARTESIAN_POINT('Ctrl Pts',(16.8832363282081,0.054648384762208,3.40743395292956));
#35679=CARTESIAN_POINT('Ctrl Pts',(16.8673310495205,-0.141515512609204,
3.38934307480212));
#35680=CARTESIAN_POINT('Ctrl Pts',(16.8514257708328,-0.347554964333599,
3.47833529219599));
#35681=CARTESIAN_POINT('Ctrl Pts',(16.8355204921452,-0.468865370989487,
3.63354914383413));
#35682=CARTESIAN_POINT('Ctrl Pts',(16.8196152134576,-0.590175777645383,
3.78876299547228));
#35683=CARTESIAN_POINT('Ctrl Pts',(16.80370993477,-0.62675713923276,4.01019848135471));
#35684=CARTESIAN_POINT('Ctrl Pts',(16.7878046560824,-0.561812842140477,
4.19618179452704));
#35685=CARTESIAN_POINT('Ctrl Pts',(16.7718993773948,-0.496868545048197,
4.38216510769936));
#35686=CARTESIAN_POINT('Ctrl Pts',(16.7559940987072,-0.330398589276266,
4.53269624816158));
#35687=CARTESIAN_POINT('Ctrl Pts',(16.7400888200196,-0.138838935752124,
4.57865768466082));
#35688=CARTESIAN_POINT('Ctrl Pts',(16.7363410170989,-0.0937012275068688,
4.58948769960953));
#35689=CARTESIAN_POINT('Ctrl Pts',(16.7325932141782,-0.0471704703862807,
4.59451171761327));
#35690=CARTESIAN_POINT('Ctrl Pts',(16.7288454112575,-0.000548108868865471,
4.59408180714414));
#35691=CARTESIAN_POINT('Ctrl Pts',(16.6211545887425,-2.1752937549985E-5,
4.5931168278739));
#35692=CARTESIAN_POINT('Ctrl Pts',(16.629001911379,-0.0980428491191961,
4.59314873014073));
#35693=CARTESIAN_POINT('Ctrl Pts',(16.6368492340155,-0.196049888122182,
4.57020350190738));
#35694=CARTESIAN_POINT('Ctrl Pts',(16.6446965566521,-0.281666676968544,
4.52419924569128));
#35695=CARTESIAN_POINT('Ctrl Pts',(16.6606018353397,-0.455198332287519,
4.43095591292362));
#35696=CARTESIAN_POINT('Ctrl Pts',(16.6765071140273,-0.577829771800838,
4.24298410528626));
#35697=CARTESIAN_POINT('Ctrl Pts',(16.6924123927149,-0.593253826592341,
4.0465925244149));
#35698=CARTESIAN_POINT('Ctrl Pts',(16.7083176714025,-0.608677881383846,
3.85020094354353));
#35699=CARTESIAN_POINT('Ctrl Pts',(16.7242229500901,-0.516894551453523,
3.64538958943816));
#35700=CARTESIAN_POINT('Ctrl Pts',(16.7401282287778,-0.360046858872914,
3.52619917105016));
#35701=CARTESIAN_POINT('Ctrl Pts',(16.7560335074654,-0.203199166292313,
3.40700875266216));
#35702=CARTESIAN_POINT('Ctrl Pts',(16.771938786153,0.0187128889385656,3.37343926999153));
#35703=CARTESIAN_POINT('Ctrl Pts',(16.7878440648406,0.203796679382533,3.44090440927292));
#35704=CARTESIAN_POINT('Ctrl Pts',(16.8037493435282,0.388880469826499,3.50836954855431));
#35705=CARTESIAN_POINT('Ctrl Pts',(16.8196546222158,0.537135995483554,3.67686930978772));
#35706=CARTESIAN_POINT('Ctrl Pts',(16.8355599009034,0.58049059114602,3.86903573125179));
#35707=CARTESIAN_POINT('Ctrl Pts',(16.851465179591,0.623845186808487,4.06120215271587));
#35708=CARTESIAN_POINT('Ctrl Pts',(16.8673704582787,0.562298852476364,4.2770352344106));
#35709=CARTESIAN_POINT('Ctrl Pts',(16.8832757369663,0.424111061064287,4.41743355636644));
#35710=CARTESIAN_POINT('Ctrl Pts',(16.8959020208917,0.314411738992559,4.5288876912157));
#35711=CARTESIAN_POINT('Ctrl Pts',(16.9085283048171,0.156414067554279,4.59280392009262));
#35712=CARTESIAN_POINT('Ctrl Pts',(16.9211545887425,-0.000535257393875686,
4.59425998651214));
#35713=CARTESIAN_POINT('Origin',(4.,0.,4.));
#35714=CARTESIAN_POINT('',(17.3288454112575,0.000452601584348983,4.59351524744837));
#35715=CARTESIAN_POINT('',(17.2211545887425,0.000283723793354941,4.5949151055343));
#35716=CARTESIAN_POINT('',(4.,-7.27562663373442E-17,4.5941));
#35717=CARTESIAN_POINT('Ctrl Pts',(17.3288454112575,0.000452601584348983,
4.59351524744837));
#35718=CARTESIAN_POINT('Ctrl Pts',(17.3234565584296,0.0676518012035294,
4.59398979695312));
#35719=CARTESIAN_POINT('Ctrl Pts',(17.3180677056016,0.134706745978521,4.58346365752876));
#35720=CARTESIAN_POINT('Ctrl Pts',(17.3126788527736,0.197661386620268,4.56129398922237));
#35721=CARTESIAN_POINT('Ctrl Pts',(17.296773574086,0.383472937993069,4.49585988588324));
#35722=CARTESIAN_POINT('Ctrl Pts',(17.2808682953984,0.533564938357213,4.32899388620009));
#35723=CARTESIAN_POINT('Ctrl Pts',(17.2649630167108,0.579021491014364,4.13731379770915));
#35724=CARTESIAN_POINT('Ctrl Pts',(17.2490577380232,0.624478043671518,3.94563370921821));
#35725=CARTESIAN_POINT('Ctrl Pts',(17.2331524593355,0.565299148621668,3.72913953191949));
#35726=CARTESIAN_POINT('Ctrl Pts',(17.2172471806479,0.428657250819126,3.58723623291525));
#35727=CARTESIAN_POINT('Ctrl Pts',(17.2013419019603,0.292015353016592,3.44533293391101));
#35728=CARTESIAN_POINT('Ctrl Pts',(17.1854366232727,0.0779104524613767,
3.37802051320125));
#35729=CARTESIAN_POINT('Ctrl Pts',(17.1695313445851,-0.115349538542919,
3.41620598662221));
#35730=CARTESIAN_POINT('Ctrl Pts',(17.1536260658975,-0.308609529547215,
3.45439146004317));
#35731=CARTESIAN_POINT('Ctrl Pts',(17.1377207872099,-0.48102461100059,3.59807482759486));
#35732=CARTESIAN_POINT('Ctrl Pts',(17.1218155085223,-0.553429071780215,
3.78128276563952));
#35733=CARTESIAN_POINT('Ctrl Pts',(17.1059102298347,-0.625833532559839,
3.96449070368418));
#35734=CARTESIAN_POINT('Ctrl Pts',(17.090004951147,-0.598227372665711,4.18722321222181));
#35735=CARTESIAN_POINT('Ctrl Pts',(17.0740996724594,-0.483286172800906,
4.34721094636728));
#35736=CARTESIAN_POINT('Ctrl Pts',(17.0590149187255,-0.374274584390508,
4.4989451987145));
#35737=CARTESIAN_POINT('Ctrl Pts',(17.0439301649915,-0.186706445247169,
4.59424147319602));
#35738=CARTESIAN_POINT('Ctrl Pts',(17.0288454112575,0.000186802344652959,
4.59500977980842));
#35739=CARTESIAN_POINT('Ctrl Pts',(16.9211545887425,-0.000535257393875686,
4.59425998651214));
#35740=CARTESIAN_POINT('Ctrl Pts',(16.9244335835047,-0.0412943609811605,
4.59463812105998));
#35741=CARTESIAN_POINT('Ctrl Pts',(16.9277125782669,-0.0819827620002526,
4.59080381827239));
#35742=CARTESIAN_POINT('Ctrl Pts',(16.9309915730291,-0.121736182180322,
4.58249572362891));
#35743=CARTESIAN_POINT('Ctrl Pts',(16.9468968517167,-0.31456638552074,4.54219600671859));
#35744=CARTESIAN_POINT('Ctrl Pts',(16.9628021304043,-0.485397543709551,
4.39663301068103));
#35745=CARTESIAN_POINT('Ctrl Pts',(16.978707409092,-0.555791216176751,4.21264310503418));
#35746=CARTESIAN_POINT('Ctrl Pts',(16.9946126877796,-0.626184888643955,
4.02865319938731));
#35747=CARTESIAN_POINT('Ctrl Pts',(17.0105179664672,-0.596141075389537,
3.80623638413113));
#35748=CARTESIAN_POINT('Ctrl Pts',(17.0264232451548,-0.479454624411006,
3.64751705115182));
#35749=CARTESIAN_POINT('Ctrl Pts',(17.0423285238424,-0.362768173432475,
3.48879771817251));
#35750=CARTESIAN_POINT('Ctrl Pts',(17.05823380253,-0.159439084729831,3.39377586747005));
#35751=CARTESIAN_POINT('Ctrl Pts',(17.0741390812176,0.0371725263090214,
3.40608151284405));
#35752=CARTESIAN_POINT('Ctrl Pts',(17.0900443599052,0.233784137347885,3.41838715821804));
#35753=CARTESIAN_POINT('Ctrl Pts',(17.1059496385929,0.423678270722955,3.5380202996685));
#35754=CARTESIAN_POINT('Ctrl Pts',(17.1218549172805,0.519663574146654,3.71005045990219));
#35755=CARTESIAN_POINT('Ctrl Pts',(17.1377601959681,0.615648877570348,3.88208062013586));
#35756=CARTESIAN_POINT('Ctrl Pts',(17.1536654746557,0.617725351042682,4.10650779915277));
#35757=CARTESIAN_POINT('Ctrl Pts',(17.1695707533433,0.524939565793509,4.28028453107927));
#35758=CARTESIAN_POINT('Ctrl Pts',(17.1854760320309,0.432153780544336,4.45406126300578));
#35759=CARTESIAN_POINT('Ctrl Pts',(17.2013813107185,0.244505736573655,4.5771875478419));
#35760=CARTESIAN_POINT('Ctrl Pts',(17.2172865894061,0.0481554769387473,
4.59312900463441));
#35761=CARTESIAN_POINT('Ctrl Pts',(17.2185759225182,0.0322386925622284,
4.59442127046022));
#35762=CARTESIAN_POINT('Ctrl Pts',(17.2198652556304,0.0162647237884017,
4.5950091984451));
#35763=CARTESIAN_POINT('Ctrl Pts',(17.2211545887425,0.000283723793354941,
4.5949151055343));
#35764=CARTESIAN_POINT('Origin',(4.,0.,4.));
#35765=CARTESIAN_POINT('',(17.6288454112575,-0.000376811216598938,4.5933658344624));
#35766=CARTESIAN_POINT('',(17.5211545887425,0.000390292690419375,4.59338796628294));
#35767=CARTESIAN_POINT('',(4.,-7.27562663373442E-17,4.5941));
#35768=CARTESIAN_POINT('Ctrl Pts',(17.6288454112575,-0.000376811216598938,
4.5933658344624));
#35769=CARTESIAN_POINT('Ctrl Pts',(17.6188882305552,0.123868145157646,4.5926473455414));
#35770=CARTESIAN_POINT('Ctrl Pts',(17.608931049853,0.248515939035854,4.55458993700248));
#35771=CARTESIAN_POINT('Ctrl Pts',(17.5989738691507,0.348483110949462,4.48236965854082));
#35772=CARTESIAN_POINT('Ctrl Pts',(17.5830685904631,0.508167440925656,4.36700731952407));
#35773=CARTESIAN_POINT('Ctrl Pts',(17.5671633117754,0.604877102606476,4.16447556457896));
#35774=CARTESIAN_POINT('Ctrl Pts',(17.5512580330878,0.594207110796467,3.96776840716434));
#35775=CARTESIAN_POINT('Ctrl Pts',(17.5353527544002,0.583537118986457,3.77106124974973));
#35776=CARTESIAN_POINT('Ctrl Pts',(17.5194474757126,0.465487473685617,3.58017868986561));
#35777=CARTESIAN_POINT('Ctrl Pts',(17.503542197025,0.294261577747463,3.48276592343564));
#35778=CARTESIAN_POINT('Ctrl Pts',(17.4876369183374,0.123035681809298,3.38535315700567));
#35779=CARTESIAN_POINT('Ctrl Pts',(17.4717316396498,-0.101366464766187,
3.38141018402985));
#35780=CARTESIAN_POINT('Ctrl Pts',(17.4558263609621,-0.275908889943427,
3.47274745088526));
#35781=CARTESIAN_POINT('Ctrl Pts',(17.4399210822745,-0.450451315120656,
3.56408471774066));
#35782=CARTESIAN_POINT('Ctrl Pts',(17.4240158035869,-0.575134018899647,
3.75070222442727));
#35783=CARTESIAN_POINT('Ctrl Pts',(17.4081105248993,-0.592707978595278,
3.94691310701022));
#35784=CARTESIAN_POINT('Ctrl Pts',(17.3922052462117,-0.610281938290908,
4.14312398959316));
#35785=CARTESIAN_POINT('Ctrl Pts',(17.3762999675241,-0.520747153903178,
4.34892824807245));
#35786=CARTESIAN_POINT('Ctrl Pts',(17.3603946888365,-0.365214210518585,
4.46982927381454));
#35787=CARTESIAN_POINT('Ctrl Pts',(17.3498782629768,-0.262377240481122,
4.54976793433994));
#35788=CARTESIAN_POINT('Ctrl Pts',(17.3393618371172,-0.130687628661636,
4.59258915708319));
#35789=CARTESIAN_POINT('Ctrl Pts',(17.3288454112575,0.000452601584348983,
4.59351524744837));
#35790=CARTESIAN_POINT('Ctrl Pts',(17.2211545887425,0.000283723793354941,
4.5949151055343));
#35791=CARTESIAN_POINT('Ctrl Pts',(17.235770534318,-0.18087770297476,4.59384846352355));
#35792=CARTESIAN_POINT('Ctrl Pts',(17.2503864798935,-0.362942684182573,
4.50513801271133));
#35793=CARTESIAN_POINT('Ctrl Pts',(17.265002425469,-0.47285052735612,4.36129398677095));
#35794=CARTESIAN_POINT('Ctrl Pts',(17.2809077041566,-0.592453796716944,
4.20476088336606));
#35795=CARTESIAN_POINT('Ctrl Pts',(17.2968129828442,-0.626607860139456,
3.98293804780737));
#35796=CARTESIAN_POINT('Ctrl Pts',(17.3127182615318,-0.559630616639302,
3.79767714163318));
#35797=CARTESIAN_POINT('Ctrl Pts',(17.3286235402194,-0.492653373139145,
3.61241623545897));
#35798=CARTESIAN_POINT('Ctrl Pts',(17.3445288189071,-0.324544822716309,
3.46371725866926));
#35799=CARTESIAN_POINT('Ctrl Pts',(17.3604340975947,-0.132493299638714,
3.41985649047097));
#35800=CARTESIAN_POINT('Ctrl Pts',(17.3763393762823,0.0595582234388708,
3.37599572227269));
#35801=CARTESIAN_POINT('Ctrl Pts',(17.3922446549699,0.275552719171213,3.43697316266583));
#35802=CARTESIAN_POINT('Ctrl Pts',(17.4081499336575,0.416314653091553,3.5747905507646));
#35803=CARTESIAN_POINT('Ctrl Pts',(17.4240552123451,0.557076587011893,3.71260793886338));
#35804=CARTESIAN_POINT('Ctrl Pts',(17.4399604910327,0.622605959120231,3.92726527466781));
#35805=CARTESIAN_POINT('Ctrl Pts',(17.4558657697203,0.582814454063527,4.12020099097945));
#35806=CARTESIAN_POINT('Ctrl Pts',(17.4717710484079,0.543022949006823,4.31313670729109));
#35807=CARTESIAN_POINT('Ctrl Pts',(17.4876763270955,0.397910566785078,4.48435080410994));
#35808=CARTESIAN_POINT('Ctrl Pts',(17.5035816057832,0.214106774115907,4.55522901164789));
#35809=CARTESIAN_POINT('Ctrl Pts',(17.5094392667696,0.146414762764002,4.58133232736073));
#35810=CARTESIAN_POINT('Ctrl Pts',(17.515296927756,0.073474912906076,4.59382676872096));
#35811=CARTESIAN_POINT('Ctrl Pts',(17.5211545887425,0.000390292690419375,
4.59338796628294));
#35812=CARTESIAN_POINT('Origin',(4.,0.,4.));
#35813=CARTESIAN_POINT('',(17.9288454112575,-0.000301159635511528,4.59489313984584));
#35814=CARTESIAN_POINT('',(17.8211545887425,-0.000441626631060947,4.59348913571676));
#35815=CARTESIAN_POINT('',(4.,-7.27562663373442E-17,4.5941));
#35816=CARTESIAN_POINT('Ctrl Pts',(17.9288454112575,-0.000301159635511528,
4.59489313984584));
#35817=CARTESIAN_POINT('Ctrl Pts',(17.9143199026809,0.179756887528332,4.59377956832623));
#35818=CARTESIAN_POINT('Ctrl Pts',(17.8997943941043,0.360751589755073,4.50630604003092));
#35819=CARTESIAN_POINT('Ctrl Pts',(17.8852688855277,0.470789914960854,4.36397502945801));
#35820=CARTESIAN_POINT('Ctrl Pts',(17.8693636068401,0.591280720462369,4.20812407407766));
#35821=CARTESIAN_POINT('Ctrl Pts',(17.8534583281524,0.626694694978596,3.98649889312445));
#35822=CARTESIAN_POINT('Ctrl Pts',(17.8375530494648,0.560771239653389,3.80086039350393));
#35823=CARTESIAN_POINT('Ctrl Pts',(17.8216477707772,0.494847784328189,3.61522189388343));
#35824=CARTESIAN_POINT('Ctrl Pts',(17.8057424920896,0.327586899161578,3.46557007559562));
#35825=CARTESIAN_POINT('Ctrl Pts',(17.789837213402,0.135787706397568,3.42061872235194));
#35826=CARTESIAN_POINT('Ctrl Pts',(17.7739319347144,-0.0560114863664412,
3.37566736910827));
#35827=CARTESIAN_POINT('Ctrl Pts',(17.7580266560268,-0.272348986727849,
3.43541648090873));
#35828=CARTESIAN_POINT('Ctrl Pts',(17.7421213773392,-0.41389176700556,3.57243179339102));
#35829=CARTESIAN_POINT('Ctrl Pts',(17.7262160986515,-0.555434547283271,
3.7094471058733));
#35830=CARTESIAN_POINT('Ctrl Pts',(17.710310819964,-0.622182607477285,3.92372861903742));
#35831=CARTESIAN_POINT('Ctrl Pts',(17.6944055412763,-0.583488062224059,
4.11688732754162));
#35832=CARTESIAN_POINT('Ctrl Pts',(17.6785002625887,-0.544793516970831,
4.31004603604583));
#35833=CARTESIAN_POINT('Ctrl Pts',(17.6625949839011,-0.400656366270352,
4.48208193989012));
#35834=CARTESIAN_POINT('Ctrl Pts',(17.6466897052135,-0.217258291784321,
4.55400343026805));
#35835=CARTESIAN_POINT('Ctrl Pts',(17.6407416072282,-0.148672903323923,
4.58089991415997));
#35836=CARTESIAN_POINT('Ctrl Pts',(17.6347935092429,-0.0745967331795002,
4.59379503652584));
#35837=CARTESIAN_POINT('Ctrl Pts',(17.6288454112575,-0.000376811216598938,
4.5933658344624));
#35838=CARTESIAN_POINT('Ctrl Pts',(17.5211545887425,0.000390292690419375,
4.59338796628294));
#35839=CARTESIAN_POINT('Ctrl Pts',(17.5312022064437,-0.12497140465997,4.59263529057266));
#35840=CARTESIAN_POINT('Ctrl Pts',(17.5412498241448,-0.250759050797478,
4.55382993891589));
#35841=CARTESIAN_POINT('Ctrl Pts',(17.551297441846,-0.351218450958555,4.48038168762358));
#35842=CARTESIAN_POINT('Ctrl Pts',(17.5672027205336,-0.510244680247213,
4.36411383780432));
#35843=CARTESIAN_POINT('Ctrl Pts',(17.5831079992212,-0.605801935707933,
4.16103581990878));
#35844=CARTESIAN_POINT('Ctrl Pts',(17.5990132779088,-0.594014368327242,
3.96439246823218));
#35845=CARTESIAN_POINT('Ctrl Pts',(17.6149185565964,-0.58222680094655,3.76774911655557));
#35846=CARTESIAN_POINT('Ctrl Pts',(17.6308238352841,-0.463094410724447,
3.5775404310979));
#35847=CARTESIAN_POINT('Ctrl Pts',(17.6467291139717,-0.291317751175132,
3.48110219315546));
#35848=CARTESIAN_POINT('Ctrl Pts',(17.6626343926593,-0.119541091625818,
3.38466395521302));
#35849=CARTESIAN_POINT('Ctrl Pts',(17.6785396713469,0.104879837250709,3.38199616478582));
#35850=CARTESIAN_POINT('Ctrl Pts',(17.6944449500345,0.278900439380867,3.47432375837312));
#35851=CARTESIAN_POINT('Ctrl Pts',(17.7103502287221,0.452921041511034,3.56665135196042));
#35852=CARTESIAN_POINT('Ctrl Pts',(17.7262555074097,0.576541316894826,3.75397432956222));
#35853=CARTESIAN_POINT('Ctrl Pts',(17.7421607860974,0.593000065018554,3.95028190484542));
#35854=CARTESIAN_POINT('Ctrl Pts',(17.758066064785,0.60945881314228,4.1465894801286));
#35855=CARTESIAN_POINT('Ctrl Pts',(17.7739713434726,0.518756034005955,4.35188165309317));
#35856=CARTESIAN_POINT('Ctrl Pts',(17.7898766221602,0.362538606470845,4.47189694310939));
#35857=CARTESIAN_POINT('Ctrl Pts',(17.8003026110209,0.260137309937395,4.55056755941266));
#35858=CARTESIAN_POINT('Ctrl Pts',(17.8107285998817,0.129585238016204,4.59259583028147));
#35859=CARTESIAN_POINT('Ctrl Pts',(17.8211545887425,-0.000441626631060947,
4.59348913571676));
#35860=CARTESIAN_POINT('Origin',(4.,0.,4.));
#35861=CARTESIAN_POINT('',(18.2288454112575,0.000530626821107938,4.59429426521737));
#35862=CARTESIAN_POINT('',(18.1211545887425,-0.000206261771334874,4.59499421029555));
#35863=CARTESIAN_POINT('',(4.,-7.27562663373442E-17,4.5941));
#35864=CARTESIAN_POINT('Ctrl Pts',(18.2288454112575,0.000530626821107938,
4.59429426521737));
#35865=CARTESIAN_POINT('Ctrl Pts',(18.2256568534942,0.0401596894680921,
4.59466101186164));
#35866=CARTESIAN_POINT('Ctrl Pts',(18.2224682957309,0.0797220295111884,
4.5910372210354));
#35867=CARTESIAN_POINT('Ctrl Pts',(18.2192797379675,0.118424305077702,4.58317806034235));
#35868=CARTESIAN_POINT('Ctrl Pts',(18.2033744592799,0.311480390123117,4.54397471188459));
#35869=CARTESIAN_POINT('Ctrl Pts',(18.1874691805923,0.483135922039688,4.39938477867344));
#35870=CARTESIAN_POINT('Ctrl Pts',(18.1715639019047,0.554573942717995,4.21579784094385));
#35871=CARTESIAN_POINT('Ctrl Pts',(18.1556586232171,0.626011963396302,4.03221090321426));
#35872=CARTESIAN_POINT('Ctrl Pts',(18.1397533445295,0.597232472836345,3.80962696096622));
#35873=CARTESIAN_POINT('Ctrl Pts',(18.1238480658419,0.481449795543417,3.65024714373002));
#35874=CARTESIAN_POINT('Ctrl Pts',(18.1079427871543,0.365667118250483,3.49086732649381));
#35875=CARTESIAN_POINT('Ctrl Pts',(18.0920375084667,0.16288125422457,3.39469163426944));
#35876=CARTESIAN_POINT('Ctrl Pts',(18.076132229779,-0.0337971069360236,
3.40587987606835));
#35877=CARTESIAN_POINT('Ctrl Pts',(18.0602269510914,-0.230475468096606,
3.41706811786726));
#35878=CARTESIAN_POINT('Ctrl Pts',(18.0443216724038,-0.421046326391869,
3.53562029368944));
#35879=CARTESIAN_POINT('Ctrl Pts',(18.0284163937162,-0.518007606080761,
3.70710225992629));
#35880=CARTESIAN_POINT('Ctrl Pts',(18.0125111150286,-0.614968885769652,
3.87858422616314));
#35881=CARTESIAN_POINT('Ctrl Pts',(17.996605836341,-0.618320586852172,4.10299598281466));
#35882=CARTESIAN_POINT('Ctrl Pts',(17.9807005576534,-0.526523749990007,
4.27729714530494));
#35883=CARTESIAN_POINT('Ctrl Pts',(17.9647952789658,-0.434726913127837,
4.45159830779523));
#35884=CARTESIAN_POINT('Ctrl Pts',(17.9488900002781,-0.247781538320971,
4.57578887612429));
#35885=CARTESIAN_POINT('Ctrl Pts',(17.9329847215905,-0.0515250326741526,
4.59284579538505));
#35886=CARTESIAN_POINT('Ctrl Pts',(17.9316049514795,-0.0344999389365885,
4.59432546938787));
#35887=CARTESIAN_POINT('Ctrl Pts',(17.9302251813685,-0.0174047750035579,
4.59499891739512));
#35888=CARTESIAN_POINT('Ctrl Pts',(17.9288454112575,-0.000301159635511528,
4.59489313984584));
#35889=CARTESIAN_POINT('Ctrl Pts',(17.8211545887425,-0.000441626631060947,
4.59348913571676));
#35890=CARTESIAN_POINT('Ctrl Pts',(17.8266338785693,-0.0687761401428734,
4.59395860479535));
#35891=CARTESIAN_POINT('Ctrl Pts',(17.8321131683962,-0.136965594625977,
4.58306684864343));
#35892=CARTESIAN_POINT('Ctrl Pts',(17.837592458223,-0.200847632772524,4.56016175744822));
#35893=CARTESIAN_POINT('Ctrl Pts',(17.8534977369106,-0.386284368546891,
4.49367287470298));
#35894=CARTESIAN_POINT('Ctrl Pts',(17.8694030155983,-0.535425764161732,
4.32595670214462));
#35895=CARTESIAN_POINT('Ctrl Pts',(17.8853082942859,-0.579792400402821,
4.13402141072584));
#35896=CARTESIAN_POINT('Ctrl Pts',(17.9012135729735,-0.624159036643913,
3.94208611930704));
#35897=CARTESIAN_POINT('Ctrl Pts',(17.9171188516611,-0.563750913511241,
3.72593170902781));
#35898=CARTESIAN_POINT('Ctrl Pts',(17.9330241303487,-0.426304885490399,
3.58480714034942));
#35899=CARTESIAN_POINT('Ctrl Pts',(17.9489294090363,-0.288858857469565,
3.44368257167104));
#35900=CARTESIAN_POINT('Ctrl Pts',(17.9648346877239,-0.0743749245605683,
3.37758784459349));
#35901=CARTESIAN_POINT('Ctrl Pts',(17.9807399664116,0.118664965311668,3.41687086155347));
#35902=CARTESIAN_POINT('Ctrl Pts',(17.9966452450992,0.311704855183904,3.45615387851346));
#35903=CARTESIAN_POINT('Ctrl Pts',(18.0125505237868,0.483300702019379,3.60081463951098));
#35904=CARTESIAN_POINT('Ctrl Pts',(18.0284558024744,0.554662952572844,3.78443104318807));
#35905=CARTESIAN_POINT('Ctrl Pts',(18.044361081162,0.62602520312631,3.96804744686516));
#35906=CARTESIAN_POINT('Ctrl Pts',(18.0602663598496,0.597153857397765,4.19061949322182));
#35907=CARTESIAN_POINT('Ctrl Pts',(18.0761716385372,0.481305415899848,4.34995151481781));
#35908=CARTESIAN_POINT('Ctrl Pts',(18.0911659552723,0.372092100044007,4.50015792394613));
#35909=CARTESIAN_POINT('Ctrl Pts',(18.1061602720074,0.185579460002099,4.59416090236354));
#35910=CARTESIAN_POINT('Ctrl Pts',(18.1211545887425,-0.000206261771334874,
4.59499421029555));
#35911=CARTESIAN_POINT('Origin',(4.,0.,4.));
#35912=CARTESIAN_POINT('',(18.5288454112575,4.04073003155148E-5,4.59311858068669));
#35913=CARTESIAN_POINT('',(18.4211545887425,0.000547083855738422,4.59411609730493));
#35914=CARTESIAN_POINT('',(4.,-7.27562663373442E-17,4.5941));
#35915=CARTESIAN_POINT('Ctrl Pts',(18.5288454112575,4.04073003155148E-5,
4.59311858068669));
#35916=CARTESIAN_POINT('Ctrl Pts',(18.5210885256199,0.0969311390001333,
4.59317716754242));
#35917=CARTESIAN_POINT('Ctrl Pts',(18.5133316399822,0.193796352446061,4.57078374547556));
#35918=CARTESIAN_POINT('Ctrl Pts',(18.5055747543446,0.27868347559656,4.52579129559858));
#35919=CARTESIAN_POINT('Ctrl Pts',(18.489669475657,0.452742165355285,4.43353552600749));
#35920=CARTESIAN_POINT('Ctrl Pts',(18.4737641969693,0.576439736070726,4.24626358090446));
#35921=CARTESIAN_POINT('Ctrl Pts',(18.4578589182817,0.592979496483005,4.04996281465819));
#35922=CARTESIAN_POINT('Ctrl Pts',(18.4419536395941,0.609519256895283,3.85366204841193));
#35923=CARTESIAN_POINT('Ctrl Pts',(18.4260483609065,0.518901207004412,3.64833246102244));
#35924=CARTESIAN_POINT('Ctrl Pts',(18.4101430822189,0.362733321586741,3.52825271224048));
#35925=CARTESIAN_POINT('Ctrl Pts',(18.3942378035313,0.206565436169079,3.40817296345854));
#35926=CARTESIAN_POINT('Ctrl Pts',(18.3783325248437,-0.015152284775374,
3.37334305328413));
#35927=CARTESIAN_POINT('Ctrl Pts',(18.3624272461561,-0.200616443892158,
3.43975540293737));
#35928=CARTESIAN_POINT('Ctrl Pts',(18.3465219674685,-0.386080603008964,
3.50616775259061));
#35929=CARTESIAN_POINT('Ctrl Pts',(18.3306166887808,-0.535291200298091,
3.67382236207151));
#35930=CARTESIAN_POINT('Ctrl Pts',(18.3147114100932,-0.579737042064157,
3.86573932758804));
#35931=CARTESIAN_POINT('Ctrl Pts',(18.2988061314056,-0.624182883830224,
4.05765629310458));
#35932=CARTESIAN_POINT('Ctrl Pts',(18.282900852718,-0.563863970073232,4.27383561465674));
#35933=CARTESIAN_POINT('Ctrl Pts',(18.2669955740304,-0.426476194107598,
4.41501689358062));
#35934=CARTESIAN_POINT('Ctrl Pts',(18.2542788531061,-0.316630774880643,
4.52789532589669));
#35935=CARTESIAN_POINT('Ctrl Pts',(18.2415621321818,-0.157519428275204,
4.5928315930404));
#35936=CARTESIAN_POINT('Ctrl Pts',(18.2288454112575,0.000530626821107938,
4.59429426521737));
#35937=CARTESIAN_POINT('Ctrl Pts',(18.1211545887425,-0.000206261771334874,
4.59499421029555));
#35938=CARTESIAN_POINT('Ctrl Pts',(18.122065550695,-0.0114934532352288,
4.59504483693191));
#35939=CARTESIAN_POINT('Ctrl Pts',(18.1229765126475,-0.0227779616248223,
4.59475157188293));
#35940=CARTESIAN_POINT('Ctrl Pts',(18.1238874746001,-0.0340422900297544,
4.59410612569417));
#35941=CARTESIAN_POINT('Ctrl Pts',(18.1397927532877,-0.230716017194119,
4.58283671813918));
#35942=CARTESIAN_POINT('Ctrl Pts',(18.1556980319753,-0.421237934255556,
4.46420590619388));
#35943=CARTESIAN_POINT('Ctrl Pts',(18.1716033106629,-0.518128437217054,
4.29268393984778));
#35944=CARTESIAN_POINT('Ctrl Pts',(18.1875085893505,-0.615018940178556,
4.12116197350168));
#35945=CARTESIAN_POINT('Ctrl Pts',(18.2034138680381,-0.618278029040109,
3.89674885275477));
#35946=CARTESIAN_POINT('Ctrl Pts',(18.2193191467258,-0.526409268077163,
3.72248558851787));
#35947=CARTESIAN_POINT('Ctrl Pts',(18.2352244254134,-0.434540507114227,
3.54822232428098));
#35948=CARTESIAN_POINT('Ctrl Pts',(18.251129704101,-0.24754389632682,3.42410891655409));
#35949=CARTESIAN_POINT('Ctrl Pts',(18.2670349827886,-0.0512803682143169,
3.40713299136011));
#35950=CARTESIAN_POINT('Ctrl Pts',(18.2829402614762,0.144983159898198,3.39015706616613));
#35951=CARTESIAN_POINT('Ctrl Pts',(18.2988455401638,0.35051360533581,3.48031862350507));
#35952=CARTESIAN_POINT('Ctrl Pts',(18.3147508188514,0.470940082829639,3.63621929066782));
#35953=CARTESIAN_POINT('Ctrl Pts',(18.330656097539,0.591366560323475,3.79211995783059));
#35954=CARTESIAN_POINT('Ctrl Pts',(18.3465613762266,0.62668906987352,4.01375973481717));
#35955=CARTESIAN_POINT('Ctrl Pts',(18.3624666549143,0.560689009466533,4.199371012841));
#35956=CARTESIAN_POINT('Ctrl Pts',(18.3783719336019,0.49468894905955,4.38498229086483));
#35957=CARTESIAN_POINT('Ctrl Pts',(18.3942772122895,0.327366318695548,4.53456506992591));
#35958=CARTESIAN_POINT('Ctrl Pts',(18.4101824909771,0.135548591400956,4.57943726620491));
#35959=CARTESIAN_POINT('Ctrl Pts',(18.4138398568989,0.0914407431336166,
4.58975547846199));
#35960=CARTESIAN_POINT('Ctrl Pts',(18.4174972228207,0.0460377050408626,
4.59453706917327));
#35961=CARTESIAN_POINT('Ctrl Pts',(18.4211545887425,0.000547083855738422,
4.59411609730493));
#35962=CARTESIAN_POINT('Origin',(4.,0.,4.));
#35963=CARTESIAN_POINT('',(18.8288454112575,-0.000545657836941327,4.59414547262434));
#35964=CARTESIAN_POINT('',(18.7211545887425,-5.63168744233308E-5,4.59312091231189));
#35965=CARTESIAN_POINT('',(4.,-7.27562663373442E-17,4.5941));
#35966=CARTESIAN_POINT('Ctrl Pts',(18.8288454112575,-0.000545657836941327,
4.59414547262434));
#35967=CARTESIAN_POINT('Ctrl Pts',(18.8165201977456,0.15273698101805,4.59272393327212));
#35968=CARTESIAN_POINT('Ctrl Pts',(18.8041949842336,0.307016766534516,4.53213273669464));
#35969=CARTESIAN_POINT('Ctrl Pts',(18.7918697707216,0.416139138999065,4.42538122089617));
#35970=CARTESIAN_POINT('Ctrl Pts',(18.775964492034,0.556957936451544,4.28762193522949));
#35971=CARTESIAN_POINT('Ctrl Pts',(18.7600592133464,0.622575889387102,4.0729916608594));
#35972=CARTESIAN_POINT('Ctrl Pts',(18.7441539346588,0.582864009884755,3.88003953951897));
#35973=CARTESIAN_POINT('Ctrl Pts',(18.7282486559712,0.543152130382401,3.6870874181785));
#35974=CARTESIAN_POINT('Ctrl Pts',(18.7123433772835,0.3981104184421,3.51581344986768));
#35975=CARTESIAN_POINT('Ctrl Pts',(18.6964380985959,0.214335891977863,3.44485939483061));
#35976=CARTESIAN_POINT('Ctrl Pts',(18.6805328199083,0.0305613655136472,
3.37390533979354));
#35977=CARTESIAN_POINT('Ctrl Pts',(18.6646275412207,-0.191945975474496,
3.40327119803019));
#35978=CARTESIAN_POINT('Ctrl Pts',(18.6487222625331,-0.351020173514001,
3.51947340980541));
#35979=CARTESIAN_POINT('Ctrl Pts',(18.6328169838455,-0.510094371553506,
3.63567562158063));
#35980=CARTESIAN_POINT('Ctrl Pts',(18.6169117051579,-0.605735426644373,
3.83871418689441));
#35981=CARTESIAN_POINT('Ctrl Pts',(18.6010064264702,-0.594029012528289,
4.03536238640794));
#35982=CARTESIAN_POINT('Ctrl Pts',(18.5851011477826,-0.582322598412206,
4.23201058592146));
#35983=CARTESIAN_POINT('Ctrl Pts',(18.569195869095,-0.463268715089173,4.42226841963472));
#35984=CARTESIAN_POINT('Ctrl Pts',(18.5532905904074,-0.29153186902666,4.51877753945177));
#35985=CARTESIAN_POINT('Ctrl Pts',(18.5451421973574,-0.203549800283198,
4.56821988225003));
#35986=CARTESIAN_POINT('Ctrl Pts',(18.5369938043075,-0.101740616897797,
4.59305703682098));
#35987=CARTESIAN_POINT('Ctrl Pts',(18.5288454112575,4.04073003155148E-5,
4.59311858068669));
#35988=CARTESIAN_POINT('Ctrl Pts',(18.4211545887425,0.000547083855738422,
4.59411609730493));
#35989=CARTESIAN_POINT('Ctrl Pts',(18.4334025015083,-0.151793472668411,
4.59270633223614));
#35990=CARTESIAN_POINT('Ctrl Pts',(18.4456504142741,-0.305116246576315,
4.53295143150856));
#35991=CARTESIAN_POINT('Ctrl Pts',(18.4578983270399,-0.414068183831284,
4.42739736222451));
#35992=CARTESIAN_POINT('Ctrl Pts',(18.4738036057275,-0.555554407543751,
4.29032364846819));
#35993=CARTESIAN_POINT('Ctrl Pts',(18.4897088844152,-0.622214030743504,
4.07601460745865));
#35994=CARTESIAN_POINT('Ctrl Pts',(18.5056141631028,-0.583439774593308,
3.88287188415962));
#35995=CARTESIAN_POINT('Ctrl Pts',(18.5215194417904,-0.54466551844311,3.68972916086059));
#35996=CARTESIAN_POINT('Ctrl Pts',(18.537424720478,-0.400457382942952,3.51775275527208));
#35997=CARTESIAN_POINT('Ctrl Pts',(18.5533299991656,-0.217029642971419,
3.44590695711865));
#35998=CARTESIAN_POINT('Ctrl Pts',(18.5692352778532,-0.0336019029998957,
3.37406115896522));
#35999=CARTESIAN_POINT('Ctrl Pts',(18.5851405565408,0.189045441442997,3.40234596824686));
#36000=CARTESIAN_POINT('Ctrl Pts',(18.6010458352284,0.348682149221421,3.51777419717301));
#36001=CARTESIAN_POINT('Ctrl Pts',(18.6169511139161,0.508318856999844,3.63320242609916));
#36002=CARTESIAN_POINT('Ctrl Pts',(18.6328563926037,0.604944928113798,3.83577407466982));
#36003=CARTESIAN_POINT('Ctrl Pts',(18.6487616712913,0.594193758619731,4.03247681196108));
#36004=CARTESIAN_POINT('Ctrl Pts',(18.6646669499789,0.583442589125664,4.22917954925235));
#36005=CARTESIAN_POINT('Ctrl Pts',(18.6805722286665,0.465314179023576,4.42001337526422));
#36006=CARTESIAN_POINT('Ctrl Pts',(18.6964775073541,0.294048096631404,4.51735547060535));
#36007=CARTESIAN_POINT('Ctrl Pts',(18.7047032011502,0.205474838715737,4.56769764225005));
#36008=CARTESIAN_POINT('Ctrl Pts',(18.7129288949463,0.102689258835563,4.59303430424318));
#36009=CARTESIAN_POINT('Ctrl Pts',(18.7211545887425,-5.63168744233308E-5,
4.59312091231189));
#36010=CARTESIAN_POINT('Origin',(4.,0.,4.));
#36011=CARTESIAN_POINT('',(19.1288454112575,0.000222628893785728,4.59497983522242));
#36012=CARTESIAN_POINT('',(19.0211545887425,-0.000526118841417405,4.59432346427954));
#36013=CARTESIAN_POINT('',(4.,-7.27562663373442E-17,4.5941));
#36014=CARTESIAN_POINT('Ctrl Pts',(19.1288454112575,0.000222628893785728,
4.59497983522242));
#36015=CARTESIAN_POINT('Ctrl Pts',(19.1278571485589,0.012468395078646,4.59503853204781));
#36016=CARTESIAN_POINT('Ctrl Pts',(19.1268688858602,0.0247107891953784,
4.59469333777414));
#36017=CARTESIAN_POINT('Ctrl Pts',(19.1258806231615,0.0369274203756033,
4.59393377720877));
#36018=CARTESIAN_POINT('Ctrl Pts',(19.1099753444739,0.233544093050454,4.58170927203582));
#36019=CARTESIAN_POINT('Ctrl Pts',(19.0940700657862,0.423487581379576,4.46215450773496));
#36020=CARTESIAN_POINT('Ctrl Pts',(19.0781647870986,0.519543871337238,4.29016397409385));
#36021=CARTESIAN_POINT('Ctrl Pts',(19.062259508411,0.615600161294901,4.11817344045274));
#36022=CARTESIAN_POINT('Ctrl Pts',(19.0463542297234,0.617769252881104,3.89374713747137));
#36023=CARTESIAN_POINT('Ctrl Pts',(19.0304489510358,0.525055191022736,3.71993212880311));
#36024=CARTESIAN_POINT('Ctrl Pts',(19.0145436723482,0.432341129164367,3.54611712013485));
#36025=CARTESIAN_POINT('Ctrl Pts',(18.9986383936606,0.244743913861428,3.42291340577968));
#36026=CARTESIAN_POINT('Ctrl Pts',(18.982733114973,0.0484002497885746,3.40689091904056));
#36027=CARTESIAN_POINT('Ctrl Pts',(18.9668278362853,-0.147943414284278,
3.39086843230144));
#36028=CARTESIAN_POINT('Ctrl Pts',(18.9509225575977,-0.353033527127044,
3.48202717317836));
#36029=CARTESIAN_POINT('Ctrl Pts',(18.9350172789101,-0.472701385564812,
3.63851090447403));
#36030=CARTESIAN_POINT('Ctrl Pts',(18.9191120002225,-0.592369244002587,
3.79499463576972));
#36031=CARTESIAN_POINT('Ctrl Pts',(18.9032067215349,-0.626614848035354,
4.01680335748416));
#36032=CARTESIAN_POINT('Ctrl Pts',(18.8873014428473,-0.559714065105754,
4.20209188855652));
#36033=CARTESIAN_POINT('Ctrl Pts',(18.8713961641597,-0.492813282176159,
4.38738041962887));
#36034=CARTESIAN_POINT('Ctrl Pts',(18.8554908854721,-0.324766112284209,
4.53614876005914));
#36035=CARTESIAN_POINT('Ctrl Pts',(18.8395856067844,-0.132732706353525,
4.58008878179264));
#36036=CARTESIAN_POINT('Ctrl Pts',(18.8360055416088,-0.0895085590353085,
4.5899790920924));
#36037=CARTESIAN_POINT('Ctrl Pts',(18.8324254764332,-0.0450691735440342,
4.59455838259347));
#36038=CARTESIAN_POINT('Ctrl Pts',(18.8288454112575,-0.000545657836941327,
4.59414547262434));
#36039=CARTESIAN_POINT('Ctrl Pts',(18.7211545887425,-5.63168744233308E-5,
4.59312091231189));
#36040=CARTESIAN_POINT('Ctrl Pts',(18.728834173634,-0.0959805501911411,
4.59320177041728));
#36041=CARTESIAN_POINT('Ctrl Pts',(18.7365137585255,-0.191869914813978,
4.57127401300463));
#36042=CARTESIAN_POINT('Ctrl Pts',(18.744193343417,-0.276126457005151,4.5271386400555));
#36043=CARTESIAN_POINT('Ctrl Pts',(18.7600986221046,-0.450631173567243,
4.43572934949413));
#36044=CARTESIAN_POINT('Ctrl Pts',(18.7760039007922,-0.575236852009173,
4.249060403701));
#36045=CARTESIAN_POINT('Ctrl Pts',(18.7919091794798,-0.592729836422094,
4.05284228527226));
#36046=CARTESIAN_POINT('Ctrl Pts',(18.8078144581674,-0.610222820835014,
3.85662416684351));
#36047=CARTESIAN_POINT('Ctrl Pts',(18.823719736855,-0.520603111218926,3.65085687577915));
#36048=CARTESIAN_POINT('Ctrl Pts',(18.8396250155426,-0.365020286731977,
3.53002004684018));
#36049=CARTESIAN_POINT('Ctrl Pts',(18.8555302942302,-0.209437462245028,
3.40918321790122));
#36050=CARTESIAN_POINT('Ctrl Pts',(18.8714355729179,0.0121084771127808,
3.37327685108765));
#36051=CARTESIAN_POINT('Ctrl Pts',(18.8873408516055,0.197893008823487,3.43878763096633));
#36052=CARTESIAN_POINT('Ctrl Pts',(18.9032461302931,0.383677540534204,3.50429841084501));
#36053=CARTESIAN_POINT('Ctrl Pts',(18.9191514089807,0.533700664597814,3.67122633741595));
#36054=CARTESIAN_POINT('Ctrl Pts',(18.9350566876683,0.579078109400399,3.86292516893752));
#36055=CARTESIAN_POINT('Ctrl Pts',(18.9509619663559,0.624455554202981,4.05462400045908));
#36056=CARTESIAN_POINT('Ctrl Pts',(18.9668672450435,0.56518731974455,4.27109373693126));
#36057=CARTESIAN_POINT('Ctrl Pts',(18.9827725237311,0.428486871854059,4.41294063344238));
#36058=CARTESIAN_POINT('Ctrl Pts',(18.9955665454016,0.318526617336051,4.52704063153052));
#36059=CARTESIAN_POINT('Ctrl Pts',(19.008360567072,0.158464569423419,4.5928566151945));
#36060=CARTESIAN_POINT('Ctrl Pts',(19.0211545887425,-0.000526118841417405,
4.59432346427954));
#36061=CARTESIAN_POINT('Origin',(4.,0.,4.));
#36062=CARTESIAN_POINT('',(19.4288454112575,0.000431836873498515,4.59346738712276));
#36063=CARTESIAN_POINT('',(19.3211545887425,0.000315695961457875,4.59487351203822));
#36064=CARTESIAN_POINT('',(4.,-7.27562663373442E-17,4.5941));
#36065=CARTESIAN_POINT('Ctrl Pts',(19.4288454112575,0.000431836873498515,
4.59346738712276));
#36066=CARTESIAN_POINT('Ctrl Pts',(19.4232888206845,0.0697367837969298,
4.59393182999066));
#36067=CARTESIAN_POINT('Ctrl Pts',(19.4177322301115,0.13889623855249,4.58272225272434));
#36068=CARTESIAN_POINT('Ctrl Pts',(19.4121756395385,0.203565929825556,4.55917964700716));
#36069=CARTESIAN_POINT('Ctrl Pts',(19.3962703608509,0.38867754617092,4.49179089484985));
#36070=CARTESIAN_POINT('Ctrl Pts',(19.3803650821633,0.537002597765565,4.32335233206236));
#36071=CARTESIAN_POINT('Ctrl Pts',(19.3644598034757,0.580436494614329,4.13120381907284));
#36072=CARTESIAN_POINT('Ctrl Pts',(19.3485545247881,0.623870391463095,3.93905530608331));
#36073=CARTESIAN_POINT('Ctrl Pts',(19.3326492461004,0.562413133565966,3.72319684289176));
#36074=CARTESIAN_POINT('Ctrl Pts',(19.3167439674128,0.424283294458304,3.58274150440131));
#36075=CARTESIAN_POINT('Ctrl Pts',(19.3008386887252,0.286153455350651,3.44228616591086));
#36076=CARTESIAN_POINT('Ctrl Pts',(19.2849334100376,0.071351035032473,3.37723395212151));
#36077=CARTESIAN_POINT('Ctrl Pts',(19.26902813135,-0.12149578302492,3.4174540870367));
#36078=CARTESIAN_POINT('Ctrl Pts',(19.2531228526624,-0.314342601082313,
3.45767422195189));
#36079=CARTESIAN_POINT('Ctrl Pts',(19.2372175739748,-0.485233816878921,
3.60316670557164));
#36080=CARTESIAN_POINT('Ctrl Pts',(19.2213122952871,-0.555703413721375,
3.78712754492824));
#36081=CARTESIAN_POINT('Ctrl Pts',(19.2054070165995,-0.626173010563829,
3.97108838428485));
#36082=CARTESIAN_POINT('Ctrl Pts',(19.1895017379119,-0.59622098845213,4.19351757937831));
#36083=CARTESIAN_POINT('Ctrl Pts',(19.1735964592243,-0.479600048885993,
4.35228505390253));
#36084=CARTESIAN_POINT('Ctrl Pts',(19.1586794432354,-0.370225264934164,
4.50118762911129));
#36085=CARTESIAN_POINT('Ctrl Pts',(19.1437624272465,-0.184617181632464,
4.59409385471947));
#36086=CARTESIAN_POINT('Ctrl Pts',(19.1288454112575,0.000222628893785728,
4.59497983522242));
#36087=CARTESIAN_POINT('Ctrl Pts',(19.0211545887425,-0.000526118841417405,
4.59432346427954));
#36088=CARTESIAN_POINT('Ctrl Pts',(19.0242658457596,-0.0391895592568775,
4.59468017342281));
#36089=CARTESIAN_POINT('Ctrl Pts',(19.0273771027768,-0.0777896429211806,
4.59123148246997));
#36090=CARTESIAN_POINT('Ctrl Pts',(19.030488359794,-0.115590453236054,4.58374636034569));
#36091=CARTESIAN_POINT('Ctrl Pts',(19.0463936384816,-0.308834669113126,
4.5454811341878));
#36092=CARTESIAN_POINT('Ctrl Pts',(19.0622989171692,-0.481190439544719,
4.40172662532195));
#36093=CARTESIAN_POINT('Ctrl Pts',(19.0782041958568,-0.553519286527586,
4.21848882245705));
#36094=CARTESIAN_POINT('Ctrl Pts',(19.0941094745444,-0.625848133510457,
4.03525101959215));
#36095=CARTESIAN_POINT('Ctrl Pts',(19.1100147532321,-0.598150057044591,
3.81252992272818));
#36096=CARTESIAN_POINT('Ctrl Pts',(19.1259200319197,-0.483142842019737,
3.65258963701249));
#36097=CARTESIAN_POINT('Ctrl Pts',(19.1418253106073,-0.36813562699489,3.49264935129682));
#36098=CARTESIAN_POINT('Ctrl Pts',(19.1577305892949,-0.165819273411065,
3.39548987672941));
#36099=CARTESIAN_POINT('Ctrl Pts',(19.1736358679825,0.0309111084379188,
3.40572273351557));
#36100=CARTESIAN_POINT('Ctrl Pts',(19.1895411466701,0.227641490286902,3.41595559030173));
#36101=CARTESIAN_POINT('Ctrl Pts',(19.2054464253577,0.418785900401045,3.53358077844144));
#36102=CARTESIAN_POINT('Ctrl Pts',(19.2213517040453,0.516578912360374,3.70458978792342));
#36103=CARTESIAN_POINT('Ctrl Pts',(19.237256982733,0.614371924319703,3.87559879740541));
#36104=CARTESIAN_POINT('Ctrl Pts',(19.2531622614206,0.618813538124218,4.09999162822965));
#36105=CARTESIAN_POINT('Ctrl Pts',(19.2690675401082,0.527864352527146,4.27473658562515));
#36106=CARTESIAN_POINT('Ctrl Pts',(19.2849728187958,0.436915166930073,4.44948154302064));
#36107=CARTESIAN_POINT('Ctrl Pts',(19.3008780974834,0.250575181931413,4.5745786269874));
#36108=CARTESIAN_POINT('Ctrl Pts',(19.316783376171,0.0544038354309166,4.59258854924263));
#36109=CARTESIAN_POINT('Ctrl Pts',(19.3182404470282,0.0364327229714708,
4.59423842494573));
#36110=CARTESIAN_POINT('Ctrl Pts',(19.3196975178853,0.0183791031991185,
4.59498959766064));
#36111=CARTESIAN_POINT('Ctrl Pts',(19.3211545887425,0.000315695961457875,
4.59487351203822));
#36112=CARTESIAN_POINT('Origin',(4.,0.,4.));
#36113=CARTESIAN_POINT('',(19.7288454112575,-0.000401422265437046,4.59340756962635));
#36114=CARTESIAN_POINT('',(19.6211545887425,0.000364945106097663,4.59334757974602));
#36115=CARTESIAN_POINT('',(4.,-7.27562663373442E-17,4.5941));
#36116=CARTESIAN_POINT('Ctrl Pts',(19.7288454112575,-0.000401422265437046,
4.59340756962635));
#36117=CARTESIAN_POINT('Ctrl Pts',(19.7187204928102,0.125914276337785,4.59262579220321));
#36118=CARTESIAN_POINT('Ctrl Pts',(19.7085955743629,0.252675872983383,4.55317429478549));
#36119=CARTESIAN_POINT('Ctrl Pts',(19.6984706559155,0.353547469597214,4.47867015725961));
#36120=CARTESIAN_POINT('Ctrl Pts',(19.6825653772279,0.512007102052776,4.36163128164859));
#36121=CARTESIAN_POINT('Ctrl Pts',(19.6666600985403,0.606576931433326,4.15809158444534));
#36122=CARTESIAN_POINT('Ctrl Pts',(19.6507548198527,0.593834428727047,3.9615078130365));
#36123=CARTESIAN_POINT('Ctrl Pts',(19.6348495411651,0.581091926020768,3.76492404162769));
#36124=CARTESIAN_POINT('Ctrl Pts',(19.6189442624775,0.46103709122769,3.57529619601327));
#36125=CARTESIAN_POINT('Ctrl Pts',(19.6030389837899,0.288794059426421,3.47969339775167));
#36126=CARTESIAN_POINT('Ctrl Pts',(19.5871337051022,0.116551027625133,3.38409059949006));
#36127=CARTESIAN_POINT('Ctrl Pts',(19.5712284264146,-0.107880201184358,
3.38251284858128));
#36128=CARTESIAN_POINT('Ctrl Pts',(19.555323147727,-0.281450319664219,3.47568456171554));
#36129=CARTESIAN_POINT('Ctrl Pts',(19.5394178690394,-0.45502043814407,3.5688562748498));
#36130=CARTESIAN_POINT('Ctrl Pts',(19.5235125903518,-0.577729446294298,
3.75677745202708));
#36131=CARTESIAN_POINT('Ctrl Pts',(19.5076073116642,-0.593234549413986,
3.95316264945144));
#36132=CARTESIAN_POINT('Ctrl Pts',(19.4917020329766,-0.608739652533674,
4.1495478468758));
#36133=CARTESIAN_POINT('Ctrl Pts',(19.475796754289,-0.517040850622822,4.35439706454724));
#36134=CARTESIAN_POINT('Ctrl Pts',(19.4598914756013,-0.360242359119356,
4.47365220261941));
#36135=CARTESIAN_POINT('Ctrl Pts',(19.4495427874867,-0.258222223711561,
4.55124494740629));
#36136=CARTESIAN_POINT('Ctrl Pts',(19.4391940993721,-0.128642866595325,
4.59260240088276));
#36137=CARTESIAN_POINT('Ctrl Pts',(19.4288454112575,0.000431836873498515,
4.59346738712276));
#36138=CARTESIAN_POINT('Ctrl Pts',(19.3211545887425,0.000315695961457875,
4.59487351203822));
#36139=CARTESIAN_POINT('Ctrl Pts',(19.3356027965729,-0.178799726336078,
4.59372241551416));
#36140=CARTESIAN_POINT('Ctrl Pts',(19.3500510044034,-0.35887750705714,4.50729762043595));
#36141=CARTESIAN_POINT('Ctrl Pts',(19.3644992122339,-0.469016560662847,
4.36625733020606));
#36142=CARTESIAN_POINT('Ctrl Pts',(19.3804044909215,-0.590262902253753,
4.21099342837053));
#36143=CARTESIAN_POINT('Ctrl Pts',(19.3963097696091,-0.626752877433238,
3.98954286415574));
#36144=CARTESIAN_POINT('Ctrl Pts',(19.4122150482967,-0.561731832709929,
3.80358636875254));
#36145=CARTESIAN_POINT('Ctrl Pts',(19.4281203269843,-0.49671078798662,3.61762987334934));
#36146=CARTESIAN_POINT('Ctrl Pts',(19.4440256056719,-0.330178723360516,
3.46716744675772));
#36147=CARTESIAN_POINT('Ctrl Pts',(19.4599308843595,-0.138600118749324,
3.42128506802099));
#36148=CARTESIAN_POINT('Ctrl Pts',(19.4758361630471,0.0529784858618673,
3.37540268928427));
#36149=CARTESIAN_POINT('Ctrl Pts',(19.4917414417347,0.269603630458146,3.43410035840244));
#36150=CARTESIAN_POINT('Ctrl Pts',(19.5076467204224,0.411810215621333,3.57042659223364));
#36151=CARTESIAN_POINT('Ctrl Pts',(19.52355199911,0.554016800784528,3.70675282606484));
#36152=CARTESIAN_POINT('Ctrl Pts',(19.5394572777976,0.621804826514621,3.92070762460909));
#36153=CARTESIAN_POINT('Ctrl Pts',(19.5553625564852,0.584048894878601,4.11405198996909));
#36154=CARTESIAN_POINT('Ctrl Pts',(19.5712678351728,0.546292963242583,4.30739635532907));
#36155=CARTESIAN_POINT('Ctrl Pts',(19.5871731138604,0.402993074240464,4.4801302875048));
#36156=CARTESIAN_POINT('Ctrl Pts',(19.6030783925481,0.219946482677819,4.55294168410437));
#36157=CARTESIAN_POINT('Ctrl Pts',(19.6091037912795,0.150602919307179,4.5805248346624));
#36158=CARTESIAN_POINT('Ctrl Pts',(19.615129190011,0.0755552166468998,4.59376787586841));
#36159=CARTESIAN_POINT('Ctrl Pts',(19.6211545887425,0.000364945106097663,
4.59334757974602));
#36160=CARTESIAN_POINT('Origin',(4.,0.,4.));
#36161=CARTESIAN_POINT('',(20.0288454112575,-0.000266600559035268,4.5949350414008));
#36162=CARTESIAN_POINT('',(19.9211545887425,-0.000461335262921832,4.59353843444423));
#36163=CARTESIAN_POINT('',(4.,-7.27562663373442E-17,4.5941));
#36164=CARTESIAN_POINT('Ctrl Pts',(20.0288454112575,-0.000266600559035268,
4.5949350414008));
#36165=CARTESIAN_POINT('Ctrl Pts',(20.0141521649359,0.181839152323842,4.59391190659116));
#36166=CARTESIAN_POINT('Ctrl Pts',(19.9994589186142,0.364814066967773,4.50413264800542));
#36167=CARTESIAN_POINT('Ctrl Pts',(19.9847656722925,0.474598868642052,4.35899217880197));
#36168=CARTESIAN_POINT('Ctrl Pts',(19.9688603936049,0.593439717564554,4.20187920587587));
#36169=CARTESIAN_POINT('Ctrl Pts',(19.9529551149173,0.626517665065843,3.97989492921597));
#36170=CARTESIAN_POINT('Ctrl Pts',(19.9370498362297,0.558641803885684,3.79496194153783));
#36171=CARTESIAN_POINT('Ctrl Pts',(19.9211445575421,0.490765942705524,3.61002895385969));
#36172=CARTESIAN_POINT('Ctrl Pts',(19.9052392788545,0.321936272843916,3.46214725516331));
#36173=CARTESIAN_POINT('Ctrl Pts',(19.8893340001669,0.129673778938228,3.41921955761011));
#36174=CARTESIAN_POINT('Ctrl Pts',(19.8734287214793,-0.0625887149674591,
3.37629186005692));
#36175=CARTESIAN_POINT('Ctrl Pts',(19.8575234427916,-0.278284032917226,
3.43831816364691));
#36176=CARTESIAN_POINT('Ctrl Pts',(19.841618164104,-0.418374827314372,3.57681771754473));
#36177=CARTESIAN_POINT('Ctrl Pts',(19.8257128854164,-0.558465621711518,
3.71531727144255));
#36178=CARTESIAN_POINT('Ctrl Pts',(19.8098076067288,-0.622951892556044,
3.9302900756482));
#36179=CARTESIAN_POINT('Ctrl Pts',(19.7939023280412,-0.58222383973146,4.12303018792675));
#36180=CARTESIAN_POINT('Ctrl Pts',(19.7779970493536,-0.541495786906873,
4.3157703002053));
#36181=CARTESIAN_POINT('Ctrl Pts',(19.762091770666,-0.395553410413165,4.48627772055676));
#36182=CARTESIAN_POINT('Ctrl Pts',(19.7461864919784,-0.211407504401025,
4.55626240372308));
#36183=CARTESIAN_POINT('Ctrl Pts',(19.7404061317381,-0.144484459893097,
4.58169651826758));
#36184=CARTESIAN_POINT('Ctrl Pts',(19.7346257714978,-0.0725156072563085,
4.59385388977766));
#36185=CARTESIAN_POINT('Ctrl Pts',(19.7288454112575,-0.000401422265437046,
4.59340756962635));
#36186=CARTESIAN_POINT('Ctrl Pts',(19.6211545887425,0.000364945106097663,
4.59334757974602));
#36187=CARTESIAN_POINT('Ctrl Pts',(19.6310344686986,-0.122924963130536,
4.59265841784648));
#36188=CARTESIAN_POINT('Ctrl Pts',(19.6409143486547,-0.246598186964828,
4.55523353708024));
#36189=CARTESIAN_POINT('Ctrl Pts',(19.6507942286109,-0.346136160298313,
4.48405653351353));
#36190=CARTESIAN_POINT('Ctrl Pts',(19.6666995072985,-0.506378917588675,
4.36947112529969));
#36191=CARTESIAN_POINT('Ctrl Pts',(19.6826047859861,-0.60407113804621,4.16741144784858));
#36192=CARTESIAN_POINT('Ctrl Pts',(19.6985100646737,-0.5943566574826,3.97065479758251));
#36193=CARTESIAN_POINT('Ctrl Pts',(19.7144153433613,-0.584642176918989,
3.77389814731645));
#36194=CARTESIAN_POINT('Ctrl Pts',(19.7303206220489,-0.467520995334232,
3.58244452423543));
#36195=CARTESIAN_POINT('Ctrl Pts',(19.7462259007365,-0.296770260159971,
3.48420125495101));
#36196=CARTESIAN_POINT('Ctrl Pts',(19.7621311794242,-0.12601952498572,3.38595798566659));
#36197=CARTESIAN_POINT('Ctrl Pts',(19.7780364581118,0.098360763778029,3.38092507017875));
#36198=CARTESIAN_POINT('Ctrl Pts',(19.7939417367994,0.27334477570878,3.47141355644931));
#36199=CARTESIAN_POINT('Ctrl Pts',(19.809847015487,0.448328787639532,3.56190204271987));
#36200=CARTESIAN_POINT('Ctrl Pts',(19.8257522941746,0.573916522737285,3.74791193074883));
#36201=CARTESIAN_POINT('Ctrl Pts',(19.8416575728622,0.592443207149574,3.9440350735258));
#36202=CARTESIAN_POINT('Ctrl Pts',(19.8575628515498,0.610969891561863,4.14015821630277));
#36203=CARTESIAN_POINT('Ctrl Pts',(19.8734681302375,0.522435525288687,4.34639461382776));
#36204=CARTESIAN_POINT('Ctrl Pts',(19.8893734089251,0.367491719635661,4.46804975837363));
#36205=CARTESIAN_POINT('Ctrl Pts',(19.8999671355309,0.264291244586565,4.54907828775811));
#36206=CARTESIAN_POINT('Ctrl Pts',(19.9105608621367,0.131629953687138,4.59258455010229));
#36207=CARTESIAN_POINT('Ctrl Pts',(19.9211545887425,-0.000461335262921832,
4.59353843444423));
#36208=CARTESIAN_POINT('Origin',(4.,0.,4.));
#36209=CARTESIAN_POINT('',(20.3288454112575,0.000547175593784699,4.59423670486774));
#36210=CARTESIAN_POINT('',(20.2211545887425,-0.000159442692484791,4.59503650419094));
#36211=CARTESIAN_POINT('',(4.,-7.27562663373442E-17,4.5941));
#36212=CARTESIAN_POINT('Ctrl Pts',(20.3288454112575,0.000547175593784699,
4.59423670486774));
#36213=CARTESIAN_POINT('Ctrl Pts',(20.3254891157492,0.0422991098545892,
4.59465405164581));
#36214=CARTESIAN_POINT('Ctrl Pts',(20.3221328202408,0.0839734681026259,
4.59066114403672));
#36215=CARTESIAN_POINT('Ctrl Pts',(20.3187765247324,0.124636177719752,4.58197547152207));
#36216=CARTESIAN_POINT('Ctrl Pts',(20.3028712460448,0.317334266145104,4.54081460186972));
#36217=CARTESIAN_POINT('Ctrl Pts',(20.2869659673572,0.48731321493246,4.39426577643889));
#36218=CARTESIAN_POINT('Ctrl Pts',(20.2710606886696,0.556778600406793,4.20989870881916));
#36219=CARTESIAN_POINT('Ctrl Pts',(20.255155409982,0.626243985881127,4.02553164119943));
#36220=CARTESIAN_POINT('Ctrl Pts',(20.2392501312944,0.595195808042437,3.80334633139079));
#36221=CARTESIAN_POINT('Ctrl Pts',(20.2233448526068,0.477757630702126,3.64521515909767));
#36222=CARTESIAN_POINT('Ctrl Pts',(20.2074395739191,0.360319453361808,3.48708398680455));
#36223=CARTESIAN_POINT('Ctrl Pts',(20.1915342952315,0.156491276519859,3.39300695202695));
#36224=CARTESIAN_POINT('Ctrl Pts',(20.1756290165439,-0.04006765138094,3.40625706061923));
#36225=CARTESIAN_POINT('Ctrl Pts',(20.1597237378563,-0.236626579281727,
3.4195071692115));
#36226=CARTESIAN_POINT('Ctrl Pts',(20.1438184591687,-0.425916258241364,
3.54008442117362));
#36227=CARTESIAN_POINT('Ctrl Pts',(20.1279131804811,-0.521059912873915,
3.71258420787224));
#36228=CARTESIAN_POINT('Ctrl Pts',(20.1120079017935,-0.616203567506467,
3.88508399457085));
#36229=CARTESIAN_POINT('Ctrl Pts',(20.0961026231058,-0.617201197811932,
4.10950631600596));
#36230=CARTESIAN_POINT('Ctrl Pts',(20.0801973444182,-0.523575121773085,
4.28282745216878));
#36231=CARTESIAN_POINT('Ctrl Pts',(20.0642920657306,-0.429949045734243,
4.45614858833159));
#36232=CARTESIAN_POINT('Ctrl Pts',(20.048386787043,-0.241699263351099,4.57836853922213));
#36233=CARTESIAN_POINT('Ctrl Pts',(20.0324815083554,-0.0452724969876719,
4.59335768007126));
#36234=CARTESIAN_POINT('Ctrl Pts',(20.0312694759895,-0.030304158296608,
4.59449989984645));
#36235=CARTESIAN_POINT('Ctrl Pts',(20.0300574436235,-0.0152883365109376,
4.5950194388496));
#36236=CARTESIAN_POINT('Ctrl Pts',(20.0288454112575,-0.000266600559035268,
4.5949350414008));
#36237=CARTESIAN_POINT('Ctrl Pts',(19.9211545887425,-0.000461335262921832,
4.59353843444423));
#36238=CARTESIAN_POINT('Ctrl Pts',(19.9264661408243,-0.0666901315043342,
4.5940166992278));
#36239=CARTESIAN_POINT('Ctrl Pts',(19.9317776929061,-0.132775635823809,
4.58379778651276));
#36240=CARTESIAN_POINT('Ctrl Pts',(19.9370892449879,-0.194932679790098,
4.56224768701753));
#36241=CARTESIAN_POINT('Ctrl Pts',(19.9529945236755,-0.381060028529917,
4.49771657954882));
#36242=CARTESIAN_POINT('Ctrl Pts',(19.9688998023631,-0.531961480976676,
4.33158047304464));
#36243=CARTESIAN_POINT('Ctrl Pts',(19.9848050810507,-0.578348134104426,
4.14012389605102));
#36244=CARTESIAN_POINT('Ctrl Pts',(20.0007103597384,-0.624734787232175,
3.94866731905739));
#36245=CARTESIAN_POINT('Ctrl Pts',(20.016615638426,-0.566606641040915,3.73189027157431));
#36246=CARTESIAN_POINT('Ctrl Pts',(20.0325209171136,-0.430656211588969,
3.58932409618151));
#36247=CARTESIAN_POINT('Ctrl Pts',(20.0484261958012,-0.294705782137024,
3.44675792078871));
#36248=CARTESIAN_POINT('Ctrl Pts',(20.0643314744888,-0.080933069424392,
3.37840261748619));
#36249=CARTESIAN_POINT('Ctrl Pts',(20.0802367531764,0.112511319004002,3.41565067076361));
#36250=CARTESIAN_POINT('Ctrl Pts',(20.096142031864,0.305955707432406,3.45289872404102));
#36251=CARTESIAN_POINT('Ctrl Pts',(20.1120473105516,0.479071771576571,3.59575013389837));
#36252=CARTESIAN_POINT('Ctrl Pts',(20.1279525892393,0.552362916535151,3.77860107435498));
#36253=CARTESIAN_POINT('Ctrl Pts',(20.1438578679269,0.625654061493722,3.96145201481158));
#36254=CARTESIAN_POINT('Ctrl Pts',(20.1597631466145,0.599120287266732,4.18430248586742));
#36255=CARTESIAN_POINT('Ctrl Pts',(20.1756684253021,0.484961816589866,4.3448525870839));
#36256=CARTESIAN_POINT('Ctrl Pts',(20.1908304797822,0.376137759761604,4.49790047950022));
#36257=CARTESIAN_POINT('Ctrl Pts',(20.2059925342623,0.187686755696174,4.59433432972249));
#36258=CARTESIAN_POINT('Ctrl Pts',(20.2211545887425,-0.000159442692484791,
4.59503650419094));
#36259=CARTESIAN_POINT('Origin',(4.,0.,4.));
#36260=CARTESIAN_POINT('',(20.6288454112575,1.84392275237588E-6,4.59415158619139));
#36261=CARTESIAN_POINT('',(20.5211545887425,0.00014515264107467,4.59408556636595));
#36262=CARTESIAN_POINT('',(4.,-7.27562663373442E-17,4.5941));
#36263=CARTESIAN_POINT('Ctrl Pts',(20.6288454112575,1.84392275237588E-6,
4.59415158619139));
#36264=CARTESIAN_POINT('Ctrl Pts',(20.6209207878748,0.0985777406598016,
4.59414764832452));
#36265=CARTESIAN_POINT('Ctrl Pts',(20.6129961644921,0.197149291092008,4.56908802213256));
#36266=CARTESIAN_POINT('Ctrl Pts',(20.6050715411094,0.283761277174982,4.52200793915563));
#36267=CARTESIAN_POINT('Ctrl Pts',(20.5971189017656,0.370679463050262,4.47476141372331));
#36268=CARTESIAN_POINT('Ctrl Pts',(20.5891662624218,0.445553373684486,4.40533845822152));
#36269=CARTESIAN_POINT('Ctrl Pts',(20.581213623078,0.499196468040806,4.3222224876916));
#36270=CARTESIAN_POINT('Ctrl Pts',(20.5732609837342,0.552839562397126,4.23910651716169));
#36271=CARTESIAN_POINT('Ctrl Pts',(20.5653083443904,0.585251840475543,4.14229753160364));
#36272=CARTESIAN_POINT('Ctrl Pts',(20.5573557050466,0.592531230276538,4.04364021904617));
#36273=CARTESIAN_POINT('Ctrl Pts',(20.5494030657028,0.599810620077534,3.9449829064887));
#36274=CARTESIAN_POINT('Ctrl Pts',(20.541450426359,0.581957121601108,3.84447726693182));
#36275=CARTESIAN_POINT('Ctrl Pts',(20.5334977870152,0.541038843355354,3.75439549632807));
#36276=CARTESIAN_POINT('Ctrl Pts',(20.5255451476714,0.5001205651096,3.66431372572433));
#36277=CARTESIAN_POINT('Ctrl Pts',(20.5175925083276,0.436137507094518,3.58465582407373));
#36278=CARTESIAN_POINT('Ctrl Pts',(20.5096398689838,0.357128912623608,3.5251911792601));
#36279=CARTESIAN_POINT('Ctrl Pts',(20.50168722964,0.278120318152698,3.46572653444646));
#36280=CARTESIAN_POINT('Ctrl Pts',(20.4937345902962,0.184086187225959,3.42645514646979));
#36281=CARTESIAN_POINT('Ctrl Pts',(20.4857819509524,0.0861162623359374,
3.4121221101222));
#36282=CARTESIAN_POINT('Ctrl Pts',(20.4778293116085,-0.0118536625540841,
3.39778907377461));
#36283=CARTESIAN_POINT('Ctrl Pts',(20.4698766722647,-0.113759381407388,
3.4083943890561));
#36284=CARTESIAN_POINT('Ctrl Pts',(20.4619240329209,-0.206384677702653,
3.44274365129583));
#36285=CARTESIAN_POINT('Ctrl Pts',(20.4539713935771,-0.299009973997917,
3.47709291353557));
#36286=CARTESIAN_POINT('Ctrl Pts',(20.4460187542333,-0.382354847735142,
3.53518612273354));
#36287=CARTESIAN_POINT('Ctrl Pts',(20.4380661148895,-0.447563842371028,
3.60976099223211));
#36288=CARTESIAN_POINT('Ctrl Pts',(20.4301134755457,-0.512772837006921,
3.68433586173069));
#36289=CARTESIAN_POINT('Ctrl Pts',(20.4221608362019,-0.559845952541473,
3.77539239152987));
#36290=CARTESIAN_POINT('Ctrl Pts',(20.4142081968581,-0.580888308445953,
3.87190852591559));
#36291=CARTESIAN_POINT('Ctrl Pts',(20.3983029181705,-0.622973020254908,
4.06494079468701));
#36292=CARTESIAN_POINT('Ctrl Pts',(20.3823976394829,-0.5609346935436,4.27981148180459));
#36293=CARTESIAN_POINT('Ctrl Pts',(20.3664923607953,-0.422206916156273,
4.41936036842645));
#36294=CARTESIAN_POINT('Ctrl Pts',(20.353943377616,-0.312753156865475,4.52946196836027));
#36295=CARTESIAN_POINT('Ctrl Pts',(20.3413943944368,-0.155560747392339,
4.59267627084609));
#36296=CARTESIAN_POINT('Ctrl Pts',(20.3288454112575,0.000547175593784699,
4.59423670486774));
#36297=CARTESIAN_POINT('Ctrl Pts',(20.2211545887425,-0.000159442692484791,
4.59503650419094));
#36298=CARTESIAN_POINT('Ctrl Pts',(20.22189781295,-0.00936741923094289,
4.59507092387091));
#36299=CARTESIAN_POINT('Ctrl Pts',(20.2226410371574,-0.0185739425223631,
4.59487531632137));
#36300=CARTESIAN_POINT('Ctrl Pts',(20.2233842613649,-0.0277695625699301,
4.59444507412072));
#36301=CARTESIAN_POINT('Ctrl Pts',(20.2392895400526,-0.224559303926058,
4.58523772856393));
#36302=CARTESIAN_POINT('Ctrl Pts',(20.2551948187402,-0.416355619511548,
4.46857330607325));
#36303=CARTESIAN_POINT('Ctrl Pts',(20.2711000974278,-0.51503297954037,4.29810345018796));
#36304=CARTESIAN_POINT('Ctrl Pts',(20.2870053761154,-0.613710339569191,
4.12763359430267));
#36305=CARTESIAN_POINT('Ctrl Pts',(20.302910654803,-0.619268744041345,3.90335830502277));
#36306=CARTESIAN_POINT('Ctrl Pts',(20.3188159334906,-0.529271009537506,
3.72809546473432));
#36307=CARTESIAN_POINT('Ctrl Pts',(20.3347212121782,-0.439273275033663,
3.55283262444587));
#36308=CARTESIAN_POINT('Ctrl Pts',(20.3506264908658,-0.253719401553817,
3.42658223314887));
#36309=CARTESIAN_POINT('Ctrl Pts',(20.3665317695535,-0.0575887485100287,
3.40762076142476));
#36310=CARTESIAN_POINT('Ctrl Pts',(20.3824370482411,0.138541904533748,3.38865928970065));
#36311=CARTESIAN_POINT('Ctrl Pts',(20.3983423269287,0.345249337141466,3.47698673754941));
#36312=CARTESIAN_POINT('Ctrl Pts',(20.4142476056163,0.467192899405167,3.63141813202173));
#36313=CARTESIAN_POINT('Ctrl Pts',(20.4301528843039,0.589136461668875,3.78584952649406));
#36314=CARTESIAN_POINT('Ctrl Pts',(20.4460581629915,0.626316153588557,4.00638486758996));
#36315=CARTESIAN_POINT('Ctrl Pts',(20.4619634416791,0.562534942182983,4.19337293359078));
#36316=CARTESIAN_POINT('Ctrl Pts',(20.4699160810229,0.530644336480201,4.28686696659118));
#36317=CARTESIAN_POINT('Ctrl Pts',(20.4778687203667,0.473513504946115,4.3719741808178));
#36318=CARTESIAN_POINT('Ctrl Pts',(20.4858213597105,0.400240502138227,4.43864269813793));
#36319=CARTESIAN_POINT('Ctrl Pts',(20.4937739990544,0.326967499330329,4.50531121545807));
#36320=CARTESIAN_POINT('Ctrl Pts',(20.5017266383982,0.237552325248626,4.55354103587171));
#36321=CARTESIAN_POINT('Ctrl Pts',(20.509679277742,0.141619450488441,4.57712494713439));
#36322=CARTESIAN_POINT('Ctrl Pts',(20.5135043814088,0.0954771353210092,
4.58846846487098));
#36323=CARTESIAN_POINT('Ctrl Pts',(20.5173294850756,0.0478269697500401,
4.59411022582368));
#36324=CARTESIAN_POINT('Ctrl Pts',(20.5211545887425,0.00014515264107467,
4.59408556636595));
#36325=CARTESIAN_POINT('Origin',(4.,0.,4.));
#36326=CARTESIAN_POINT('',(20.9288454112575,-6.4040329070536E-6,4.59405282094147));
#36327=CARTESIAN_POINT('',(20.8211545887425,5.65245430726296E-6,4.59414685459231));
#36328=CARTESIAN_POINT('',(4.,-7.27562663373442E-17,4.5941));
#36329=CARTESIAN_POINT('Ctrl Pts',(20.9288454112575,-6.4040329070536E-6,
4.59405282094147));
#36330=CARTESIAN_POINT('Ctrl Pts',(20.9243050993443,0.0564994875152707,
4.59403151438501));
#36331=CARTESIAN_POINT('Ctrl Pts',(20.9197647874311,0.113011285737041,4.58603249222448));
#36332=CARTESIAN_POINT('Ctrl Pts',(20.9152244755179,0.167207550221224,4.57013805289591));
#36333=CARTESIAN_POINT('Ctrl Pts',(20.9072718361741,0.262135685878584,4.5422979516059));
#36334=CARTESIAN_POINT('Ctrl Pts',(20.8993191968303,0.349959832061366,4.49023494241839));
#36335=CARTESIAN_POINT('Ctrl Pts',(20.8913665574865,0.419942299057043,4.42031443844746));
#36336=CARTESIAN_POINT('Ctrl Pts',(20.8834139181427,0.489924766052721,4.35039393447653));
#36337=CARTESIAN_POINT('Ctrl Pts',(20.8754612787989,0.542065553861293,4.26261593572219));
#36338=CARTESIAN_POINT('Ctrl Pts',(20.8675086394551,0.569989725359365,4.16771249585991));
#36339=CARTESIAN_POINT('Ctrl Pts',(20.8595560001113,0.597913896857441,4.07280905599763));
#36340=CARTESIAN_POINT('Ctrl Pts',(20.8516033607674,0.601621452045013,3.97078017502742));
#36341=CARTESIAN_POINT('Ctrl Pts',(20.8436507214236,0.580659121393648,3.87410027737825));
#36342=CARTESIAN_POINT('Ctrl Pts',(20.8356980820798,0.559696790742287,3.77742037972911));
#36343=CARTESIAN_POINT('Ctrl Pts',(20.827745442736,0.514064574252002,3.686089465401));
#36344=CARTESIAN_POINT('Ctrl Pts',(20.8197928033922,0.44934157601673,3.61127397478397));
#36345=CARTESIAN_POINT('Ctrl Pts',(20.8118401640484,0.384618577781443,3.53645848416692));
#36346=CARTESIAN_POINT('Ctrl Pts',(20.8038875247046,0.300804797801161,3.47815841726095));
#36347=CARTESIAN_POINT('Ctrl Pts',(20.7959348853608,0.208147717693743,3.44350176598286));
#36348=CARTESIAN_POINT('Ctrl Pts',(20.787982246017,0.115490637586335,3.40884511470477));
#36349=CARTESIAN_POINT('Ctrl Pts',(20.7800296066732,0.0139902573517945,
3.39783187905454));
#36350=CARTESIAN_POINT('Ctrl Pts',(20.7720769673294,-0.0839438183138644,
3.41180854931868));
#36351=CARTESIAN_POINT('Ctrl Pts',(20.7641243279856,-0.181877893979523,
3.42578521958283));
#36352=CARTESIAN_POINT('Ctrl Pts',(20.7561716886418,-0.2762456650763,3.46475179576135));
#36353=CARTESIAN_POINT('Ctrl Pts',(20.748219049298,-0.355509010203556,3.52394413563581));
#36354=CARTESIAN_POINT('Ctrl Pts',(20.7402664099542,-0.434772355330821,
3.58313647551028));
#36355=CARTESIAN_POINT('Ctrl Pts',(20.7323137706103,-0.498931274488562,
3.66255457908069));
#36356=CARTESIAN_POINT('Ctrl Pts',(20.7243611312665,-0.54014217617541,3.75248840252759));
#36357=CARTESIAN_POINT('Ctrl Pts',(20.7164084919227,-0.581353077862249,
3.84242222597448));
#36358=CARTESIAN_POINT('Ctrl Pts',(20.7084558525789,-0.599615962078206,
3.94287176929784));
#36359=CARTESIAN_POINT('Ctrl Pts',(20.7005032132351,-0.592696601504336,
4.0415558946729));
#36360=CARTESIAN_POINT('Ctrl Pts',(20.6925505738913,-0.585777240930466,
4.14024002004797));
#36361=CARTESIAN_POINT('Ctrl Pts',(20.6845979345475,-0.553675635566762,
4.23715872747472));
#36362=CARTESIAN_POINT('Ctrl Pts',(20.6766452952037,-0.50031917594212,4.32046203197985));
#36363=CARTESIAN_POINT('Ctrl Pts',(20.6686926558599,-0.446962716317479,
4.40376533648498));
#36364=CARTESIAN_POINT('Ctrl Pts',(20.6607400165161,-0.3723514024319,4.47345323806848));
#36365=CARTESIAN_POINT('Ctrl Pts',(20.6527873771723,-0.285602702553558,
4.52100610813718));
#36366=CARTESIAN_POINT('Ctrl Pts',(20.6448347378285,-0.198854002675205,
4.56855897820588));
#36367=CARTESIAN_POINT('Ctrl Pts',(20.6368820984847,-0.099967916804087,
4.59397681675976));
#36368=CARTESIAN_POINT('Ctrl Pts',(20.6289294591409,-0.00104364331035449,
4.59415068835528));
#36369=CARTESIAN_POINT('Ctrl Pts',(20.6289014431798,-0.000695147863829354,
4.59415130087895));
#36370=CARTESIAN_POINT('Ctrl Pts',(20.6288734272186,-0.000346651943377611,
4.59415160011295));
#36371=CARTESIAN_POINT('Ctrl Pts',(20.6288454112575,1.84392275237588E-6,
4.59415158619139));
#36372=CARTESIAN_POINT('Ctrl Pts',(20.5211545887425,0.00014515264107467,
4.59408556636595));
#36373=CARTESIAN_POINT('Ctrl Pts',(20.5252821244194,-0.0513066296901884,
4.59405895720698));
#36374=CARTESIAN_POINT('Ctrl Pts',(20.5294096600964,-0.102795266482965,
4.58743447362686));
#36375=CARTESIAN_POINT('Ctrl Pts',(20.5335371957734,-0.152465997634008,
4.57425651377355));
#36376=CARTESIAN_POINT('Ctrl Pts',(20.5414898351172,-0.248167995557571,
4.5488661670383));
#36377=CARTESIAN_POINT('Ctrl Pts',(20.549442474461,-0.33712141596603,4.49914747145609));
#36378=CARTESIAN_POINT('Ctrl Pts',(20.5573951138048,-0.408848640915227,
4.43107686705031));
#36379=CARTESIAN_POINT('Ctrl Pts',(20.5653477531486,-0.480575865864423,
4.36300626264453));
#36380=CARTESIAN_POINT('Ctrl Pts',(20.5733003924924,-0.535076895354358,
4.27658374941519));
#36381=CARTESIAN_POINT('Ctrl Pts',(20.5812530318362,-0.565476628275392,
4.18243021985824));
#36382=CARTESIAN_POINT('Ctrl Pts',(20.58920567118,-0.595876361196427,4.08827669030129));
#36383=CARTESIAN_POINT('Ctrl Pts',(20.5971583105238,-0.602174797548561,
3.98639214441672));
#36384=CARTESIAN_POINT('Ctrl Pts',(20.6051109498677,-0.58371402745925,3.88920441471463));
#36385=CARTESIAN_POINT('Ctrl Pts',(20.6130635892115,-0.565253257369939,
3.79201668501254));
#36386=CARTESIAN_POINT('Ctrl Pts',(20.6210162285553,-0.522033280839182,
3.69952577149293));
#36387=CARTESIAN_POINT('Ctrl Pts',(20.6289688678991,-0.459278917219465,
3.62305528060961));
#36388=CARTESIAN_POINT('Ctrl Pts',(20.6369215072429,-0.396524553599749,
3.54658478972629));
#36389=CARTESIAN_POINT('Ctrl Pts',(20.6448741465867,-0.314235802891072,
3.48613472147926));
#36390=CARTESIAN_POINT('Ctrl Pts',(20.6528267859305,-0.222505051509483,
3.44908779917463));
#36391=CARTESIAN_POINT('Ctrl Pts',(20.6607794252743,-0.130774300127894,
3.41204087687));
#36392=CARTESIAN_POINT('Ctrl Pts',(20.6687320646181,-0.029601548073392,
3.39839710050778));
#36393=CARTESIAN_POINT('Ctrl Pts',(20.6766847039619,0.0686601223983595,
3.40982890848785));
#36394=CARTESIAN_POINT('Ctrl Pts',(20.6846373433057,0.1669217928701,3.42126071646792));
#36395=CARTESIAN_POINT('Ctrl Pts',(20.6925899826495,0.262272381759091,3.45776810879028));
#36396=CARTESIAN_POINT('Ctrl Pts',(20.7005426219933,0.343045155251024,3.51488528173127));
#36397=CARTESIAN_POINT('Ctrl Pts',(20.7084952613371,0.423817928742975,3.57200245467228));
#36398=CARTESIAN_POINT('Ctrl Pts',(20.7164479006809,0.490012886837861,3.64972940823193));
#36399=CARTESIAN_POINT('Ctrl Pts',(20.7244005400247,0.533541468465666,3.73856417004634));
#36400=CARTESIAN_POINT('Ctrl Pts',(20.7323531793686,0.577070050093471,3.82739893186076));
#36401=CARTESIAN_POINT('Ctrl Pts',(20.7403058187123,0.597932255254196,3.92734150192994));
#36402=CARTESIAN_POINT('Ctrl Pts',(20.7482584580562,0.593574919799613,4.02617190099588));
#36403=CARTESIAN_POINT('Ctrl Pts',(20.7562110974,0.589217584345031,4.1250023000618));
#36404=CARTESIAN_POINT('Ctrl Pts',(20.7641637367438,0.559640708275147,4.22272052812447));
#36405=CARTESIAN_POINT('Ctrl Pts',(20.7721163760876,0.508461778515953,4.30737953925928));
#36406=CARTESIAN_POINT('Ctrl Pts',(20.7800690154314,0.457282848756759,4.39203855039408));
#36407=CARTESIAN_POINT('Ctrl Pts',(20.7880216547752,0.384501865308254,4.46363834460102));
#36408=CARTESIAN_POINT('Ctrl Pts',(20.795974294119,0.299016600344635,4.51342469267633));
#36409=CARTESIAN_POINT('Ctrl Pts',(20.8039269334628,0.213531335381016,4.56321104075164));
#36410=CARTESIAN_POINT('Ctrl Pts',(20.8118795728066,0.115341788902283,4.59118394269532));
#36411=CARTESIAN_POINT('Ctrl Pts',(20.8198322121504,0.0164533379892873,
4.59392342516246));
#36412=CARTESIAN_POINT('Ctrl Pts',(20.8202730043478,0.0109722321971217,
4.59407526688998));
#36413=CARTESIAN_POINT('Ctrl Pts',(20.8207137965451,0.00548897925183007,
4.59414958726715));
#36414=CARTESIAN_POINT('Ctrl Pts',(20.8211545887425,5.65245430726296E-6,
4.59414685459231));
#36415=CARTESIAN_POINT('Origin',(4.,0.,4.));
#36416=CARTESIAN_POINT('',(21.2288454112575,1.28243205298473E-5,4.59412621697841));
#36417=CARTESIAN_POINT('',(21.1211545887425,-1.09306879613159E-5,4.5940621922514));
#36418=CARTESIAN_POINT('',(4.,-7.27562663373442E-17,4.5941));
#36419=CARTESIAN_POINT('Ctrl Pts',(21.2288454112575,1.28243205298473E-5,
4.59412621697841));
#36420=CARTESIAN_POINT('Ctrl Pts',(21.2276894108138,0.0143945780386088,
4.59413985249388));
#36421=CARTESIAN_POINT('Ctrl Pts',(21.2265334103701,0.028775363636007,4.59362827285675));
#36422=CARTESIAN_POINT('Ctrl Pts',(21.2253774099263,0.043117441953227,4.59258471957415));
#36423=CARTESIAN_POINT('Ctrl Pts',(21.2174247705826,0.141782954511012,4.58540565408365));
#36424=CARTESIAN_POINT('Ctrl Pts',(21.2094721312387,0.238616577754522,4.55305001116024));
#36425=CARTESIAN_POINT('Ctrl Pts',(21.2015194918949,0.321779082392626,4.49947370882601));
#36426=CARTESIAN_POINT('Ctrl Pts',(21.1935668525511,0.404941587030731,4.44589740649178));
#36427=CARTESIAN_POINT('Ctrl Pts',(21.1856142132073,0.474432973063433,4.37110044474674));
#36428=CARTESIAN_POINT('Ctrl Pts',(21.1776615738635,0.521756972098598,4.28422777087894));
#36429=CARTESIAN_POINT('Ctrl Pts',(21.1697089345197,0.569080971133768,4.19735509701114));
#36430=CARTESIAN_POINT('Ctrl Pts',(21.1617562951759,0.594237583171398,4.09840671102057));
#36431=CARTESIAN_POINT('Ctrl Pts',(21.1538036558321,0.594151069756079,3.9994804007435));
#36432=CARTESIAN_POINT('Ctrl Pts',(21.1458510164883,0.59406455634076,3.90055409046644));
#36433=CARTESIAN_POINT('Ctrl Pts',(21.1378983771445,0.568734917472505,3.80164985590287));
#36434=CARTESIAN_POINT('Ctrl Pts',(21.1299457378007,0.521259046500119,3.71486008677882));
#36435=CARTESIAN_POINT('Ctrl Pts',(21.1219930984569,0.473783175527722,3.62807031765475));
#36436=CARTESIAN_POINT('Ctrl Pts',(21.114040459113,0.40416107245118,3.5533950139702));
#36437=CARTESIAN_POINT('Ctrl Pts',(21.1060878197692,0.320904987578411,3.49996424865404));
#36438=CARTESIAN_POINT('Ctrl Pts',(21.0981351804254,0.237648902705652,3.44653348333788));
#36439=CARTESIAN_POINT('Ctrl Pts',(21.0901825410817,0.140758836036697,3.41434725639011));
#36440=CARTESIAN_POINT('Ctrl Pts',(21.0822299017378,0.042080917889342,3.40734077242984));
#36441=CARTESIAN_POINT('Ctrl Pts',(21.074277262394,-0.056597000258024,3.40033428846957));
#36442=CARTESIAN_POINT('Ctrl Pts',(21.0663246230502,-0.157062769883762,
3.41850754749682));
#36443=CARTESIAN_POINT('Ctrl Pts',(21.0583719837064,-0.247033082431791,
3.45963862106718));
#36444=CARTESIAN_POINT('Ctrl Pts',(21.0504193443626,-0.337003394979799,
3.50076969463752));
#36445=CARTESIAN_POINT('Ctrl Pts',(21.0424667050188,-0.416478250450111,
3.56485858275095));
#36446=CARTESIAN_POINT('Ctrl Pts',(21.034514065675,-0.475740765152555,3.644069545988));
#36447=CARTESIAN_POINT('Ctrl Pts',(21.0265614263312,-0.535003279855012,
3.72328050922507));
#36448=CARTESIAN_POINT('Ctrl Pts',(21.0186087869874,-0.574053453789596,
3.81761354758578));
#36449=CARTESIAN_POINT('Ctrl Pts',(21.0106561476436,-0.588116871685884,
3.91553516229212));
#36450=CARTESIAN_POINT('Ctrl Pts',(21.0027035082998,-0.60218028958217,4.01345677699845));
#36451=CARTESIAN_POINT('Ctrl Pts',(20.994750868956,-0.591256951440166,4.11496696805043));
#36452=CARTESIAN_POINT('Ctrl Pts',(20.9867982296121,-0.556682383467722,
4.20765473214191));
#36453=CARTESIAN_POINT('Ctrl Pts',(20.9788455902683,-0.522107815495282,
4.30034249623339));
#36454=CARTESIAN_POINT('Ctrl Pts',(20.9708929509246,-0.463882017692404,
4.38420783336438));
#36455=CARTESIAN_POINT('Ctrl Pts',(20.9629403115808,-0.389123888092725,
4.4489970636758));
#36456=CARTESIAN_POINT('Ctrl Pts',(20.9549876722369,-0.314365758493028,
4.51378629398723));
#36457=CARTESIAN_POINT('Ctrl Pts',(20.9470350328931,-0.223075297096518,
4.5594994174791));
#36458=CARTESIAN_POINT('Ctrl Pts',(20.9390823935493,-0.12641400383229,4.58054738252877));
#36459=CARTESIAN_POINT('Ctrl Pts',(20.9356700661187,-0.0849384674446181,
4.58957866703598));
#36460=CARTESIAN_POINT('Ctrl Pts',(20.9322577386881,-0.0424741039190781,
4.59406883414683));
#36461=CARTESIAN_POINT('Ctrl Pts',(20.9288454112575,-6.4040329070536E-6,
4.59405282094147));
#36462=CARTESIAN_POINT('Ctrl Pts',(20.8211545887425,5.65245430726296E-6,
4.59414685459231));
#36463=CARTESIAN_POINT('Ctrl Pts',(20.8286664358889,-0.0934395423672534,
4.59410028517524));
#36464=CARTESIAN_POINT('Ctrl Pts',(20.8361782830354,-0.18690618531264,4.57167601133058));
#36465=CARTESIAN_POINT('Ctrl Pts',(20.8436901301818,-0.270133012248912,
4.529191754035));
#36466=CARTESIAN_POINT('Ctrl Pts',(20.8516427695256,-0.358243556226857,
4.4842145374498));
#36467=CARTESIAN_POINT('Ctrl Pts',(20.8595954088694,-0.434877288835492,
4.41675404128879));
#36468=CARTESIAN_POINT('Ctrl Pts',(20.8675480482133,-0.490664589397756,
4.33505825661903));
#36469=CARTESIAN_POINT('Ctrl Pts',(20.8755006875571,-0.546451889960021,
4.25336247194927));
#36470=CARTESIAN_POINT('Ctrl Pts',(20.8834533269009,-0.581392758475918,
4.15743139877076));
#36471=CARTESIAN_POINT('Ctrl Pts',(20.8914059662447,-0.591215252505097,
4.05899390323763));
#36472=CARTESIAN_POINT('Ctrl Pts',(20.8993586055885,-0.601037746534278,
3.96055640770449));
#36473=CARTESIAN_POINT('Ctrl Pts',(20.9073112449323,-0.585741866076735,
3.85961248981672));
#36474=CARTESIAN_POINT('Ctrl Pts',(20.9152638842761,-0.547197711916726,
3.76850392583047));
#36475=CARTESIAN_POINT('Ctrl Pts',(20.9232165236199,-0.508653557756717,
3.67739536184422));
#36476=CARTESIAN_POINT('Ctrl Pts',(20.9311691629637,-0.446861129894262,
3.59612215175949));
#36477=CARTESIAN_POINT('Ctrl Pts',(20.9391218023075,-0.369375409551539,
3.53462104847409));
#36478=CARTESIAN_POINT('Ctrl Pts',(20.9470744416513,-0.291889689208826,
3.4731199451887));
#36479=CARTESIAN_POINT('Ctrl Pts',(20.9550270809951,-0.198710676385865,
3.43139094870266));
#36480=CARTESIAN_POINT('Ctrl Pts',(20.9629797203389,-0.101230766359376,
3.41453599926792));
#36481=CARTESIAN_POINT('Ctrl Pts',(20.9709323596827,-0.00375085633288601,
3.39768104983318));
#36482=CARTESIAN_POINT('Ctrl Pts',(20.9788849990265,0.0980299508971346,
3.40570014744973));
#36483=CARTESIAN_POINT('Ctrl Pts',(20.9868376383704,0.191667561123074,3.43761284710704));
#36484=CARTESIAN_POINT('Ctrl Pts',(20.9947902777142,0.285305171349014,3.46952554676435));
#36485=CARTESIAN_POINT('Ctrl Pts',(21.002742917058,0.37079958457088,3.52533184846243));
#36486=CARTESIAN_POINT('Ctrl Pts',(21.0106955564018,0.437697946637459,3.59820867233944));
#36487=CARTESIAN_POINT('Ctrl Pts',(21.0186481957456,0.504596308704037,3.67108549621644));
#36488=CARTESIAN_POINT('Ctrl Pts',(21.0266008350894,0.552898619615334,3.76103284227238));
#36489=CARTESIAN_POINT('Ctrl Pts',(21.0345534744332,0.576699262792956,3.8570534220826));
#36490=CARTESIAN_POINT('Ctrl Pts',(21.042506113777,0.600499905970578,3.95307400189282));
#36491=CARTESIAN_POINT('Ctrl Pts',(21.0504587531208,0.599798881414527,4.05516781545734));
#36492=CARTESIAN_POINT('Ctrl Pts',(21.0584113924646,0.574681899562831,4.15085250374278));
#36493=CARTESIAN_POINT('Ctrl Pts',(21.0663640318084,0.549564917711138,4.24653719202821));
#36494=CARTESIAN_POINT('Ctrl Pts',(21.0743166711522,0.500031978563804,4.33581275503458));
#36495=CARTESIAN_POINT('Ctrl Pts',(21.082269310496,0.432139158218639,4.40776403918836));
#36496=CARTESIAN_POINT('Ctrl Pts',(21.0902219498398,0.364246337873458,4.47971532334216));
#36497=CARTESIAN_POINT('Ctrl Pts',(21.0981745891836,0.277993636330433,4.53434232864337));
#36498=CARTESIAN_POINT('Ctrl Pts',(21.1061272285274,0.183926621270441,4.56496615973523));
#36499=CARTESIAN_POINT('Ctrl Pts',(21.1111363485991,0.124676735433976,4.5842551580617));
#36500=CARTESIAN_POINT('Ctrl Pts',(21.1161454686708,0.0623266393968894,
4.59402126159141));
#36501=CARTESIAN_POINT('Ctrl Pts',(21.1211545887425,-1.09306879613159E-5,
4.5940621922514));
#36502=CARTESIAN_POINT('Origin',(4.,0.,4.));
#36503=CARTESIAN_POINT('',(21.5288454112575,-1.51073027558624E-5,4.59408477831653));
#36504=CARTESIAN_POINT('',(21.4211545887425,1.51733402061755E-5,4.59410821609125));
#36505=CARTESIAN_POINT('',(4.,-7.27562663373442E-17,4.5941));
#36506=CARTESIAN_POINT('Ctrl Pts',(21.5288454112575,-1.51073027558624E-5,
4.59408477831653));
#36507=CARTESIAN_POINT('Ctrl Pts',(21.5231210829395,0.0712153309254728,
4.59401644885886));
#36508=CARTESIAN_POINT('Ctrl Pts',(21.5173967546214,0.142469702059594,4.58119587380047));
#36509=CARTESIAN_POINT('Ctrl Pts',(21.5116724263034,0.209120766622247,4.55613331912479));
#36510=CARTESIAN_POINT('Ctrl Pts',(21.5037197869596,0.301717111362981,4.52131465616629));
#36511=CARTESIAN_POINT('Ctrl Pts',(21.4957671476158,0.385428743083265,4.46286809139133));
#36512=CARTESIAN_POINT('Ctrl Pts',(21.4878145082719,0.450020774675764,4.38793951336988));
#36513=CARTESIAN_POINT('Ctrl Pts',(21.4798618689281,0.514612806268249,4.31301093534845));
#36514=CARTESIAN_POINT('Ctrl Pts',(21.4719092295843,0.560085237732952,4.22160034408054));
#36515=CARTESIAN_POINT('Ctrl Pts',(21.4639565902405,0.58087844500124,4.1248839293359));
#36516=CARTESIAN_POINT('Ctrl Pts',(21.4560039508967,0.601671652269532,4.02816751459124));
#36517=CARTESIAN_POINT('Ctrl Pts',(21.4480513115529,0.597785635341394,3.92614527636987));
#36518=CARTESIAN_POINT('Ctrl Pts',(21.4400986722091,0.569695512712777,3.83129082280931));
#36519=CARTESIAN_POINT('Ctrl Pts',(21.4321460328653,0.541605390084162,3.73643636924876));
#36520=CARTESIAN_POINT('Ctrl Pts',(21.4241933935215,0.489311161755075,3.64874970034904));
#36521=CARTESIAN_POINT('Ctrl Pts',(21.4162407541777,0.419206509371839,3.57895170565158));
#36522=CARTESIAN_POINT('Ctrl Pts',(21.4082881148339,0.349101856988603,3.50915371095413));
#36523=CARTESIAN_POINT('Ctrl Pts',(21.4003354754901,0.261186780551223,3.45724439045894));
#36524=CARTESIAN_POINT('Ctrl Pts',(21.3923828361463,0.16621009553345,3.42957036558731));
#36525=CARTESIAN_POINT('Ctrl Pts',(21.3844301968025,0.0712334105156764,
3.40189634071567));
#36526=CARTESIAN_POINT('Ctrl Pts',(21.3764775574587,-0.0308048830825163,
3.3984576114676));
#36527=CARTESIAN_POINT('Ctrl Pts',(21.3685249181149,-0.127429214135013,
3.41967460932821));
#36528=CARTESIAN_POINT('Ctrl Pts',(21.360572278771,-0.22405354518751,3.44089160718882));
#36529=CARTESIAN_POINT('Ctrl Pts',(21.3526196394272,-0.315263913694308,
3.4867643321581));
#36530=CARTESIAN_POINT('Ctrl Pts',(21.3446670000834,-0.389908609845283,
3.5516842188346));
#36531=CARTESIAN_POINT('Ctrl Pts',(21.3367143607396,-0.464553305996249,
3.6166041055111));
#36532=CARTESIAN_POINT('Ctrl Pts',(21.3287617213958,-0.522632329791381,
3.70057115389483));
#36533=CARTESIAN_POINT('Ctrl Pts',(21.320809082052,-0.557044729551177,3.79331924871262));
#36534=CARTESIAN_POINT('Ctrl Pts',(21.3128564427082,-0.591457129310977,
3.88606734353042));
#36535=CARTESIAN_POINT('Ctrl Pts',(21.3049038033644,-0.602202905035458,
3.9875964847823));
#36536=CARTESIAN_POINT('Ctrl Pts',(21.2969511640206,-0.587968239287942,
4.08549335215105));
#36537=CARTESIAN_POINT('Ctrl Pts',(21.2889985246768,-0.573733573540424,
4.18339021951981));
#36538=CARTESIAN_POINT('Ctrl Pts',(21.281045885333,-0.534518466320906,4.27765481300544));
#36539=CARTESIAN_POINT('Ctrl Pts',(21.2730932459892,-0.47511749858569,4.35676200219639));
#36540=CARTESIAN_POINT('Ctrl Pts',(21.2651406066454,-0.415716530850488,
4.43586919138732));
#36541=CARTESIAN_POINT('Ctrl Pts',(21.2571879673016,-0.336129702599601,
4.49981897628356));
#36542=CARTESIAN_POINT('Ctrl Pts',(21.2492353279577,-0.246087587538132,
4.54079262470289));
#36543=CARTESIAN_POINT('Ctrl Pts',(21.2424386890577,-0.169134048541188,
4.57581031891556));
#36544=CARTESIAN_POINT('Ctrl Pts',(21.2356420501576,-0.0845438791841879,
4.59404604774026));
#36545=CARTESIAN_POINT('Ctrl Pts',(21.2288454112575,1.28243205298473E-5,
4.59412621697841));
#36546=CARTESIAN_POINT('Ctrl Pts',(21.1211545887425,-1.09306879613159E-5,
4.5940621922514));
#36547=CARTESIAN_POINT('Ctrl Pts',(21.1240981080146,-0.0366424819978743,
4.5940862444172));
#36548=CARTESIAN_POINT('Ctrl Pts',(21.1270416272867,-0.0732697079540161,
4.59075208378119));
#36549=CARTESIAN_POINT('Ctrl Pts',(21.1299851465589,-0.109260984540888,
4.58401866488291));
#36550=CARTESIAN_POINT('Ctrl Pts',(21.1379377859027,-0.20650024671525,4.56582668205621));
#36551=CARTESIAN_POINT('Ctrl Pts',(21.1458904252465,-0.299097442487026,
4.52282205952027));
#36552=CARTESIAN_POINT('Ctrl Pts',(21.1538430645903,-0.375731303474415,
4.46026269810429));
#36553=CARTESIAN_POINT('Ctrl Pts',(21.1617957039341,-0.452365164461805,
4.3977033366883));
#36554=CARTESIAN_POINT('Ctrl Pts',(21.1697483432779,-0.513035690664809,
4.31558923639226));
#36555=CARTESIAN_POINT('Ctrl Pts',(21.1777009826217,-0.550325083965727,
4.22395996434209));
#36556=CARTESIAN_POINT('Ctrl Pts',(21.1856536219655,-0.587614477266646,
4.13233069229192));
#36557=CARTESIAN_POINT('Ctrl Pts',(21.1936062613093,-0.601522737665479,
4.03118624848761));
#36558=CARTESIAN_POINT('Ctrl Pts',(21.2015589006531,-0.590349390887683,
3.93289291874755));
#36559=CARTESIAN_POINT('Ctrl Pts',(21.2095115399969,-0.579176044109886,
3.83459958900749));
#36560=CARTESIAN_POINT('Ctrl Pts',(21.2174641793407,-0.542921090155459,
3.73915737333167));
#36561=CARTESIAN_POINT('Ctrl Pts',(21.2254168186845,-0.486017190935348,
3.65823538248142));
#36562=CARTESIAN_POINT('Ctrl Pts',(21.2333694580283,-0.429113291715238,
3.57731339163117));
#36563=CARTESIAN_POINT('Ctrl Pts',(21.2413220973721,-0.351560447229444,
3.51091162560648));
#36564=CARTESIAN_POINT('Ctrl Pts',(21.249274736716,-0.262840548960938,3.46714860467879));
#36565=CARTESIAN_POINT('Ctrl Pts',(21.2572273760598,-0.174120650692433,
3.4233855837511));
#36566=CARTESIAN_POINT('Ctrl Pts',(21.2651800154036,-0.0742336986412151,
3.40226130792041));
#36567=CARTESIAN_POINT('Ctrl Pts',(21.2731326547474,0.0246077668693877,
3.40635850761334));
#36568=CARTESIAN_POINT('Ctrl Pts',(21.2810852940912,0.123449232380002,3.41045570730627));
#36569=CARTESIAN_POINT('Ctrl Pts',(21.289037933435,0.221245211350001,3.43977438252282));
#36570=CARTESIAN_POINT('Ctrl Pts',(21.2969905727788,0.306038813396919,3.49072992590572));
#36571=CARTESIAN_POINT('Ctrl Pts',(21.3049432121226,0.390832415443818,3.54168546928862));
#36572=CARTESIAN_POINT('Ctrl Pts',(21.3128958514664,0.462623640567642,3.61427788083785));
#36573=CARTESIAN_POINT('Ctrl Pts',(21.3208484908102,0.512635033719562,3.69963174955258));
#36574=CARTESIAN_POINT('Ctrl Pts',(21.328801130154,0.562646426871494,3.78498561826733));
#36575=CARTESIAN_POINT('Ctrl Pts',(21.3367537694978,0.590877988051513,3.88310094414759));
#36576=CARTESIAN_POINT('Ctrl Pts',(21.3447064088416,0.59387802439953,3.98198179230066));
#36577=CARTESIAN_POINT('Ctrl Pts',(21.3526590481854,0.596878060747546,4.08086264045372));
#36578=CARTESIAN_POINT('Ctrl Pts',(21.3606116875293,0.574646572263566,4.1805090108796));
#36579=CARTESIAN_POINT('Ctrl Pts',(21.3685643268731,0.529901661201384,4.26873777763737));
#36580=CARTESIAN_POINT('Ctrl Pts',(21.3765169662169,0.485156750139203,4.35696654439514));
#36581=CARTESIAN_POINT('Ctrl Pts',(21.3844696055607,0.417898416498819,4.4337777074848));
#36582=CARTESIAN_POINT('Ctrl Pts',(21.3924222449045,0.336349907607971,4.48978005607163));
#36583=CARTESIAN_POINT('Ctrl Pts',(21.4003748842483,0.254801398717122,4.54578240465847));
#36584=CARTESIAN_POINT('Ctrl Pts',(21.4083275235921,0.158962714575808,4.58097593874246));
#36585=CARTESIAN_POINT('Ctrl Pts',(21.4162801629359,0.0605514396169286,
4.59105776945554));
#36586=CARTESIAN_POINT('Ctrl Pts',(21.4179049715381,0.0404449719157324,
4.59311759444699));
#36587=CARTESIAN_POINT('Ctrl Pts',(21.4195297801403,0.0202311170044278,
4.59412918598148));
#36588=CARTESIAN_POINT('Ctrl Pts',(21.4211545887425,1.51733402061755E-5,
4.59410821609125));
#36589=CARTESIAN_POINT('Origin',(4.,0.,4.));
#36590=CARTESIAN_POINT('',(21.8288454112575,1.47252919898561E-5,4.59408074293421));
#36591=CARTESIAN_POINT('',(21.7211545887425,-1.54601956517634E-5,4.59410286710644));
#36592=CARTESIAN_POINT('',(4.,-7.27562663373442E-17,4.5941));
#36593=CARTESIAN_POINT('Ctrl Pts',(21.8288454112575,1.47252919898561E-5,
4.59408074293421));
#36594=CARTESIAN_POINT('Ctrl Pts',(21.826505394409,0.0291331941223908,4.59410767674242));
#36595=CARTESIAN_POINT('Ctrl Pts',(21.8241653775604,0.0582478076928112,
4.59200528777341));
#36596=CARTESIAN_POINT('Ctrl Pts',(21.8218253607118,0.0870422430987805,
4.58774093918134));
#36597=CARTESIAN_POINT('Ctrl Pts',(21.813872721368,0.184901264939656,4.57324838268129));
#36598=CARTESIAN_POINT('Ctrl Pts',(21.8059200820242,0.279062206656402,4.53378504179028));
#36599=CARTESIAN_POINT('Ctrl Pts',(21.7979674426804,0.358012610677869,4.47417584741217));
#36600=CARTESIAN_POINT('Ctrl Pts',(21.7900148033366,0.436963014699336,4.41456665303406));
#36601=CARTESIAN_POINT('Ctrl Pts',(21.7820621639928,0.500702881025523,4.33481160516884));
#36602=CARTESIAN_POINT('Ctrl Pts',(21.774109524649,0.541439142878506,4.24466184465998));
#36603=CARTESIAN_POINT('Ctrl Pts',(21.7661568853052,0.58217540473149,4.15451208415111));
#36604=CARTESIAN_POINT('Ctrl Pts',(21.7582042459614,0.599908062111268,4.0539676109986));
#36605=CARTESIAN_POINT('Ctrl Pts',(21.7502516066176,0.59246905613922,3.95532135643358));
#36606=CARTESIAN_POINT('Ctrl Pts',(21.7422989672738,0.585030050167171,3.85667510186855));
#36607=CARTESIAN_POINT('Ctrl Pts',(21.73434632793,0.552419380843296,3.759927065891));
#36608=CARTESIAN_POINT('Ctrl Pts',(21.7263936885861,0.498624146640836,3.67690601358098));
#36609=CARTESIAN_POINT('Ctrl Pts',(21.7184410492423,0.444828912438376,3.59388496127097));
#36610=CARTESIAN_POINT('Ctrl Pts',(21.7104884098985,0.369849113357332,3.52459089262848));
#36611=CARTESIAN_POINT('Ctrl Pts',(21.7025357705547,0.28285205103972,3.47749595131133));
#36612=CARTESIAN_POINT('Ctrl Pts',(21.6945831312109,0.195854988722108,3.43040100999418));
#36613=CARTESIAN_POINT('Ctrl Pts',(21.6866304918671,0.0968406631679286,
3.40550519600236));
#36614=CARTESIAN_POINT('Ctrl Pts',(21.6786778525233,-0.00208507577578169,
3.40585236167057));
#36615=CARTESIAN_POINT('Ctrl Pts',(21.6707252131795,-0.101010814719503,
3.40619952733877));
#36616=CARTESIAN_POINT('Ctrl Pts',(21.6627725738357,-0.199847967052756,
3.431789672667));
#36617=CARTESIAN_POINT('Ctrl Pts',(21.6548199344919,-0.28651234476781,3.47949405385809));
#36618=CARTESIAN_POINT('Ctrl Pts',(21.6468672951481,-0.373176722482865,
3.52719843504918));
#36619=CARTESIAN_POINT('Ctrl Pts',(21.6389146558043,-0.44766832557972,3.59701705210314));
#36620=CARTESIAN_POINT('Ctrl Pts',(21.6309620164605,-0.500879541024521,
3.68041362817464));
#36621=CARTESIAN_POINT('Ctrl Pts',(21.6230093771167,-0.55409075646931,3.76381020424612));
#36622=CARTESIAN_POINT('Ctrl Pts',(21.6150567377728,-0.586021584262053,
3.86078473933514));
#36623=CARTESIAN_POINT('Ctrl Pts',(21.607104098429,-0.592768045815946,3.95948077576042));
#36624=CARTESIAN_POINT('Ctrl Pts',(21.5991514590852,-0.599514507369841,
4.05817681218572));
#36625=CARTESIAN_POINT('Ctrl Pts',(21.5911988197414,-0.581076602684875,
4.15859434994728));
#36626=CARTESIAN_POINT('Ctrl Pts',(21.5832461803976,-0.539708616728004,
4.24845597739434));
#36627=CARTESIAN_POINT('Ctrl Pts',(21.5752935410538,-0.498340630771147,
4.33831760484137));
#36628=CARTESIAN_POINT('Ctrl Pts',(21.56734090171,-0.434042563542403,4.41762332197391));
#36629=CARTESIAN_POINT('Ctrl Pts',(21.5593882623662,-0.354675729482573,
4.47667692475034));
#36630=CARTESIAN_POINT('Ctrl Pts',(21.5514356230224,-0.275308895422716,
4.53573052752678));
#36631=CARTESIAN_POINT('Ctrl Pts',(21.5434829836786,-0.180873294531764,
4.57453201594709));
#36632=CARTESIAN_POINT('Ctrl Pts',(21.5355303443348,-0.0829149652056982,
4.58833737958621));
#36633=CARTESIAN_POINT('Ctrl Pts',(21.533302033309,-0.055467269432644,4.59220561033096));
#36634=CARTESIAN_POINT('Ctrl Pts',(21.5310737222833,-0.0277430016607059,
4.5941113769453));
#36635=CARTESIAN_POINT('Ctrl Pts',(21.5288454112575,-1.51073027558624E-5,
4.59408477831653));
#36636=CARTESIAN_POINT('Ctrl Pts',(21.4211545887425,1.51733402061755E-5,
4.59410821609125));
#36637=CARTESIAN_POINT('Ctrl Pts',(21.4274824194841,-0.0787159889745399,
4.59402654867773));
#36638=CARTESIAN_POINT('Ctrl Pts',(21.4338102502257,-0.15747883181342,4.57828382012605));
#36639=CARTESIAN_POINT('Ctrl Pts',(21.4401380809673,-0.230053504748576,
4.54780575811717));
#36640=CARTESIAN_POINT('Ctrl Pts',(21.4480907203111,-0.321263308378747,
4.50950178872359));
#36641=CARTESIAN_POINT('Ctrl Pts',(21.4560433596549,-0.402699049862651,
4.44792372259427));
#36642=CARTESIAN_POINT('Ctrl Pts',(21.4639959989987,-0.464404100671371,
4.37060031698995));
#36643=CARTESIAN_POINT('Ctrl Pts',(21.4719486383425,-0.526109151480106,
4.2932769113856));
#36644=CARTESIAN_POINT('Ctrl Pts',(21.4799012776864,-0.568083511613643,
4.20020816630624));
#36645=CARTESIAN_POINT('Ctrl Pts',(21.4878539170302,-0.585195243866348,
4.10277300340868));
#36646=CARTESIAN_POINT('Ctrl Pts',(21.495806556374,-0.602306976119048,4.00533784051114));
#36647=CARTESIAN_POINT('Ctrl Pts',(21.5037591957178,-0.594556080490919,
3.90353625979537));
#36648=CARTESIAN_POINT('Ctrl Pts',(21.5117118350616,-0.562890209537588,
3.80981489101362));
#36649=CARTESIAN_POINT('Ctrl Pts',(21.5196644744054,-0.53122433858425,3.71609352223184));
#36650=CARTESIAN_POINT('Ctrl Pts',(21.5276171137492,-0.47564349230572,3.63045236538409));
#36651=CARTESIAN_POINT('Ctrl Pts',(21.535569753093,-0.402943186155437,3.56336221830407));
#36652=CARTESIAN_POINT('Ctrl Pts',(21.5435223924368,-0.330242880005154,
3.49627207122406));
#36653=CARTESIAN_POINT('Ctrl Pts',(21.5514750317806,-0.24042311398314,3.44773293391182));
#36654=CARTESIAN_POINT('Ctrl Pts',(21.5594276711244,-0.144465577806233,
3.42367937699355));
#36655=CARTESIAN_POINT('Ctrl Pts',(21.5673803104682,-0.0485080416293372,
3.39962582007528));
#36656=CARTESIAN_POINT('Ctrl Pts',(21.575332949812,0.0535872647024426,3.40005784355098));
#36657=CARTESIAN_POINT('Ctrl Pts',(21.5832855891558,0.149337799479898,3.42492262666669));
#36658=CARTESIAN_POINT('Ctrl Pts',(21.5912382284996,0.245088334257342,3.44978740978241));
#36659=CARTESIAN_POINT('Ctrl Pts',(21.5991908678434,0.33449409748049,3.49908495253815));
#36660=CARTESIAN_POINT('Ctrl Pts',(21.6071435071872,0.406624016913212,3.56678795891296));
#36661=CARTESIAN_POINT('Ctrl Pts',(21.6150961465311,0.478753936345942,3.63449096528778));
#36662=CARTESIAN_POINT('Ctrl Pts',(21.6230487858749,0.533608011988269,3.72059943528167));
#36663=CARTESIAN_POINT('Ctrl Pts',(21.6310014252187,0.564479585995414,3.81458543566408));
#36664=CARTESIAN_POINT('Ctrl Pts',(21.6389540645625,0.595351160002559,3.90857143604649));
#36665=CARTESIAN_POINT('Ctrl Pts',(21.6469067039063,0.602240232374519,4.0104349668174));
#36666=CARTESIAN_POINT('Ctrl Pts',(21.6548593432501,0.584304520186539,4.10772182398666));
#36667=CARTESIAN_POINT('Ctrl Pts',(21.6628119825939,0.566368807998562,4.2050086811559));
#36668=CARTESIAN_POINT('Ctrl Pts',(21.6707646219377,0.523608311250652,4.29771886472347));
#36669=CARTESIAN_POINT('Ctrl Pts',(21.6787172612815,0.461251083056512,4.37451729206089));
#36670=CARTESIAN_POINT('Ctrl Pts',(21.6866699006253,0.398893854862358,4.45131571939834));
#36671=CARTESIAN_POINT('Ctrl Pts',(21.6946225399691,0.316939895221968,4.51220239050563));
#36672=CARTESIAN_POINT('Ctrl Pts',(21.7025751793129,0.225409191891896,4.54973308058009));
#36673=CARTESIAN_POINT('Ctrl Pts',(21.7087683157894,0.15412944274098,4.5789601931952));
#36674=CARTESIAN_POINT('Ctrl Pts',(21.7149614522659,0.0770418275534371,
4.59402294959611));
#36675=CARTESIAN_POINT('Ctrl Pts',(21.7211545887425,-1.54601956517634E-5,
4.59410286710644));
#36676=CARTESIAN_POINT('Origin',(4.,0.,4.));
#36677=CARTESIAN_POINT('',(22.1288454112575,-1.19684274697274E-5,4.59413016891312));
#36678=CARTESIAN_POINT('',(22.0211545887425,1.20066176157995E-5,4.59406577061205));
#36679=CARTESIAN_POINT('',(4.,-7.27562663373442E-17,4.5941));
#36680=CARTESIAN_POINT('Ctrl Pts',(22.1288454112575,-1.19684274697274E-5,
4.59413016891312));
#36681=CARTESIAN_POINT('Ctrl Pts',(22.1219370665346,0.0859328098890183,
4.59405244111828));
#36682=CARTESIAN_POINT('Ctrl Pts',(22.1150287218117,0.171910584533005,4.57519344187135));
#36683=CARTESIAN_POINT('Ctrl Pts',(22.1081203770888,0.24987714748571,4.53905210772026));
#36684=CARTESIAN_POINT('Ctrl Pts',(22.100167737745,0.339629466009183,4.49744749656716));
#36685=CARTESIAN_POINT('Ctrl Pts',(22.0922150984012,0.418765494330909,4.4329406966096));
#36686=CARTESIAN_POINT('Ctrl Pts',(22.0842624590574,0.477609775176754,4.35341854270704));
#36687=CARTESIAN_POINT('Ctrl Pts',(22.0763098197136,0.536454056022584,4.2738963888045));
#36688=CARTESIAN_POINT('Ctrl Pts',(22.0683571803698,0.575006589392542,4.17935888095698));
#36689=CARTESIAN_POINT('Ctrl Pts',(22.060404541026,0.588553803007579,4.081364517074));
#36690=CARTESIAN_POINT('Ctrl Pts',(22.0524519016822,0.60210101662262,3.983370153191));
#36691=CARTESIAN_POINT('Ctrl Pts',(22.0444992623384,0.590642910482727,3.88191893327255));
#36692=CARTESIAN_POINT('Ctrl Pts',(22.0365466229946,0.55558039411957,3.78941465069146));
#36693=CARTESIAN_POINT('Ctrl Pts',(22.0285939836508,0.520517877756421,3.69691036811039));
#36694=CARTESIAN_POINT('Ctrl Pts',(22.020641344307,0.461850951170019,3.61335302286667));
#36695=CARTESIAN_POINT('Ctrl Pts',(22.0126887049632,0.386752445163155,3.5489586384446));
#36696=CARTESIAN_POINT('Ctrl Pts',(22.0047360656194,0.311653939156274,3.48456425402251));
#36697=CARTESIAN_POINT('Ctrl Pts',(21.9967834262756,0.220123853728924,3.43933283042207));
#36698=CARTESIAN_POINT('Ctrl Pts',(21.9888307869318,0.123352988439278,3.41879452521803));
#36699=CARTESIAN_POINT('Ctrl Pts',(21.980878147588,0.0265821231496428,3.398256220014));
#36700=CARTESIAN_POINT('Ctrl Pts',(21.9729255082441,-0.075429522002288,
3.40241103320635));
#36701=CARTESIAN_POINT('Ctrl Pts',(21.9649728689003,-0.170209634025949,
3.43075098229493));
#36702=CARTESIAN_POINT('Ctrl Pts',(21.9570202295565,-0.26498974604961,3.4590909313835));
#36703=CARTESIAN_POINT('Ctrl Pts',(21.9490675902127,-0.352538324945002,
3.5116160163683));
#36704=CARTESIAN_POINT('Ctrl Pts',(21.9411149508689,-0.422151364554475,
3.58190433023263));
#36705=CARTESIAN_POINT('Ctrl Pts',(21.9331623115251,-0.491764404163956,
3.65219264409696));
#36706=CARTESIAN_POINT('Ctrl Pts',(21.9252096721813,-0.543441904487514,
3.74024418684083));
#36707=CARTESIAN_POINT('Ctrl Pts',(21.9172570328375,-0.570865587277161,
3.83529345812586));
#36708=CARTESIAN_POINT('Ctrl Pts',(21.9093043934937,-0.598289270066803,
3.93034272941087));
#36709=CARTESIAN_POINT('Ctrl Pts',(21.9013517541499,-0.601459135322544,
4.03238972923704));
#36710=CARTESIAN_POINT('Ctrl Pts',(21.8933991148061,-0.579987623844179,
4.12895782202339));
#36711=CARTESIAN_POINT('Ctrl Pts',(21.8854464754623,-0.558516112365809,
4.22552591480976));
#36712=CARTESIAN_POINT('Ctrl Pts',(21.8774938361185,-0.512403224153321,
4.31661510055631));
#36713=CARTESIAN_POINT('Ctrl Pts',(21.8695411967747,-0.447286887835617,
4.39108848569571));
#36714=CARTESIAN_POINT('Ctrl Pts',(21.8615885574308,-0.38217055151792,4.46556187083511));
#36715=CARTESIAN_POINT('Ctrl Pts',(21.853635918087,-0.298050767095013,4.52341945536736));
#36716=CARTESIAN_POINT('Ctrl Pts',(21.8456832787432,-0.205212323901057,
4.55758736157894));
#36717=CARTESIAN_POINT('Ctrl Pts',(21.840070656248,-0.139691040693493,4.58170156451555));
#36718=CARTESIAN_POINT('Ctrl Pts',(21.8344580337528,-0.0698270680627233,
4.59401614113532));
#36719=CARTESIAN_POINT('Ctrl Pts',(21.8288454112575,1.47252919898561E-5,
4.59408074293421));
#36720=CARTESIAN_POINT('Ctrl Pts',(21.7211545887425,-1.54601956517634E-5,
4.59410286710644));
#36721=CARTESIAN_POINT('Ctrl Pts',(21.7229140916097,-0.0219078436841643,
4.59412557209431));
#36722=CARTESIAN_POINT('Ctrl Pts',(21.724673594477,-0.0437977792686499,
4.59293892497318));
#36723=CARTESIAN_POINT('Ctrl Pts',(21.7264330973443,-0.0655513867134097,
4.59052415646896));
#36724=CARTESIAN_POINT('Ctrl Pts',(21.7343857366881,-0.163873814968881,
4.57960983324176));
#36725=CARTESIAN_POINT('Ctrl Pts',(21.742338376032,-0.259411224460086,4.54360647774573));
#36726=CARTESIAN_POINT('Ctrl Pts',(21.7502910153758,-0.340482865683332,
4.48691599054611));
#36727=CARTESIAN_POINT('Ctrl Pts',(21.7582436547196,-0.421554506906578,
4.4302255033465));
#36728=CARTESIAN_POINT('Ctrl Pts',(21.7661962940634,-0.488160379861865,
4.3528478844433));
#36729=CARTESIAN_POINT('Ctrl Pts',(21.7741489334072,-0.532157009426634,
4.26424360160945));
#36730=CARTESIAN_POINT('Ctrl Pts',(21.782101572751,-0.576153638991403,4.1756393187756));
#36731=CARTESIAN_POINT('Ctrl Pts',(21.7900542120948,-0.597541025165654,
4.0758083720111));
#36732=CARTESIAN_POINT('Ctrl Pts',(21.7980068514386,-0.593704268699233,
3.9769564542281));
#36733=CARTESIAN_POINT('Ctrl Pts',(21.8059594907824,-0.589867512232813,
3.87810453644509));
#36734=CARTESIAN_POINT('Ctrl Pts',(21.8139121301262,-0.560806613125721,
3.78023164764359));
#36735=CARTESIAN_POINT('Ctrl Pts',(21.82186476947,-0.510074662095298,3.69530408148155));
#36736=CARTESIAN_POINT('Ctrl Pts',(21.8298174088138,-0.459342711064876,
3.61037651531951));
#36737=CARTESIAN_POINT('Ctrl Pts',(21.8377700481576,-0.386939708111122,
3.53839427179695));
#36738=CARTESIAN_POINT('Ctrl Pts',(21.8457226875014,-0.301717906454235,
3.48815816056295));
#36739=CARTESIAN_POINT('Ctrl Pts',(21.8536753268452,-0.216496104797349,
3.43792204932895));
#36740=CARTESIAN_POINT('Ctrl Pts',(21.8616279661891,-0.118455504437329,
3.40943207038352));
#36741=CARTESIAN_POINT('Ctrl Pts',(21.8695806055329,-0.0195829040543552,
3.40617151167847));
#36742=CARTESIAN_POINT('Ctrl Pts',(21.8775332448767,0.0792896963286298,
3.40291095297342));
#36743=CARTESIAN_POINT('Ctrl Pts',(21.8854858842205,0.178994296734569,3.42487981450875));
#36744=CARTESIAN_POINT('Ctrl Pts',(21.8934385235643,0.267340651814441,3.46939210375187));
#36745=CARTESIAN_POINT('Ctrl Pts',(21.9013911629081,0.355687006894294,3.51390439299499));
#36746=CARTESIAN_POINT('Ctrl Pts',(21.9093438022519,0.432675116648084,3.58096010994589));
#36747=CARTESIAN_POINT('Ctrl Pts',(21.9172964415957,0.488892136101412,3.66236077992681));
#36748=CARTESIAN_POINT('Ctrl Pts',(21.9252490809395,0.545109155554752,3.74376144990775));
#36749=CARTESIAN_POINT('Ctrl Pts',(21.9332017202833,0.580555084707621,3.8395070729187));
#36750=CARTESIAN_POINT('Ctrl Pts',(21.9411543596271,0.590896175957217,3.93789144251738));
#36751=CARTESIAN_POINT('Ctrl Pts',(21.9491069989709,0.601237267206812,4.03627581211605));
#36752=CARTESIAN_POINT('Ctrl Pts',(21.9570596383147,0.58647352055314,4.13729892830245));
#36753=CARTESIAN_POINT('Ctrl Pts',(21.9650122776585,0.548410005102802,4.22860933921557));
#36754=CARTESIAN_POINT('Ctrl Pts',(21.9729649170023,0.510346489652465,4.31991975012869));
#36755=CARTESIAN_POINT('Ctrl Pts',(21.9809175563462,0.448983205405461,4.40151745576853));
#36756=CARTESIAN_POINT('Ctrl Pts',(21.98887019569,0.371822649612145,4.46342602528218));
#36757=CARTESIAN_POINT('Ctrl Pts',(21.9968228350338,0.29466209381883,4.52533459479583));
#36758=CARTESIAN_POINT('Ctrl Pts',(22.0047754743776,0.201704266479203,4.5675540281833));
#36759=CARTESIAN_POINT('Ctrl Pts',(22.0127281137214,0.104314528045707,4.58492242469582));
#36760=CARTESIAN_POINT('Ctrl Pts',(22.0155369387284,0.069917050565085,4.59105683924014));
#36761=CARTESIAN_POINT('Ctrl Pts',(22.0183457637354,0.0349667096964542,
4.59409118517947));
#36762=CARTESIAN_POINT('Ctrl Pts',(22.0211545887425,1.20066176157995E-5,
4.59406577061205));
#36763=CARTESIAN_POINT('Origin',(4.,0.,4.));
#36764=CARTESIAN_POINT('',(22.4288454112575,5.18920962550018E-6,4.59405135764298));
#36765=CARTESIAN_POINT('',(22.3211545887424,-7.30827440488969E-6,4.59414400810326));
#36766=CARTESIAN_POINT('',(4.,-7.27562663373442E-17,4.5941));
#36767=CARTESIAN_POINT('Ctrl Pts',(22.4288454112575,5.18920962550018E-6,
4.59405135764298));
#36768=CARTESIAN_POINT('Ctrl Pts',(22.4253213780041,0.0438634191921666,
4.5940647188338));
#36769=CARTESIAN_POINT('Ctrl Pts',(22.4217973447507,0.0877187745911938,
4.589273164082));
#36770=CARTESIAN_POINT('Ctrl Pts',(22.4182733114973,0.130485535360993,4.57964583089408));
#36771=CARTESIAN_POINT('Ctrl Pts',(22.4103206721535,0.226996720088313,4.55791995512033));
#36772=CARTESIAN_POINT('Ctrl Pts',(22.4023680328097,0.317964089339764,4.51156722320365));
#36773=CARTESIAN_POINT('Ctrl Pts',(22.3944153934659,0.392265646131591,4.44625488916104));
#36774=CARTESIAN_POINT('Ctrl Pts',(22.3864627541221,0.4665672029234,4.38094255511845));
#36775=CARTESIAN_POINT('Ctrl Pts',(22.3785101147783,0.524202947255594,4.29667061894994));
#36776=CARTESIAN_POINT('Ctrl Pts',(22.3705574754345,0.558126122886914,4.20374247196213));
#36777=CARTESIAN_POINT('Ctrl Pts',(22.3626048360906,0.592049298518242,4.11081432497429));
#36778=CARTESIAN_POINT('Ctrl Pts',(22.3546521967468,0.602259905448686,4.00922996716717));
#36779=CARTESIAN_POINT('Ctrl Pts',(22.346699557403,0.587509558716917,3.91140947017845));
#36780=CARTESIAN_POINT('Ctrl Pts',(22.3387469180592,0.572759211985149,3.81358897318973));
#36781=CARTESIAN_POINT('Ctrl Pts',(22.3307942787154,0.533047911591167,3.71953233701942));
#36782=CARTESIAN_POINT('Ctrl Pts',(22.3228416393716,0.473230904440663,3.6407392662825));
#36783=CARTESIAN_POINT('Ctrl Pts',(22.3148890000278,0.413413897290173,3.5619461955456));
#36784=CARTESIAN_POINT('Ctrl Pts',(22.306936360684,0.333491183383171,3.49841669024209));
#36785=CARTESIAN_POINT('Ctrl Pts',(22.2989837213402,0.243234403245124,3.45791809774646));
#36786=CARTESIAN_POINT('Ctrl Pts',(22.2910310819964,0.152977623107077,3.41741950525082));
#36787=CARTESIAN_POINT('Ctrl Pts',(22.2830784426526,0.0523867767379842,
3.39995182556307));
#36788=CARTESIAN_POINT('Ctrl Pts',(22.2751258033088,-0.0462395349927855,
3.40765072037886));
#36789=CARTESIAN_POINT('Ctrl Pts',(22.267173163965,-0.144865846723578,3.41534961519466));
#36790=CARTESIAN_POINT('Ctrl Pts',(22.2592205246212,-0.241527623816046,
3.448215084514));
#36791=CARTESIAN_POINT('Ctrl Pts',(22.2512678852774,-0.324406647450603,
3.50222887712101));
#36792=CARTESIAN_POINT('Ctrl Pts',(22.2433152459336,-0.40728567108515,3.55624266972802));
#36793=CARTESIAN_POINT('Ctrl Pts',(22.2353626065897,-0.476381941261788,
3.63140478562268));
#36794=CARTESIAN_POINT('Ctrl Pts',(22.2274099672459,-0.523247497912515,
3.71852563243507));
#36795=CARTESIAN_POINT('Ctrl Pts',(22.2194573279021,-0.570113054563243,
3.80564647924745));
#36796=CARTESIAN_POINT('Ctrl Pts',(22.2115046885583,-0.59474789768806,3.90472605697756));
#36797=CARTESIAN_POINT('Ctrl Pts',(22.2035520492145,-0.594140082177443,
4.00365053781872));
#36798=CARTESIAN_POINT('Ctrl Pts',(22.1955994098707,-0.593532266666827,
4.10257501865988));
#36799=CARTESIAN_POINT('Ctrl Pts',(22.1876467705269,-0.567681792520777,
4.2013444026121));
#36800=CARTESIAN_POINT('Ctrl Pts',(22.1796941311831,-0.519749232289404,
4.2878827872712));
#36801=CARTESIAN_POINT('Ctrl Pts',(22.1717414918393,-0.471816672058032,
4.37442117193029));
#36802=CARTESIAN_POINT('Ctrl Pts',(22.1637888524955,-0.401802025741336,
4.44872855729627));
#36803=CARTESIAN_POINT('Ctrl Pts',(22.1558362131517,-0.318265537426909,
4.50171985346399));
#36804=CARTESIAN_POINT('Ctrl Pts',(22.1478835738079,-0.234729049112483,
4.55471114963171));
#36805=CARTESIAN_POINT('Ctrl Pts',(22.1399309344641,-0.137670718800326,
4.58638635660118));
#36806=CARTESIAN_POINT('Ctrl Pts',(22.1319782951203,-0.0389572492816432,
4.5928727489116));
#36807=CARTESIAN_POINT('Ctrl Pts',(22.1309340004994,-0.0259947671705595,
4.5937245044491));
#36808=CARTESIAN_POINT('Ctrl Pts',(22.1298897058784,-0.0130037447923657,
4.5941419185755));
#36809=CARTESIAN_POINT('Ctrl Pts',(22.1288454112575,-1.19684274697274E-5,
4.59413016891312));
#36810=CARTESIAN_POINT('Ctrl Pts',(22.0211545887425,1.20066176157995E-5,
4.59406577061205));
#36811=CARTESIAN_POINT('Ctrl Pts',(22.0262984030792,-0.064000704172389,
4.59401922879619));
#36812=CARTESIAN_POINT('Ctrl Pts',(22.031442217416,-0.128028044405449,4.5837112392356));
#36813=CARTESIAN_POINT('Ctrl Pts',(22.0365860317528,-0.188701337098646,
4.56338935830438));
#36814=CARTESIAN_POINT('Ctrl Pts',(22.0445386710966,-0.282505814282095,
4.53197053576284));
#36815=CARTESIAN_POINT('Ctrl Pts',(22.0524913104404,-0.368293119121642,
4.4766155310422));
#36816=CARTESIAN_POINT('Ctrl Pts',(22.0604439497842,-0.435574585201076,
4.40409224738955));
#36817=CARTESIAN_POINT('Ctrl Pts',(22.068396589128,-0.502856051280518,4.33156896373689));
#36818=CARTESIAN_POINT('Ctrl Pts',(22.0763492284718,-0.551631678599843,
4.24187740115222));
#36819=CARTESIAN_POINT('Ctrl Pts',(22.0843018678156,-0.575937982408454,
4.14598357473613));
#36820=CARTESIAN_POINT('Ctrl Pts',(22.0922545071594,-0.600244286217068,
4.05008974832002));
#36821=CARTESIAN_POINT('Ctrl Pts',(22.1002071465032,-0.600081266514962,
3.94799365807249));
#36822=CARTESIAN_POINT('Ctrl Pts',(22.1081597858471,-0.575468854681199,
3.85217794154701));
#36823=CARTESIAN_POINT('Ctrl Pts',(22.1161124251909,-0.550856442847438,
3.75636222502155));
#36824=CARTESIAN_POINT('Ctrl Pts',(22.1240650645347,-0.501794638882025,
3.66682688221814));
#36825=CARTESIAN_POINT('Ctrl Pts',(22.1320177038785,-0.434281916527717,
3.5945188282416));
#36826=CARTESIAN_POINT('Ctrl Pts',(22.1399703432223,-0.366769194173409,
3.52221077426505));
#36827=CARTESIAN_POINT('Ctrl Pts',(22.1479229825661,-0.280805553430205,
3.46713000911538));
#36828=CARTESIAN_POINT('Ctrl Pts',(22.1558756219099,-0.186901220180937,
3.43601090651668));
#36829=CARTESIAN_POINT('Ctrl Pts',(22.1638282612537,-0.0929968869316588,
3.40489180391798));
#36830=CARTESIAN_POINT('Ctrl Pts',(22.1717809005975,0.00884813882368474,
3.39773436387026));
#36831=CARTESIAN_POINT('Ctrl Pts',(22.1797335399413,0.106181915586414,3.41541368090248));
#36832=CARTESIAN_POINT('Ctrl Pts',(22.1876861792851,0.203515692349121,3.4330929979347));
#36833=CARTESIAN_POINT('Ctrl Pts',(22.1956388186289,0.296338220119215,3.47560907204686));
#36834=CARTESIAN_POINT('Ctrl Pts',(22.2035914579727,0.373300680656879,3.53776373412001));
#36835=CARTESIAN_POINT('Ctrl Pts',(22.2115440973165,0.450263141194552,3.59991839619317));
#36836=CARTESIAN_POINT('Ctrl Pts',(22.2194967366603,0.511365534499791,3.68171164622733));
#36837=CARTESIAN_POINT('Ctrl Pts',(22.2274493760041,0.549137260797828,3.7731431454068));
#36838=CARTESIAN_POINT('Ctrl Pts',(22.2354020153479,0.586908987095865,3.86457464458628));
#36839=CARTESIAN_POINT('Ctrl Pts',(22.2433546546918,0.6013500463867,3.96564439291107));
#36840=CARTESIAN_POINT('Ctrl Pts',(22.2513072940356,0.590694822479903,4.06399523710107));
#36841=CARTESIAN_POINT('Ctrl Pts',(22.2592599333794,0.580039598573106,4.16234608129106));
#36842=CARTESIAN_POINT('Ctrl Pts',(22.2672125727232,0.544288091468676,4.25797802134625));
#36843=CARTESIAN_POINT('Ctrl Pts',(22.275165212067,0.487811409852587,4.33919875012361));
#36844=CARTESIAN_POINT('Ctrl Pts',(22.2831178514108,0.431334728236497,4.42041947890096));
#36845=CARTESIAN_POINT('Ctrl Pts',(22.2910704907546,0.354132872108749,4.48722899640046));
#36846=CARTESIAN_POINT('Ctrl Pts',(22.2990231300984,0.265644819817582,4.53145892916239));
#36847=CARTESIAN_POINT('Ctrl Pts',(22.3064002829798,0.183560135512932,4.57248819778762));
#36848=CARTESIAN_POINT('Ctrl Pts',(22.3137774358611,0.0917635873240076,
4.59408754951618));
#36849=CARTESIAN_POINT('Ctrl Pts',(22.3211545887424,-7.30827440488969E-6,
4.59414400810326));
#36850=CARTESIAN_POINT('Origin',(4.,0.,4.));
#36851=CARTESIAN_POINT('',(22.7288454112575,-7.11440487624268E-7,4.59414971000239));
#36852=CARTESIAN_POINT('',(22.6211545887425,-1.51245797256638E-7,4.59404869726453));
#36853=CARTESIAN_POINT('',(4.,-7.27562663373442E-17,4.5941));
#36854=CARTESIAN_POINT('Ctrl Pts',(22.7288454112575,-7.11440487624268E-7,
4.59414971000239));
#36855=CARTESIAN_POINT('Ctrl Pts',(22.7287056894736,0.0017373052546791,
4.59414999869406));
#36856=CARTESIAN_POINT('Ctrl Pts',(22.7285659676897,0.0034753215591825,
4.59414251282321));
#36857=CARTESIAN_POINT('Ctrl Pts',(22.7284262459057,0.00521327185949689,
4.59412723628209));
#36858=CARTESIAN_POINT('Ctrl Pts',(22.7204736065619,0.104133365400505,4.59325773105135));
#36859=CARTESIAN_POINT('Ctrl Pts',(22.7125209672181,0.202839630323109,4.56714939948764));
#36860=CARTESIAN_POINT('Ctrl Pts',(22.7045683278743,0.289252680684759,4.51898953373575));
#36861=CARTESIAN_POINT('Ctrl Pts',(22.6966156885305,0.375665731046408,4.47082966798385));
#36862=CARTESIAN_POINT('Ctrl Pts',(22.6886630491867,0.449785566847107,4.40061826804377));
#36863=CARTESIAN_POINT('Ctrl Pts',(22.6807104098429,0.502555912967013,4.31694216252228));
#36864=CARTESIAN_POINT('Ctrl Pts',(22.6727577704991,0.555326259086918,4.23326605700079));
#36865=CARTESIAN_POINT('Ctrl Pts',(22.6648051311553,0.586747115526033,4.13612524589788));
#36866=CARTESIAN_POINT('Ctrl Pts',(22.6568524918115,0.592973744123511,4.03739517928057));
#36867=CARTESIAN_POINT('Ctrl Pts',(22.6488998524677,0.59920037272099,3.93866511266326));
#36868=CARTESIAN_POINT('Ctrl Pts',(22.6409472131239,0.580232773476834,3.83834579053153));
#36869=CARTESIAN_POINT('Ctrl Pts',(22.6329945737801,0.538391640361539,3.74870332422701));
#36870=CARTESIAN_POINT('Ctrl Pts',(22.6250419344363,0.496550507246239,3.65906085792248));
#36871=CARTESIAN_POINT('Ctrl Pts',(22.6170892950925,0.431835840259791,3.58009524744515));
#36872=CARTESIAN_POINT('Ctrl Pts',(22.6091366557487,0.35215901686313,3.52146073929621));
#36873=CARTESIAN_POINT('Ctrl Pts',(22.6011840164048,0.272482193466486,3.46282623114728));
#36874=CARTESIAN_POINT('Ctrl Pts',(22.593231377061,0.17784321365963,3.42452282532672));
#36875=CARTESIAN_POINT('Ctrl Pts',(22.5852787377172,0.0798134434713266,
3.41123383340666));
#36876=CARTESIAN_POINT('Ctrl Pts',(22.5773260983734,-0.0182163267169884,
3.3979448414866));
#36877=CARTESIAN_POINT('Ctrl Pts',(22.5693734590296,-0.119636887286728,
3.40967026346704));
#36878=CARTESIAN_POINT('Ctrl Pts',(22.5614208196858,-0.212048437952692,
3.44497640167274));
#36879=CARTESIAN_POINT('Ctrl Pts',(22.553468180342,-0.304459988618666,3.48028253987845));
#36880=CARTESIAN_POINT('Ctrl Pts',(22.5455155409982,-0.387862529380837,
3.53916939430943));
#36881=CARTESIAN_POINT('Ctrl Pts',(22.5375629016544,-0.452058834188948,
3.61443730067171));
#36882=CARTESIAN_POINT('Ctrl Pts',(22.5296102623106,-0.516255138997059,
3.689705207034));
#36883=CARTESIAN_POINT('Ctrl Pts',(22.5216576229668,-0.561245207851117,
3.7813541653276));
#36884=CARTESIAN_POINT('Ctrl Pts',(22.513704983623,-0.581528460676763,3.87817881267738));
#36885=CARTESIAN_POINT('Ctrl Pts',(22.5057523442792,-0.601811713502406,
3.97500346002715));
#36886=CARTESIAN_POINT('Ctrl Pts',(22.4977997049354,-0.597388150299644,
4.07700379643311));
#36887=CARTESIAN_POINT('Ctrl Pts',(22.4898470655916,-0.568798575589296,
4.17170890717095));
#36888=CARTESIAN_POINT('Ctrl Pts',(22.4818944262477,-0.540209000878948,
4.26641401790879));
#36889=CARTESIAN_POINT('Ctrl Pts',(22.4739417869039,-0.487453414661012,
4.35382390297851));
#36890=CARTESIAN_POINT('Ctrl Pts',(22.4659891475601,-0.416981925106977,
4.42325150516024));
#36891=CARTESIAN_POINT('Ctrl Pts',(22.4580365082163,-0.346510435552941,
4.49267910734197));
#36892=CARTESIAN_POINT('Ctrl Pts',(22.4500838688725,-0.258323042662803,
4.54412442663572));
#36893=CARTESIAN_POINT('Ctrl Pts',(22.4421312295287,-0.163201846116148,
4.57129757646718));
#36894=CARTESIAN_POINT('Ctrl Pts',(22.4377026234383,-0.11023146834083,4.58642955613285));
#36895=CARTESIAN_POINT('Ctrl Pts',(22.4332740173479,-0.0551108697057404,
4.59403456681078));
#36896=CARTESIAN_POINT('Ctrl Pts',(22.4288454112575,5.18920962550018E-6,
4.59405135764298));
#36897=CARTESIAN_POINT('Ctrl Pts',(22.3211545887424,-7.30827440488969E-6,
4.59414400810326));
#36898=CARTESIAN_POINT('Ctrl Pts',(22.3217300752049,-0.00716629073194701,
4.59414841239758));
#36899=CARTESIAN_POINT('Ctrl Pts',(22.3223055616673,-0.0143251170819474,
4.59402171850555));
#36900=CARTESIAN_POINT('Ctrl Pts',(22.3228810481298,-0.0214791647150919,
4.59376292335171));
#36901=CARTESIAN_POINT('Ctrl Pts',(22.3308336874736,-0.120340848501978,
4.59018663675477));
#36902=CARTESIAN_POINT('Ctrl Pts',(22.3387863268174,-0.218289967621164,
4.56138371553656));
#36903=CARTESIAN_POINT('Ctrl Pts',(22.3467389661612,-0.303350908332583,
4.51087570903952));
#36904=CARTESIAN_POINT('Ctrl Pts',(22.3546916055051,-0.388411849044011,
4.46036770254246));
#36905=CARTESIAN_POINT('Ctrl Pts',(22.3626442448489,-0.460584611347669,
4.38815461076656));
#36906=CARTESIAN_POINT('Ctrl Pts',(22.3705968841927,-0.511045091866278,
4.3030654678256));
#36907=CARTESIAN_POINT('Ctrl Pts',(22.3785495235365,-0.561505572384874,
4.21797632488466));
#36908=CARTESIAN_POINT('Ctrl Pts',(22.3865021628803,-0.590253771118432,
4.12001113077866));
#36909=CARTESIAN_POINT('Ctrl Pts',(22.3944548022241,-0.593774829630164,
4.02114746451658));
#36910=CARTESIAN_POINT('Ctrl Pts',(22.4024074415679,-0.597295888141896,
3.92228379825449));
#36911=CARTESIAN_POINT('Ctrl Pts',(22.4103600809117,-0.575589806431797,
3.82252165983632));
#36912=CARTESIAN_POINT('Ctrl Pts',(22.4183127202555,-0.531310447862662,
3.73405832985033));
#36913=CARTESIAN_POINT('Ctrl Pts',(22.4262653595993,-0.487031089293526,
3.64559499986435));
#36914=CARTESIAN_POINT('Ctrl Pts',(22.4342179989431,-0.420178453865353,
3.56843047831055));
#36915=CARTESIAN_POINT('Ctrl Pts',(22.4421706382869,-0.338926188203527,
3.51199917808983));
#36916=CARTESIAN_POINT('Ctrl Pts',(22.4501232776307,-0.257673922541701,
3.45556787786912));
#36917=CARTESIAN_POINT('Ctrl Pts',(22.4580759169745,-0.162022026646223,
3.41986979898149));
#36918=CARTESIAN_POINT('Ctrl Pts',(22.4660285563183,-0.0636652448434586,
3.40926951931498));
#36919=CARTESIAN_POINT('Ctrl Pts',(22.4739811956621,0.0346915369593057,
3.39866923964846));
#36920=CARTESIAN_POINT('Ctrl Pts',(22.4819338350059,0.135753204669356,3.41316675920307));
#36921=CARTESIAN_POINT('Ctrl Pts',(22.4898864743497,0.227163587879617,3.45098955584192));
#36922=CARTESIAN_POINT('Ctrl Pts',(22.4978391136936,0.318573971089878,3.48881235248077));
#36923=CARTESIAN_POINT('Ctrl Pts',(22.5057917530374,0.40033306980035,3.54996042620388));
#36924=CARTESIAN_POINT('Ctrl Pts',(22.5137443923812,0.462444730281743,3.62695759769032));
#36925=CARTESIAN_POINT('Ctrl Pts',(22.521697031725,0.524556390763143,3.70395476917678));
#36926=CARTESIAN_POINT('Ctrl Pts',(22.5296496710688,0.567020613015458,3.79680103842659));
#36927=CARTESIAN_POINT('Ctrl Pts',(22.5376023104126,0.584645549343987,3.89414467407578));
#36928=CARTESIAN_POINT('Ctrl Pts',(22.5455549497564,0.602270485672515,3.99148830972497));
#36929=CARTESIAN_POINT('Ctrl Pts',(22.5535075891002,0.595056136077256,4.09332931177355));
#36930=CARTESIAN_POINT('Ctrl Pts',(22.561460228444,0.563884587368514,4.18721625032571));
#36931=CARTESIAN_POINT('Ctrl Pts',(22.5694128677878,0.532713038659782,4.28110318887784));
#36932=CARTESIAN_POINT('Ctrl Pts',(22.5773655071316,0.477584290837583,4.36703606393356));
#36933=CARTESIAN_POINT('Ctrl Pts',(22.5853181464754,0.405238519368296,4.43450837402952));
#36934=CARTESIAN_POINT('Ctrl Pts',(22.5932707858192,0.332892747898984,4.5019806841255));
#36935=CARTESIAN_POINT('Ctrl Pts',(22.601223425163,0.24332995278257,4.55099242926169));
#36936=CARTESIAN_POINT('Ctrl Pts',(22.6091760645068,0.14750052788588,4.57555132613148));
#36937=CARTESIAN_POINT('Ctrl Pts',(22.6131689059187,0.0993867282199646,
4.58788179608141));
#36938=CARTESIAN_POINT('Ctrl Pts',(22.6171617473306,0.0496932250345643,
4.5940481472271));
#36939=CARTESIAN_POINT('Ctrl Pts',(22.6211545887425,-1.51173456864708E-7,
4.59404872180247));
#36940=CARTESIAN_POINT('Origin',(3.42660065607856,0.,4.));
#36941=CARTESIAN_POINT('',(22.7766006560786,-4.98014040841517E-7,4.41590979742004));
#36942=CARTESIAN_POINT('',(22.8,4.87367679877478E-13,4.415875));
#36943=CARTESIAN_POINT('',(3.42660065607856,4.87367679877478E-13,4.415875));
#36944=CARTESIAN_POINT('',(22.8,-0.195748955928421,4.36692555359082));
#36945=CARTESIAN_POINT('Ctrl Pts',(22.7766006560786,-4.98014040834069E-7,
4.41590979742004));
#36946=CARTESIAN_POINT('Ctrl Pts',(22.7844004373857,-0.0679170312443507,
4.41589851620688));
#36947=CARTESIAN_POINT('Ctrl Pts',(22.7922002186928,-0.135834416676695,
4.39892762624317));
#36948=CARTESIAN_POINT('Ctrl Pts',(22.8,-0.195762566582618,4.36695865185838));
#36949=CARTESIAN_POINT('Origin',(22.8,0.,4.));
#36950=CARTESIAN_POINT('Origin',(3.42660065607856,0.,4.));
#36951=CARTESIAN_POINT('',(22.4766006560785,3.63249072247605E-6,4.41584094994071));
#36952=CARTESIAN_POINT('',(22.5733993439214,-1.05822049303872E-7,4.41583910483016));
#36953=CARTESIAN_POINT('',(3.42660065607856,4.87367679877478E-13,4.415875));
#36954=CARTESIAN_POINT('Ctrl Pts',(22.4766006560785,3.63249072248342E-6,
4.41584094994071));
#36955=CARTESIAN_POINT('Ctrl Pts',(22.4810292621689,-0.0385780726118879,
4.41582919621688));
#36956=CARTESIAN_POINT('Ctrl Pts',(22.4934105076031,-0.146451497349971,
4.40094585736882));
#36957=CARTESIAN_POINT('Ctrl Pts',(22.5137443923812,-0.304292138366774,
4.30886736509782));
#36958=CARTESIAN_POINT('Ctrl Pts',(22.5376023104126,-0.415080201412036,
4.12530439950267));
#36959=CARTESIAN_POINT('Ctrl Pts',(22.561460228444,-0.424369795825249,3.91110111771763));
#36960=CARTESIAN_POINT('Ctrl Pts',(22.5853181464754,-0.329889515310188,
3.71863599132299));
#36961=CARTESIAN_POINT('Ctrl Pts',(22.6091760645068,-0.154742073939436,
3.59497211022641));
#36962=CARTESIAN_POINT('Ctrl Pts',(22.6330339825383,0.0582436639512456,
3.57034842802071));
#36963=CARTESIAN_POINT('Ctrl Pts',(22.6568919005697,0.256987911016647,3.65078654733876));
#36964=CARTESIAN_POINT('Ctrl Pts',(22.6807498186011,0.39289034562191,3.81661632308649));
#36965=CARTESIAN_POINT('Ctrl Pts',(22.7046077366325,0.432722782933869,4.02728943245291));
#36966=CARTESIAN_POINT('Ctrl Pts',(22.7284656546639,0.366738191089385,4.2312875884069));
#36967=CARTESIAN_POINT('Ctrl Pts',(22.7523235726953,0.211084664509997,4.37873330099785));
#36968=CARTESIAN_POINT('Ctrl Pts',(22.7683685731669,0.0716802821347026,
4.41560650088387));
#36969=CARTESIAN_POINT('Ctrl Pts',(22.7764609342946,0.00121612829983627,
4.41590999950663));
#36970=CARTESIAN_POINT('Ctrl Pts',(22.7766006560786,-4.98014040834069E-7,
4.41590979742004));
#36971=CARTESIAN_POINT('',(22.8,0.415641328671541,4.01393920819689));
#36972=CARTESIAN_POINT('Origin',(22.8,0.,4.));
#36973=CARTESIAN_POINT('Ctrl Pts',(22.5733993439214,-1.0582204931428E-7,
4.41583910483016));
#36974=CARTESIAN_POINT('Ctrl Pts',(22.5773591418533,-0.034498011376554,
4.41583950370926));
#36975=CARTESIAN_POINT('Ctrl Pts',(22.5892715791291,-0.138279341065089,
4.40307041914735));
#36976=CARTESIAN_POINT('Ctrl Pts',(22.6091366557487,-0.295063722636797,
4.31769517074077));
#36977=CARTESIAN_POINT('Ctrl Pts',(22.6329945737801,-0.411209141905604,
4.13747522778479));
#36978=CARTESIAN_POINT('Ctrl Pts',(22.6568524918115,-0.426804986482714,
3.92363755172126));
#36979=CARTESIAN_POINT('Ctrl Pts',(22.6807104098429,-0.33803111495158,3.72847502015617));
#36980=CARTESIAN_POINT('Ctrl Pts',(22.7045683278743,-0.16660749730952,3.59970312177549));
#36981=CARTESIAN_POINT('Ctrl Pts',(22.7284262459057,0.0455714674079685,
3.56882345794434));
#36982=CARTESIAN_POINT('Ctrl Pts',(22.7522841639372,0.246577802732478,3.64336153500176));
#36983=CARTESIAN_POINT('Ctrl Pts',(22.7761420819686,0.387346815298129,3.80514019809748));
#36984=CARTESIAN_POINT('Ctrl Pts',(22.7920473606562,0.417963038852713,3.94471011778788));
#36985=CARTESIAN_POINT('Ctrl Pts',(22.8,0.415641328671541,4.01393920819689));
#36986=CARTESIAN_POINT('Origin',(3.42660065607856,0.,4.));
#36987=CARTESIAN_POINT('',(22.1766006560786,-8.37799962078257E-6,4.41589611849309));
#36988=CARTESIAN_POINT('',(22.2733993439214,-5.11585294796223E-6,4.41590580604266));
#36989=CARTESIAN_POINT('',(3.42660065607856,4.87367679877478E-13,4.415875));
#36990=CARTESIAN_POINT('Ctrl Pts',(22.1766006560786,-8.37799962077716E-6,
4.41589611849309));
#36991=CARTESIAN_POINT('Ctrl Pts',(22.1776449506995,-0.0091027307950905,
4.41590434335565));
#36992=CARTESIAN_POINT('Ctrl Pts',(22.1866418846642,-0.0874489573854402,
4.4133870032437));
#36993=CARTESIAN_POINT('Ctrl Pts',(22.2035914579727,-0.232253957950086,
4.36612956178204));
#36994=CARTESIAN_POINT('Ctrl Pts',(22.2274493760041,-0.379286482964224,
4.21008217638027));
#36995=CARTESIAN_POINT('Ctrl Pts',(22.2513072940356,-0.433573131350875,
4.00266397632408));
#36996=CARTESIAN_POINT('Ctrl Pts',(22.275165212067,-0.381839338801546,3.79459436150246));
#36997=CARTESIAN_POINT('Ctrl Pts',(22.2990231300984,-0.236735426869051,
3.63675202040985));
#36998=CARTESIAN_POINT('Ctrl Pts',(22.3228810481298,-0.0337432544318164,
3.56773370504276));
#36999=CARTESIAN_POINT('Ctrl Pts',(22.3467389661613,0.177500062688638,3.60441627341574));
#37000=CARTESIAN_POINT('Ctrl Pts',(22.3705968841926,0.345339779804043,3.73782983856348));
#37001=CARTESIAN_POINT('Ctrl Pts',(22.3944548022241,0.428734513273282,3.93535114928888));
#37002=CARTESIAN_POINT('Ctrl Pts',(22.4183127202555,0.407291980919218,4.1486808655136));
#37003=CARTESIAN_POINT('Ctrl Pts',(22.4421706382869,0.286255462618544,4.32565405918856));
#37004=CARTESIAN_POINT('Ctrl Pts',(22.4615999502279,0.130682174689606,4.40492695636159));
#37005=CARTESIAN_POINT('Ctrl Pts',(22.4730766228251,0.0307047625933256,
4.41585030288671));
#37006=CARTESIAN_POINT('Ctrl Pts',(22.4766006560785,3.63249072248342E-6,
4.41584094994071));
#37007=CARTESIAN_POINT('Ctrl Pts',(22.2733993439214,-5.11585294797612E-6,
4.41590580604266));
#37008=CARTESIAN_POINT('Ctrl Pts',(22.2739748303838,-0.0050164638240448,
4.41590888908576));
#37009=CARTESIAN_POINT('Ctrl Pts',(22.2825029561901,-0.0792779396689182,
4.41459464077989));
#37010=CARTESIAN_POINT('Ctrl Pts',(22.2989837213402,-0.221370022215225,
4.37281103827166));
#37011=CARTESIAN_POINT('Ctrl Pts',(22.3228416393716,-0.372934645290675,
4.22116172228637));
#37012=CARTESIAN_POINT('Ctrl Pts',(22.346699557403,-0.43330658847365,4.01543234121164));
#37013=CARTESIAN_POINT('Ctrl Pts',(22.3705574754345,-0.387723268841402,
3.80592933171158));
#37014=CARTESIAN_POINT('Ctrl Pts',(22.3944153934659,-0.247331046528593,
3.64388188817752));
#37015=CARTESIAN_POINT('Ctrl Pts',(22.4182733114973,-0.0464596501027702,
3.56891502119853));
#37016=CARTESIAN_POINT('Ctrl Pts',(22.4421312295287,0.165772403721094,3.59936017830047));
#37017=CARTESIAN_POINT('Ctrl Pts',(22.4659891475602,0.337468575289321,3.7277726770023));
#37018=CARTESIAN_POINT('Ctrl Pts',(22.4898470655915,0.426644514167594,3.92275218663495));
#37019=CARTESIAN_POINT('Ctrl Pts',(22.513704983623,0.411494197867752,4.13662086224655));
#37020=CARTESIAN_POINT('Ctrl Pts',(22.5375629016544,0.295722435535401,4.31708206952049));
#37021=CARTESIAN_POINT('Ctrl Pts',(22.5574610217539,0.138855410360913,4.40292493148274));
#37022=CARTESIAN_POINT('Ctrl Pts',(22.5694065025095,0.0347856757474044,
4.41583870262252));
#37023=CARTESIAN_POINT('Ctrl Pts',(22.5733993439214,-1.0582204931428E-7,
4.41583910483016));
#37024=CARTESIAN_POINT('Origin',(3.42660065607856,0.,4.));
#37025=CARTESIAN_POINT('',(21.8766006560786,1.03078286340212E-5,4.41586151989188));
#37026=CARTESIAN_POINT('',(21.9733993439214,8.40473402259622E-6,4.41585103914036));
#37027=CARTESIAN_POINT('',(3.42660065607856,4.87367679877478E-13,4.415875));
#37028=CARTESIAN_POINT('Ctrl Pts',(21.8766006560786,1.03078286340201E-5,
4.41586151989188));
#37029=CARTESIAN_POINT('Ctrl Pts',(21.8822132785738,-0.0488795353146484,
4.415816298089));
#37030=CARTESIAN_POINT('Ctrl Pts',(21.8957785404128,-0.167079919178725,
4.39498170153279));
#37031=CARTESIAN_POINT('Ctrl Pts',(21.9172964415957,-0.326407159500644,
4.28539643168872));
#37032=CARTESIAN_POINT('Ctrl Pts',(21.9411543596271,-0.423245389017799,
4.09410684177624));
#37033=CARTESIAN_POINT('Ctrl Pts',(21.9650122776585,-0.416588591947193,
3.87980556563057));
#37034=CARTESIAN_POINT('Ctrl Pts',(21.98887019569,-0.30806453650007,3.69489510271888));
#37035=CARTESIAN_POINT('Ctrl Pts',(22.0127281137213,-0.12421031036921,3.58459109808296));
#37036=CARTESIAN_POINT('Ctrl Pts',(22.0365860317528,0.0900167200678817,
3.57586588547707));
#37037=CARTESIAN_POINT('Ctrl Pts',(22.0604439497842,0.282232210442068,3.67085301705332));
#37038=CARTESIAN_POINT('Ctrl Pts',(22.0843018678157,0.405434237512275,3.8463255517439));
#37039=CARTESIAN_POINT('Ctrl Pts',(22.108159785847,0.429496549703537,4.05937567504088));
#37040=CARTESIAN_POINT('Ctrl Pts',(22.1320177038785,0.348535256241736,4.25790682842971));
#37041=CARTESIAN_POINT('Ctrl Pts',(22.1548313272889,0.18962186617866,4.38744320371645));
#37042=CARTESIAN_POINT('Ctrl Pts',(22.1696923113557,0.0601536901409818,
4.41584170838249));
#37043=CARTESIAN_POINT('Ctrl Pts',(22.1766006560786,-8.37799962077716E-6,
4.41589611849309));
#37044=CARTESIAN_POINT('Ctrl Pts',(21.9733993439214,8.40473402260317E-6,
4.41585103914036));
#37045=CARTESIAN_POINT('Ctrl Pts',(21.9785431582582,-0.044801031555974,
4.41581845947763));
#37046=CARTESIAN_POINT('Ctrl Pts',(21.9916396119388,-0.158914563981884,
4.39744691543598));
#37047=CARTESIAN_POINT('Ctrl Pts',(22.0126887049632,-0.317860118355158,
4.29488591379237));
#37048=CARTESIAN_POINT('Ctrl Pts',(22.0365466229946,-0.420290167226249,
4.10653136780738));
#37049=CARTESIAN_POINT('Ctrl Pts',(22.060404541026,-0.419947821735935,3.89212700053744));
#37050=CARTESIAN_POINT('Ctrl Pts',(22.0842624590574,-0.316916794682727,
3.70410052003731));
#37051=CARTESIAN_POINT('Ctrl Pts',(22.1081203770888,-0.136390978688423,
3.58842952252864));
#37052=CARTESIAN_POINT('Ctrl Pts',(22.1319782951203,0.0774861468089536,
3.57339871771534));
#37053=CARTESIAN_POINT('Ctrl Pts',(22.1558362131517,0.27241579873489,3.66268354680831));
#37054=CARTESIAN_POINT('Ctrl Pts',(22.1796941311831,0.400732367405962,3.83445143701846));
#37055=CARTESIAN_POINT('Ctrl Pts',(22.2035520492145,0.431058956528623,4.04670046033727));
#37056=CARTESIAN_POINT('Ctrl Pts',(22.227409967246,0.355979888945518,4.24752994899471));
#37057=CARTESIAN_POINT('Ctrl Pts',(22.2506923988149,0.197764744804664,4.38444734931837));
#37058=CARTESIAN_POINT('Ctrl Pts',(22.26602219104,0.064235283418036,4.41586628455644));
#37059=CARTESIAN_POINT('Ctrl Pts',(22.2733993439214,-5.11585294797612E-6,
4.41590580604266));
#37060=CARTESIAN_POINT('Origin',(3.42660065607856,0.,4.));
#37061=CARTESIAN_POINT('',(21.5766006560785,-1.05752387382048E-5,4.41586434469346));
#37062=CARTESIAN_POINT('',(21.6733993439214,-1.08222664516599E-5,4.41587700699864));
#37063=CARTESIAN_POINT('',(3.42660065607856,4.87367679877478E-13,4.415875));
#37064=CARTESIAN_POINT('Ctrl Pts',(21.5766006560785,-1.05752387381843E-5,
4.41586434469346));
#37065=CARTESIAN_POINT('Ctrl Pts',(21.5788289671043,-0.0194203346498642,
4.41588296395747));
#37066=CARTESIAN_POINT('Ctrl Pts',(21.5890099174739,-0.10809016089515,4.40978779866957));
#37067=CARTESIAN_POINT('Ctrl Pts',(21.6071435071872,-0.258824259222961,
4.34785450957493));
#37068=CARTESIAN_POINT('Ctrl Pts',(21.6310014252187,-0.39385182381868,4.18131050126406));
#37069=CARTESIAN_POINT('Ctrl Pts',(21.6548593432501,-0.432571889182456,
3.97043113659525));
#37070=CARTESIAN_POINT('Ctrl Pts',(21.6787172612815,-0.365516344619441,
3.76678216446856));
#37071=CARTESIAN_POINT('Ctrl Pts',(21.702575179313,-0.209082097331647,3.62016130585559));
#37072=CARTESIAN_POINT('Ctrl Pts',(21.7264330973443,-0.00152158196427748,
3.56642135455923));
#37073=CARTESIAN_POINT('Ctrl Pts',(21.7502910153758,0.206411001640417,3.61870319251831));
#37074=CARTESIAN_POINT('Ctrl Pts',(21.7741489334072,0.363870472821225,3.76422248622317));
#37075=CARTESIAN_POINT('Ctrl Pts',(21.7980068514386,0.432353701764573,3.96739580449697));
#37076=CARTESIAN_POINT('Ctrl Pts',(21.82186476947,0.395114673548107,4.17854173669174));
#37077=CARTESIAN_POINT('Ctrl Pts',(21.8457226875014,0.261259344941517,4.3460293508861));
#37078=CARTESIAN_POINT('Ctrl Pts',(21.8639679830376,0.110037800305057,4.4094070875278));
#37079=CARTESIAN_POINT('Ctrl Pts',(21.87426063923,0.0203934810735595,4.41588037378429));
#37080=CARTESIAN_POINT('Ctrl Pts',(21.8766006560786,1.03078286340201E-5,
4.41586151989188));
#37081=CARTESIAN_POINT('Ctrl Pts',(21.6733993439214,-1.0822266451653E-5,
4.41587700699864));
#37082=CARTESIAN_POINT('Ctrl Pts',(21.6751588467887,-0.0153356749568721,
4.41589290068126));
#37083=CARTESIAN_POINT('Ctrl Pts',(21.6848709889998,-0.0999166717736498,
4.41130778913604));
#37084=CARTESIAN_POINT('Ctrl Pts',(21.7025357705547,-0.248467031045983,
4.35532645760922));
#37085=CARTESIAN_POINT('Ctrl Pts',(21.7263936885861,-0.388341045935521,
4.1928315042612));
#37086=CARTESIAN_POINT('Ctrl Pts',(21.7502516066176,-0.433255096896122,
3.98318399549658));
#37087=CARTESIAN_POINT('Ctrl Pts',(21.774109524649,-0.372226475033738,3.77764845789182));
#37088=CARTESIAN_POINT('Ctrl Pts',(21.7979674426804,-0.220178340780001,
3.62648392906691));
#37089=CARTESIAN_POINT('Ctrl Pts',(21.8218253607118,-0.0142906046679706,
3.56665425395863));
#37090=CARTESIAN_POINT('Ctrl Pts',(21.8456832787432,0.195091573553633,3.61278941785858));
#37091=CARTESIAN_POINT('Ctrl Pts',(21.8695411967747,0.356768547853618,3.75360811649661));
#37092=CARTESIAN_POINT('Ctrl Pts',(21.8933991148061,0.431205894023261,3.95467634223136));
#37093=CARTESIAN_POINT('Ctrl Pts',(21.9172570328375,0.400201653291494,4.16682743688221));
#37094=CARTESIAN_POINT('Ctrl Pts',(21.941114950869,0.271337207055788,4.33818467892719));
#37095=CARTESIAN_POINT('Ctrl Pts',(21.9598290545635,0.118211900824938,4.40773087908456));
#37096=CARTESIAN_POINT('Ctrl Pts',(21.9705905189143,0.0244769910710258,
4.41586882955141));
#37097=CARTESIAN_POINT('Ctrl Pts',(21.9733993439214,8.40473402260317E-6,
4.41585103914036));
#37098=CARTESIAN_POINT('Origin',(3.42660065607856,0.,4.));
#37099=CARTESIAN_POINT('',(21.2766006560785,8.9771325895615E-6,4.41589335210553));
#37100=CARTESIAN_POINT('',(21.3733993439214,1.06214664634743E-5,4.41588075133303));
#37101=CARTESIAN_POINT('',(3.42660065607856,4.87367679877478E-13,4.415875));
#37102=CARTESIAN_POINT('Ctrl Pts',(21.2766006560785,8.97713258955941E-6,
4.41589335210553));
#37103=CARTESIAN_POINT('Ctrl Pts',(21.2833972949786,-0.0591814269577189,
4.41583723296416));
#37104=CARTESIAN_POINT('Ctrl Pts',(21.2981465732225,-0.187680420990878,
4.38813575385326));
#37105=CARTESIAN_POINT('Ctrl Pts',(21.3208484908102,-0.346716519889314,
4.26034671465164));
#37106=CARTESIAN_POINT('Ctrl Pts',(21.3447064088417,-0.429069235164158,
4.0623886883135));
#37107=CARTESIAN_POINT('Ctrl Pts',(21.368564326873,-0.406502834830527,3.8491749282489));
#37108=CARTESIAN_POINT('Ctrl Pts',(21.3924222449045,-0.284535418465691,
3.67284200661995));
#37109=CARTESIAN_POINT('Ctrl Pts',(21.4162801629359,-0.0929913416969399,
3.5765081259772));
#37110=CARTESIAN_POINT('Ctrl Pts',(21.4401380809674,0.121291651150069,3.58372954422009));
#37111=CARTESIAN_POINT('Ctrl Pts',(21.4639959989987,0.305915531372611,3.69274042788069));
#37112=CARTESIAN_POINT('Ctrl Pts',(21.4878539170302,0.415734731202803,3.87688464650718));
#37113=CARTESIAN_POINT('Ctrl Pts',(21.5117118350615,0.423895464867194,4.09113392265755));
#37114=CARTESIAN_POINT('Ctrl Pts',(21.535569753093,0.328402210690932,4.28309847227994));
#37115=CARTESIAN_POINT('Ctrl Pts',(21.5571993600986,0.169024930905334,4.39437398220882));
#37116=CARTESIAN_POINT('Ctrl Pts',(21.5708763277605,0.0498513310028489,
4.41581651349798));
#37117=CARTESIAN_POINT('Ctrl Pts',(21.5766006560785,-1.05752387381843E-5,
4.41586434469346));
#37118=CARTESIAN_POINT('Ctrl Pts',(21.3733993439214,1.06214664634605E-5,
4.41588075133303));
#37119=CARTESIAN_POINT('Ctrl Pts',(21.379727174663,-0.0551018547626871,
4.41582358345633));
#37120=CARTESIAN_POINT('Ctrl Pts',(21.3940076447484,-0.1795281855266,4.39095386216025));
#37121=CARTESIAN_POINT('Ctrl Pts',(21.4162407541777,-0.338898428465248,
4.27044521104599));
#37122=CARTESIAN_POINT('Ctrl Pts',(21.4400986722091,-0.427045644525908,
4.07499849655415));
#37123=CARTESIAN_POINT('Ctrl Pts',(21.4639565902406,-0.410768568010174,
3.86121260673678));
#37124=CARTESIAN_POINT('Ctrl Pts',(21.4878145082719,-0.294047387504818,
3.68136401506497));
#37125=CARTESIAN_POINT('Ctrl Pts',(21.5116724263034,-0.105423611064507,
3.57943060117972));
#37126=CARTESIAN_POINT('Ctrl Pts',(21.5355303443348,0.108979109962582,3.58033786138646));
#37127=CARTESIAN_POINT('Ctrl Pts',(21.5593882623662,0.296733470072461,3.68386394585134));
#37128=CARTESIAN_POINT('Ctrl Pts',(21.5832461803976,0.411928413892185,3.86469390692879));
#37129=CARTESIAN_POINT('Ctrl Pts',(21.6071040984291,0.426395639810567,4.07860989342611));
#37130=CARTESIAN_POINT('Ctrl Pts',(21.6309620164605,0.33659751701124,4.27330361969026));
#37131=CARTESIAN_POINT('Ctrl Pts',(21.6530604316246,0.177184770587036,4.39173732935402));
#37132=CARTESIAN_POINT('Ctrl Pts',(21.6672062074449,0.0539299276789421,
4.41582106406873));
#37133=CARTESIAN_POINT('Ctrl Pts',(21.6733993439214,-1.0822266451653E-5,
4.41587700699864));
#37134=CARTESIAN_POINT('Origin',(3.42660065607856,0.,4.));
#37135=CARTESIAN_POINT('',(20.9766006560786,-4.48287659654576E-6,4.41584197426197));
#37136=CARTESIAN_POINT('',(21.0733993439214,-7.65157297119567E-6,4.41584853425778));
#37137=CARTESIAN_POINT('',(3.42660065607856,4.87367679877478E-13,4.415875));
#37138=CARTESIAN_POINT('Ctrl Pts',(20.9766006560786,-4.48287659652116E-6,
4.41584197426197));
#37139=CARTESIAN_POINT('Ctrl Pts',(20.9800129835092,-0.0297322302090305,
4.41585318364051));
#37140=CARTESIAN_POINT('Ctrl Pts',(20.9913779502836,-0.128734546054536,
4.40538471300776));
#37141=CARTESIAN_POINT('Ctrl Pts',(21.0106955564018,-0.28396276796243,4.32765515869354));
#37142=CARTESIAN_POINT('Ctrl Pts',(21.0345534744332,-0.40623841344949,4.15153583326342));
#37143=CARTESIAN_POINT('Ctrl Pts',(21.0584113924646,-0.429177699343215,
3.93836186909709));
#37144=CARTESIAN_POINT('Ctrl Pts',(21.082269310496,-0.347171348131155,3.74026010679315));
#37145=CARTESIAN_POINT('Ctrl Pts',(21.1061272285274,-0.180272145040548,
3.605671823621));
#37146=CARTESIAN_POINT('Ctrl Pts',(21.1299851465589,0.0307085077608185,
3.56750752082027));
#37147=CARTESIAN_POINT('Ctrl Pts',(21.1538430645903,0.234180094072738,3.63509941005724));
#37148=CARTESIAN_POINT('Ctrl Pts',(21.1777009826217,0.380388268371489,3.79191943321731));
#37149=CARTESIAN_POINT('Ctrl Pts',(21.2015589006531,0.433581149524578,3.99962082296209));
#37150=CARTESIAN_POINT('Ctrl Pts',(21.2254168186846,0.380751629084578,4.2074149318183));
#37151=CARTESIAN_POINT('Ctrl Pts',(21.2492747367159,0.234817963878357,4.36449043997717));
#37152=CARTESIAN_POINT('Ctrl Pts',(21.2663360158473,0.0893960873046664,
4.41308118928586));
#37153=CARTESIAN_POINT('Ctrl Pts',(21.2754446556348,0.0100763257733538,
4.41590289708112));
#37154=CARTESIAN_POINT('Ctrl Pts',(21.2766006560785,8.97713258955941E-6,
4.41589335210553));
#37155=CARTESIAN_POINT('Ctrl Pts',(21.0733993439214,-7.65157297121996E-6,
4.41584853425778));
#37156=CARTESIAN_POINT('Ctrl Pts',(21.0763428631935,-0.0256500457845501,
4.41586537097631));
#37157=CARTESIAN_POINT('Ctrl Pts',(21.0872390218095,-0.120560449820324,
4.40722571769055));
#37158=CARTESIAN_POINT('Ctrl Pts',(21.1060878197692,-0.274189543318984,
4.33587624407661));
#37159=CARTESIAN_POINT('Ctrl Pts',(21.1299457378007,-0.401599180171465,
4.16343456021562));
#37160=CARTESIAN_POINT('Ctrl Pts',(21.1538036558321,-0.430806878168669,
3.95102867450389));
#37161=CARTESIAN_POINT('Ctrl Pts',(21.1776615738635,-0.354670559489406,
3.75059761183336));
#37162=CARTESIAN_POINT('Ctrl Pts',(21.2015194918949,-0.191807627993766,
3.61115222665144));
#37163=CARTESIAN_POINT('Ctrl Pts',(21.2253774099264,0.0179574932869785,
3.56679071405539));
#37164=CARTESIAN_POINT('Ctrl Pts',(21.2492353279577,0.223331518303719,3.62836067225603));
#37165=CARTESIAN_POINT('Ctrl Pts',(21.2730932459892,0.374094903668402,3.78080656934254));
#37166=CARTESIAN_POINT('Ctrl Pts',(21.2969511640206,0.433381894944723,3.98685123093373));
#37167=CARTESIAN_POINT('Ctrl Pts',(21.320809082052,0.386695207821707,4.19611112472705));
#37168=CARTESIAN_POINT('Ctrl Pts',(21.3446670000834,0.245451009020076,4.35741650656472));
#37169=CARTESIAN_POINT('Ctrl Pts',(21.3621970873732,0.0975684711839555,
4.41172139589413));
#37170=CARTESIAN_POINT('Ctrl Pts',(21.3717745353192,0.014161952170494,4.41589543043265));
#37171=CARTESIAN_POINT('Ctrl Pts',(21.3733993439214,1.06214664634605E-5,
4.41588075133303));
#37172=CARTESIAN_POINT('Origin',(3.42660065607856,0.,4.));
#37173=CARTESIAN_POINT('',(20.6766006560786,1.29204965968245E-6,4.41591114679826));
#37174=CARTESIAN_POINT('',(20.7733993439214,3.9567662055099E-6,4.41590779860895));
#37175=CARTESIAN_POINT('',(3.42660065607856,4.87367679877478E-13,4.415875));
#37176=CARTESIAN_POINT('Ctrl Pts',(20.6766006560786,1.29076178055295E-6,
4.41591111076812));
#37177=CARTESIAN_POINT('Ctrl Pts',(20.6766286720397,-0.000242659277546582,
4.41591112051333));
#37178=CARTESIAN_POINT('Ctrl Pts',(20.6846093273446,-0.0697345275278937,
4.41585145172406));
#37179=CARTESIAN_POINT('Ctrl Pts',(20.7005426219933,-0.208420567790133,
4.38020336888205));
#37180=CARTESIAN_POINT('Ctrl Pts',(20.7244005400248,-0.365106210756856,
4.23385701605743));
#37181=CARTESIAN_POINT('Ctrl Pts',(20.7482584580562,-0.432520392530856,
4.03032528343114));
#37182=CARTESIAN_POINT('Ctrl Pts',(20.7721163760876,-0.394167874571092,
3.81937870627435));
#37183=CARTESIAN_POINT('Ctrl Pts',(20.795974294119,-0.259432524437891,3.65259868360638));
#37184=CARTESIAN_POINT('Ctrl Pts',(20.8198322121504,-0.0612578225112809,
3.57076788979259));
#37185=CARTESIAN_POINT('Ctrl Pts',(20.8436901301819,0.151895538690754,3.5938959627232));
#37186=CARTESIAN_POINT('Ctrl Pts',(20.8675480482132,0.327906592802717,3.71632757520176));
#37187=CARTESIAN_POINT('Ctrl Pts',(20.8914059662447,0.423735399567132,3.90812480123879));
#37188=CARTESIAN_POINT('Ctrl Pts',(20.9152638842761,0.415949440063929,4.12238802732943));
#37189=CARTESIAN_POINT('Ctrl Pts',(20.9391218023075,0.30645246920106,4.30672404095661));
#37190=CARTESIAN_POINT('Ctrl Pts',(20.9595673929083,0.148398440326279,4.40042000858165));
#37191=CARTESIAN_POINT('Ctrl Pts',(20.9720603441653,0.0395501167658222,
4.4158270594931));
#37192=CARTESIAN_POINT('Ctrl Pts',(20.9766006560786,-4.48287659652116E-6,
4.41584197426197));
#37193=CARTESIAN_POINT('Ctrl Pts',(20.7733993439214,3.95676620551077E-6,
4.41590779860895));
#37194=CARTESIAN_POINT('Ctrl Pts',(20.7809111910678,-0.0654084660523611,
4.41587519962517));
#37195=CARTESIAN_POINT('Ctrl Pts',(20.7963756775582,-0.200102595337945,
4.3835597345012));
#37196=CARTESIAN_POINT('Ctrl Pts',(20.8197928033922,-0.358062019934396,
4.24450842127602));
#37197=CARTESIAN_POINT('Ctrl Pts',(20.8436507214237,-0.431438726014498,
4.04305074550709));
#37198=CARTESIAN_POINT('Ctrl Pts',(20.867508639455,-0.399316990859146,3.83106596928302));
#37199=CARTESIAN_POINT('Ctrl Pts',(20.8913665574865,-0.269551332195825,
3.66039017609669));
#37200=CARTESIAN_POINT('Ctrl Pts',(20.9152244755179,-0.0738730526583281,
3.57275822989076));
#37201=CARTESIAN_POINT('Ctrl Pts',(20.9390823935493,0.139869212314499,3.58959853735383));
#37202=CARTESIAN_POINT('Ctrl Pts',(20.9629403115807,0.319409638666883,3.70679317993256));
#37203=CARTESIAN_POINT('Ctrl Pts',(20.9867982296122,0.420845711130686,3.8956848776653));
#37204=CARTESIAN_POINT('Ctrl Pts',(21.0106561476436,0.419373541863394,4.11008446384341));
#37205=CARTESIAN_POINT('Ctrl Pts',(21.034514065675,0.315353119032788,4.29756540021079));
#37206=CARTESIAN_POINT('Ctrl Pts',(21.0554284644342,0.156567902793621,4.39812991232556));
#37207=CARTESIAN_POINT('Ctrl Pts',(21.0683902238497,0.0436291721249729,
4.41581988245125));
#37208=CARTESIAN_POINT('Ctrl Pts',(21.0733993439214,-7.65157297121996E-6,
4.41584853425778));
#37209=CARTESIAN_POINT('Origin',(3.42660065607856,0.,4.));
#37210=CARTESIAN_POINT('',(20.3766006560786,0.000383027521040961,4.41597069455794));
#37211=CARTESIAN_POINT('',(20.4733993439214,0.000101608071013781,4.41586489633469));
#37212=CARTESIAN_POINT('',(3.42660065607856,4.87367679877478E-13,4.415875));
#37213=CARTESIAN_POINT('Ctrl Pts',(20.3766006560786,0.000383027521040954,
4.41597069455794));
#37214=CARTESIAN_POINT('Ctrl Pts',(20.3891496392578,-0.108893832387875,
4.41487837761012));
#37215=CARTESIAN_POINT('Ctrl Pts',(20.4176039011246,-0.35839559572325,4.31454223548297));
#37216=CARTESIAN_POINT('Ctrl Pts',(20.4540108023354,-0.457800032585507,
3.97025345815189));
#37217=CARTESIAN_POINT('Ctrl Pts',(20.4858213597105,-0.325993724402262,
3.71529210935379));
#37218=CARTESIAN_POINT('Ctrl Pts',(20.509679277742,-0.15096738523986,3.59329490328468));
#37219=CARTESIAN_POINT('Ctrl Pts',(20.5335371957734,0.0630371972956549,
3.57102347342756));
#37220=CARTESIAN_POINT('Ctrl Pts',(20.5573951138048,0.260511246441404,3.65349437971329));
#37221=CARTESIAN_POINT('Ctrl Pts',(20.5812530318362,0.394877283734959,3.82077798440408));
#37222=CARTESIAN_POINT('Ctrl Pts',(20.6051109498677,0.432370081305563,4.03184236506754));
#37223=CARTESIAN_POINT('Ctrl Pts',(20.6289688678991,0.364303478986858,4.23514367899931));
#37224=CARTESIAN_POINT('Ctrl Pts',(20.6527987699694,0.207251017164088,4.38076243960928));
#37225=CARTESIAN_POINT('Ctrl Pts',(20.6686760326959,0.0690052481014253,
4.41590835422812));
#37226=CARTESIAN_POINT('Ctrl Pts',(20.6766006560786,1.29076178055295E-6,
4.41591111076812));
#37227=CARTESIAN_POINT('Ctrl Pts',(20.4733993439214,0.000101608071013788,
4.4158648963347));
#37228=CARTESIAN_POINT('Ctrl Pts',(20.4775268795984,-0.0359150725839473,
4.41584626969953));
#37229=CARTESIAN_POINT('Ctrl Pts',(20.4896070546192,-0.141401612166324,
4.40227446254147));
#37230=CARTESIAN_POINT('Ctrl Pts',(20.5096398689838,-0.298255971346869,
4.31460392554555));
#37231=CARTESIAN_POINT('Ctrl Pts',(20.5334977870152,-0.412709509332759,
4.13311446574462));
#37232=CARTESIAN_POINT('Ctrl Pts',(20.5573557050466,-0.425936384696969,
3.91915434697803));
#37233=CARTESIAN_POINT('Ctrl Pts',(20.581213623078,-0.335173342752607,3.72492109335083));
#37234=CARTESIAN_POINT('Ctrl Pts',(20.6050715411095,-0.162364888615448,
3.59797442377207));
#37235=CARTESIAN_POINT('Ctrl Pts',(20.6289294591408,0.0501004451364318,
3.56932214892951));
#37236=CARTESIAN_POINT('Ctrl Pts',(20.6527873771723,0.250339089241223,3.64598859455508));
#37237=CARTESIAN_POINT('Ctrl Pts',(20.6766452952037,0.389350172549011,3.80921715950176));
#37238=CARTESIAN_POINT('Ctrl Pts',(20.7005032132352,0.433161330121289,4.01909908002448));
#37239=CARTESIAN_POINT('Ctrl Pts',(20.7243611312665,0.371049143609512,4.22430982617278));
#37240=CARTESIAN_POINT('Ctrl Pts',(20.748219049298,0.218207240773441,4.37467120177868));
#37241=CARTESIAN_POINT('Ctrl Pts',(20.7645651201829,0.0769305199015265,
4.41491906931248));
#37242=CARTESIAN_POINT('Ctrl Pts',(20.772958551724,0.00384233167249433,
4.41590971150433));
#37243=CARTESIAN_POINT('Ctrl Pts',(20.7733993439214,3.95676620551077E-6,
4.41590779860895));
#37244=CARTESIAN_POINT('Origin',(3.42660065607856,0.,4.));
#37245=CARTESIAN_POINT('',(20.0766006560786,-0.000186622634748148,4.41645953600834));
#37246=CARTESIAN_POINT('',(20.1733993439214,-0.000111611226006447,4.41653056081536));
#37247=CARTESIAN_POINT('',(3.42660065607856,4.87367679877478E-13,4.415875));
#37248=CARTESIAN_POINT('Ctrl Pts',(20.0766006560786,-0.000186622634748109,
4.41645953600834));
#37249=CARTESIAN_POINT('Ctrl Pts',(20.0778126884445,-0.0107019642254321,
4.4165186149328));
#37250=CARTESIAN_POINT('Ctrl Pts',(20.0949299994981,-0.159149739060163,
4.41138240526969));
#37251=CARTESIAN_POINT('Ctrl Pts',(20.1279525892393,-0.432744382500041,
4.23375285658289));
#37252=CARTESIAN_POINT('Ctrl Pts',(20.1756684253021,-0.430649333670284,
3.76246031529274));
#37253=CARTESIAN_POINT('Ctrl Pts',(20.223384261365,-0.033136228617316,3.50924504180455));
#37254=CARTESIAN_POINT('Ctrl Pts',(20.2711000974278,0.394908089060633,3.70680919012016));
#37255=CARTESIAN_POINT('Ctrl Pts',(20.3188159334906,0.460110046434968,4.17340395051402));
#37256=CARTESIAN_POINT('Ctrl Pts',(20.3539827863742,0.197028357007358,4.40022211154544));
#37257=CARTESIAN_POINT('Ctrl Pts',(20.3732443605702,0.0296097328916507,
4.416262840815));
#37258=CARTESIAN_POINT('Ctrl Pts',(20.3766006560786,0.000383027521040954,
4.41597069455794));
#37259=CARTESIAN_POINT('Ctrl Pts',(20.1733993439214,-0.000111611226006447,
4.41653056081536));
#37260=CARTESIAN_POINT('Ctrl Pts',(20.1741425681289,-0.00655727229825777,
4.41655465488103));
#37261=CARTESIAN_POINT('Ctrl Pts',(20.190791071024,-0.150919726673813,4.41348743992374));
#37262=CARTESIAN_POINT('Ctrl Pts',(20.2233448526067,-0.425711472830213,
4.24633918020534));
#37263=CARTESIAN_POINT('Ctrl Pts',(20.2710606886696,-0.437384262562023,
3.77535541015343));
#37264=CARTESIAN_POINT('Ctrl Pts',(20.3187765247324,-0.0477164433392854,
3.51022640082505));
#37265=CARTESIAN_POINT('Ctrl Pts',(20.3664923607953,0.386374384143037,3.69571627142296));
#37266=CARTESIAN_POINT('Ctrl Pts',(20.4062555575143,0.45143962727185,4.08165775845481));
#37267=CARTESIAN_POINT('Ctrl Pts',(20.4380661148895,0.291471375703242,4.31996082336987));
#37268=CARTESIAN_POINT('Ctrl Pts',(20.4577964972439,0.136183087716603,4.40372206768731));
#37269=CARTESIAN_POINT('Ctrl Pts',(20.4695742402546,0.0334792813416625,
4.41588215816259));
#37270=CARTESIAN_POINT('Ctrl Pts',(20.4733993439214,0.000101608071013788,
4.4158648963347));
#37271=CARTESIAN_POINT('Origin',(3.42660065607856,0.,4.));
#37272=CARTESIAN_POINT('',(19.7766006560786,-0.000280998963924209,4.41539029291088));
#37273=CARTESIAN_POINT('',(19.8733993439214,-0.000322938566065189,4.41548189938477));
#37274=CARTESIAN_POINT('',(3.42660065607856,4.87367679877478E-13,4.415875));
#37275=CARTESIAN_POINT('Ctrl Pts',(19.7766006560786,-0.000280998963924181,
4.41539029291088));
#37276=CARTESIAN_POINT('Ctrl Pts',(19.7823810163188,-0.0507615353771658,
4.41570272077311));
#37277=CARTESIAN_POINT('Ctrl Pts',(19.8040666552467,-0.23976299482565,4.3837755623668));
#37278=CARTESIAN_POINT('Ctrl Pts',(19.8416575728622,-0.481212499922896,
4.10168523844358));
#37279=CARTESIAN_POINT('Ctrl Pts',(19.8893734089251,-0.345789702982467,
3.65023692191923));
#37280=CARTESIAN_POINT('Ctrl Pts',(19.9370892449879,0.107175910646637,3.51998011832295));
#37281=CARTESIAN_POINT('Ctrl Pts',(19.9848050810508,0.461722480014006,3.83053541934297));
#37282=CARTESIAN_POINT('Ctrl Pts',(20.0313088847476,0.394022427012164,4.28486673161383));
#37283=CARTESIAN_POINT('Ctrl Pts',(20.0619074097569,0.127288937001902,4.4157433330307));
#37284=CARTESIAN_POINT('Ctrl Pts',(20.0766006560786,-0.000186622634748109,
4.41645953600834));
#37285=CARTESIAN_POINT('Ctrl Pts',(19.8733993439214,-0.000322938566065196,
4.41548189938477));
#37286=CARTESIAN_POINT('Ctrl Pts',(19.8787108960032,-0.0466836533228258,
4.41581668875846));
#37287=CARTESIAN_POINT('Ctrl Pts',(19.8999277267727,-0.231469429366377,
4.38724295332581));
#37288=CARTESIAN_POINT('Ctrl Pts',(19.9370498362297,-0.47800980043334,4.11581244897344));
#37289=CARTESIAN_POINT('Ctrl Pts',(19.9847656722926,-0.355939225796451,
3.66057517601247));
#37290=CARTESIAN_POINT('Ctrl Pts',(20.0324815083554,0.0929888682922082,
3.51702731322357));
#37291=CARTESIAN_POINT('Ctrl Pts',(20.0801973444182,0.456536973876988,3.81701888067549));
#37292=CARTESIAN_POINT('Ctrl Pts',(20.1271699562736,0.401683300383188,4.27772103607547));
#37293=CARTESIAN_POINT('Ctrl Pts',(20.1582372894413,0.131382308576697,4.41603903277767));
#37294=CARTESIAN_POINT('Ctrl Pts',(20.1733993439214,-0.000111611226006447,
4.41653056081536));
#37295=CARTESIAN_POINT('Origin',(3.42660065607856,0.,4.));
#37296=CARTESIAN_POINT('',(19.4766006560786,0.000302289446139524,4.41543216566181));
#37297=CARTESIAN_POINT('',(19.5733993439214,0.000255464646300079,4.41534829948978));
#37298=CARTESIAN_POINT('',(3.42660065607856,4.87367679877478E-13,4.415875));
#37299=CARTESIAN_POINT('Ctrl Pts',(19.4766006560786,0.000302289446139546,
4.41543216566181));
#37300=CARTESIAN_POINT('Ctrl Pts',(19.4869493441932,-0.0900510892866153,
4.41482666801407));
#37301=CARTESIAN_POINT('Ctrl Pts',(19.5132033109954,-0.320168095705801,
4.3413809155508));
#37302=CARTESIAN_POINT('Ctrl Pts',(19.5553625564852,-0.490312813065352,
3.96128857502183));
#37303=CARTESIAN_POINT('Ctrl Pts',(19.603078392548,-0.232620797759261,3.56664935826393));
#37304=CARTESIAN_POINT('Ctrl Pts',(19.6507942286109,0.238690449241969,3.56996267500769));
#37305=CARTESIAN_POINT('Ctrl Pts',(19.6985100646737,0.490808633485035,3.96818593857384));
#37306=CARTESIAN_POINT('Ctrl Pts',(19.7404455404963,0.316268156276861,4.34384396940031));
#37307=CARTESIAN_POINT('Ctrl Pts',(19.7664757376312,0.0881410531427697,
4.41484304213512));
#37308=CARTESIAN_POINT('Ctrl Pts',(19.7766006560786,-0.000280998963924181,
4.41539029291088));
#37309=CARTESIAN_POINT('Ctrl Pts',(19.5733993439214,0.000255464646300094,
4.41534829948978));
#37310=CARTESIAN_POINT('Ctrl Pts',(19.5832792238775,-0.0860485087386658,
4.41486588036018));
#37311=CARTESIAN_POINT('Ctrl Pts',(19.6090643825213,-0.311990568344336,
4.34649332259355));
#37312=CARTESIAN_POINT('Ctrl Pts',(19.6507548198527,-0.491240257057309,
3.97574594767572));
#37313=CARTESIAN_POINT('Ctrl Pts',(19.6984706559155,-0.245282818621706,
3.57368850533185));
#37314=CARTESIAN_POINT('Ctrl Pts',(19.7461864919783,0.225921452997342,3.56311925573479));
#37315=CARTESIAN_POINT('Ctrl Pts',(19.7939023280412,0.489658867576397,3.95374471702426));
#37316=CARTESIAN_POINT('Ctrl Pts',(19.8363066120222,0.324430886710512,4.33863507066385));
#37317=CARTESIAN_POINT('Ctrl Pts',(19.8628056173156,0.0921420753912029,
4.4148141723173));
#37318=CARTESIAN_POINT('Ctrl Pts',(19.8733993439214,-0.000322938566065196,
4.41548189938477));
#37319=CARTESIAN_POINT('Origin',(3.42660065607856,0.,4.));
#37320=CARTESIAN_POINT('',(19.1766006560786,0.000155842099650094,4.41649089206047));
#37321=CARTESIAN_POINT('',(19.2733993439214,0.000220989830587742,4.4164164649367));
#37322=CARTESIAN_POINT('',(3.42660065607856,4.87367679877478E-13,4.415875));
#37323=CARTESIAN_POINT('Ctrl Pts',(19.1766006560786,0.000155842099650088,
4.41649089206047));
#37324=CARTESIAN_POINT('Ctrl Pts',(19.1915176720675,-0.129233580897558,
4.41587069825202));
#37325=CARTESIAN_POINT('Ctrl Pts',(19.2223399667441,-0.397695790553126,
4.28149179527637));
#37326=CARTESIAN_POINT('Ctrl Pts',(19.2690675401082,-0.459293044881286,
3.82405931712685));
#37327=CARTESIAN_POINT('Ctrl Pts',(19.316783376171,-0.100417177000157,3.51852142809106));
#37328=CARTESIAN_POINT('Ctrl Pts',(19.3644992122339,0.350673329058588,3.65513271950473));
#37329=CARTESIAN_POINT('Ctrl Pts',(19.4122150482967,0.479735122332443,4.10844094226069));
#37330=CARTESIAN_POINT('Ctrl Pts',(19.4495821962449,0.235804435834584,4.38544967282755));
#37331=CARTESIAN_POINT('Ctrl Pts',(19.4710440655056,0.0488163355692654,
4.4157572795781));
#37332=CARTESIAN_POINT('Ctrl Pts',(19.4766006560786,0.000302289446139546,
4.41543216566181));
#37333=CARTESIAN_POINT('Ctrl Pts',(19.2733993439214,0.000220989830587761,
4.4164164649367));
#37334=CARTESIAN_POINT('Ctrl Pts',(19.2878475517519,-0.125161313229646,
4.41561068768233));
#37335=CARTESIAN_POINT('Ctrl Pts',(19.31820103827,-0.389985711500173,4.28851341748863));
#37336=CARTESIAN_POINT('Ctrl Pts',(19.3644598034757,-0.464275578741542,
3.8376626582024));
#37337=CARTESIAN_POINT('Ctrl Pts',(19.4121756395385,-0.114554038379521,
3.52168776344319));
#37338=CARTESIAN_POINT('Ctrl Pts',(19.4598914756013,0.340364234683876,3.64495435060606));
#37339=CARTESIAN_POINT('Ctrl Pts',(19.5076073116642,0.482720800247919,4.09426482953845));
#37340=CARTESIAN_POINT('Ctrl Pts',(19.5454432677708,0.244097666198316,4.38190156491584));
#37341=CARTESIAN_POINT('Ctrl Pts',(19.5673739451899,0.0528892875329133,
4.41564251031262));
#37342=CARTESIAN_POINT('Ctrl Pts',(19.5733993439214,0.000255464646300094,
4.41534829948978));
#37343=CARTESIAN_POINT('Origin',(3.42660065607856,0.,4.));
#37344=CARTESIAN_POINT('',(18.8766006560785,-0.00038196507782994,4.41590683121974));
#37345=CARTESIAN_POINT('',(18.9733993439214,-0.000368287616214491,4.41603142687637));
#37346=CARTESIAN_POINT('',(3.42660065607856,4.87367679877478E-13,4.415875));
#37347=CARTESIAN_POINT('Ctrl Pts',(18.8766006560785,-0.000381965077829925,
4.41590683121974));
#37348=CARTESIAN_POINT('Ctrl Pts',(18.8801807212542,-0.0315488007868432,
4.41619587167324));
#37349=CARTESIAN_POINT('Ctrl Pts',(18.8996660651174,-0.200861076696893,
4.39874895857547));
#37350=CARTESIAN_POINT('Ctrl Pts',(18.9350566876684,-0.462607878309702,
4.16703046362027));
#37351=CARTESIAN_POINT('Ctrl Pts',(18.9827725237311,-0.39069124519864,3.70122654773242));
#37352=CARTESIAN_POINT('Ctrl Pts',(19.030488359794,0.0400031699426168,3.50979089028978));
#37353=CARTESIAN_POINT('Ctrl Pts',(19.0782041958568,0.433962058584907,3.76852180111673));
#37354=CARTESIAN_POINT('Ctrl Pts',(19.1259200319197,0.429406911488226,4.23982270375453));
#37355=CARTESIAN_POINT('Ctrl Pts',(19.1587188519936,0.155221332864305,4.41240136130926));
#37356=CARTESIAN_POINT('Ctrl Pts',(19.1756123933799,0.00872798149047904,
4.41653198033223));
#37357=CARTESIAN_POINT('Ctrl Pts',(19.1766006560786,0.000155842099650088,
4.41649089206047));
#37358=CARTESIAN_POINT('Ctrl Pts',(18.9733993439214,-0.000368287616214533,
4.41603142687637));
#37359=CARTESIAN_POINT('Ctrl Pts',(18.9765106009386,-0.0274330213022572,
4.4162811262788));
#37360=CARTESIAN_POINT('Ctrl Pts',(18.9955271366434,-0.192586232161443,
4.40152565608163));
#37361=CARTESIAN_POINT('Ctrl Pts',(19.0304489510358,-0.457487847288108,
4.18058265263639));
#37362=CARTESIAN_POINT('Ctrl Pts',(19.0781647870987,-0.399321187381313,
3.71286272589862));
#37363=CARTESIAN_POINT('Ctrl Pts',(19.1258806231614,0.0255482632835279,
3.50882537619781));
#37364=CARTESIAN_POINT('Ctrl Pts',(19.1735964592243,0.426956350589889,3.75584124112414));
#37365=CARTESIAN_POINT('Ctrl Pts',(19.2213122952871,0.436283851722622,4.22707185138688));
#37366=CARTESIAN_POINT('Ctrl Pts',(19.2545799235195,0.163455264474221,4.41023200720537));
#37367=CARTESIAN_POINT('Ctrl Pts',(19.2719422730642,0.0128655269200745,
4.41649772584937));
#37368=CARTESIAN_POINT('Ctrl Pts',(19.2733993439214,0.000220989830587761,
4.4164164649367));
#37369=CARTESIAN_POINT('Origin',(3.42660065607856,0.,4.));
#37370=CARTESIAN_POINT('',(18.5766006560786,2.82854505807383E-5,4.41518799822097));
#37371=CARTESIAN_POINT('',(18.6733993439214,-3.94222854199766E-5,4.41518963037823));
#37372=CARTESIAN_POINT('',(3.42660065607856,4.87367679877478E-13,4.415875));
#37373=CARTESIAN_POINT('Ctrl Pts',(18.5766006560786,2.82854505807215E-5,
4.41518799822097));
#37374=CARTESIAN_POINT('Ctrl Pts',(18.5847490491285,-0.0712192880865648,
4.41514491699706));
#37375=CARTESIAN_POINT('Ctrl Pts',(18.6088027208661,-0.281596950705947,
4.36382162423513));
#37376=CARTESIAN_POINT('Ctrl Pts',(18.6487616712913,-0.49096944006335,4.0292272779409));
#37377=CARTESIAN_POINT('Ctrl Pts',(18.6964775073541,-0.290120809601049,
3.60284116440841));
#37378=CARTESIAN_POINT('Ctrl Pts',(18.744193343417,0.177150224400508,3.54117212067402));
#37379=CARTESIAN_POINT('Ctrl Pts',(18.7919091794797,0.481741481528227,3.90085177849878));
#37380=CARTESIAN_POINT('Ctrl Pts',(18.836044950367,0.354281053487698,4.31776308733785));
#37381=CARTESIAN_POINT('Ctrl Pts',(18.8642754425666,0.106917172161326,4.4149117417093));
#37382=CARTESIAN_POINT('Ctrl Pts',(18.8766006560785,-0.000381965077829925,
4.41590683121974));
#37383=CARTESIAN_POINT('Ctrl Pts',(18.6733993439214,-3.94222854199489E-5,
4.41518963037823));
#37384=CARTESIAN_POINT('Ctrl Pts',(18.6810789288129,-0.0671871929144198,
4.41524623173262));
#37385=CARTESIAN_POINT('Ctrl Pts',(18.704663792392,-0.273330541024821,4.36810584919535));
#37386=CARTESIAN_POINT('Ctrl Pts',(18.7441539346588,-0.489895661254576,
4.0436745456279));
#37387=CARTESIAN_POINT('Ctrl Pts',(18.7918697707216,-0.301692008317894,
3.6115580391236));
#37388=CARTESIAN_POINT('Ctrl Pts',(18.8395856067845,0.163560057986223,3.53615376224111));
#37389=CARTESIAN_POINT('Ctrl Pts',(18.8873014428472,0.478612406344963,3.88670662268212));
#37390=CARTESIAN_POINT('Ctrl Pts',(18.9319060218929,0.362263203066427,4.31165738429376));
#37391=CARTESIAN_POINT('Ctrl Pts',(18.960605322251,0.110926532249199,4.41500462017153));
#37392=CARTESIAN_POINT('Ctrl Pts',(18.9733993439214,-0.000368287616214533,
4.41603142687637));
#37393=CARTESIAN_POINT('Origin',(3.42660065607856,0.,4.));
#37394=CARTESIAN_POINT('',(18.2766006560786,0.000371443240938316,4.41601098728712));
#37395=CARTESIAN_POINT('',(18.3733993439214,0.000382963303967143,4.41588626824893));
#37396=CARTESIAN_POINT('',(3.42660065607856,4.87367679877478E-13,4.415875));
#37397=CARTESIAN_POINT('Ctrl Pts',(18.2766006560785,0.000371443240938293,
4.41601098728712));
#37398=CARTESIAN_POINT('Ctrl Pts',(18.2893173770028,-0.110264925490287,
4.41498710445335));
#37399=CARTESIAN_POINT('Ctrl Pts',(18.3179393766147,-0.360950442388199,
4.31267773405576));
#37400=CARTESIAN_POINT('Ctrl Pts',(18.3624666549143,-0.479157019140895,
3.88903254594255));
#37401=CARTESIAN_POINT('Ctrl Pts',(18.4101824909771,-0.165810997523729,
3.5369536330429));
#37402=CARTESIAN_POINT('Ctrl Pts',(18.4578983270399,0.299801814449608,3.61009732380414));
#37403=CARTESIAN_POINT('Ctrl Pts',(18.5056141631028,0.49010200717001,4.04129464153984));
#37404=CARTESIAN_POINT('Ctrl Pts',(18.5451816061157,0.274694351318236,4.36741107590602));
#37405=CARTESIAN_POINT('Ctrl Pts',(18.5688437704409,0.0678526130816757,
4.41522900951301));
#37406=CARTESIAN_POINT('Ctrl Pts',(18.5766006560786,2.82854505807215E-5,
4.41518799822097));
#37407=CARTESIAN_POINT('Ctrl Pts',(18.3733993439214,0.000382963303967157,
4.41588626824893));
#37408=CARTESIAN_POINT('Ctrl Pts',(18.3856472566872,-0.106256708375174,
4.41489942083623));
#37409=CARTESIAN_POINT('Ctrl Pts',(18.4138004481407,-0.352960303644862,
4.31875095920395));
#37410=CARTESIAN_POINT('Ctrl Pts',(18.4578589182817,-0.482217355384067,
3.90319273261591));
#37411=CARTESIAN_POINT('Ctrl Pts',(18.5055747543446,-0.179376629827252,
3.54203793877243));
#37412=CARTESIAN_POINT('Ctrl Pts',(18.5532905904074,0.288188414964166,3.60143675240633));
#37413=CARTESIAN_POINT('Ctrl Pts',(18.6010064264702,0.491105603945206,4.02684232898929));
#37414=CARTESIAN_POINT('Ctrl Pts',(18.6410426776416,0.282958802096416,4.36309886994028));
#37415=CARTESIAN_POINT('Ctrl Pts',(18.6651736501253,0.0718833454275778,
4.41512900400112));
#37416=CARTESIAN_POINT('Ctrl Pts',(18.6733993439214,-3.94222854199489E-5,
4.41518963037823));
#37417=CARTESIAN_POINT('Origin',(3.42660065607856,0.,4.));
#37418=CARTESIAN_POINT('',(17.9766006560786,-0.000210814279110197,4.41643020456723));
#37419=CARTESIAN_POINT('',(18.0733993439214,-0.000144384975211464,4.41650095473263));
#37420=CARTESIAN_POINT('',(3.42660065607856,4.87367679877478E-13,4.415875));
#37421=CARTESIAN_POINT('Ctrl Pts',(17.9766006560786,-0.000210814279110157,
4.41643020456723));
#37422=CARTESIAN_POINT('Ctrl Pts',(17.9779804261896,-0.0121834889824064,
4.41650424974197));
#37423=CARTESIAN_POINT('Ctrl Pts',(17.9952654749882,-0.162096873242269,
4.41059855206721));
#37424=CARTESIAN_POINT('Ctrl Pts',(18.0284558024744,-0.435175833605105,
4.22918817311999));
#37425=CARTESIAN_POINT('Ctrl Pts',(18.0761716385373,-0.428137176707308,
3.75791781814212));
#37426=CARTESIAN_POINT('Ctrl Pts',(18.1238874746,-0.0279335627019553,3.5089552556775));
#37427=CARTESIAN_POINT('Ctrl Pts',(18.1716033106629,0.397921871745719,3.71092663761881));
#37428=CARTESIAN_POINT('Ctrl Pts',(18.2193191467257,0.458359528554279,4.17835853620019));
#37429=CARTESIAN_POINT('Ctrl Pts',(18.2543182618643,0.193950155243433,4.40107745006558));
#37430=CARTESIAN_POINT('Ctrl Pts',(18.2734120983152,0.0281121206155762,
4.41626771302466));
#37431=CARTESIAN_POINT('Ctrl Pts',(18.2766006560785,0.000371443240938293,
4.41601098728712));
#37432=CARTESIAN_POINT('Ctrl Pts',(18.0733993439214,-0.000144384975211439,
4.41650095473263));
#37433=CARTESIAN_POINT('Ctrl Pts',(18.0743103058739,-0.00804551399413891,
4.41653639380418));
#37434=CARTESIAN_POINT('Ctrl Pts',(18.0911265465141,-0.153864670001157,
4.41274680364665));
#37435=CARTESIAN_POINT('Ctrl Pts',(18.1238480658419,-0.428237044548737,
4.24190547436581));
#37436=CARTESIAN_POINT('Ctrl Pts',(18.1715639019047,-0.435081213444543,
3.7706322547532));
#37437=CARTESIAN_POINT('Ctrl Pts',(18.2192797379675,-0.0423836094492617,
3.50999096487715));
#37438=CARTESIAN_POINT('Ctrl Pts',(18.2669955740304,0.389235515258945,3.69933251171255));
#37439=CARTESIAN_POINT('Ctrl Pts',(18.3147114100932,0.463413677146622,4.16478163940629));
#37440=CARTESIAN_POINT('Ctrl Pts',(18.3501793333902,0.202226156869028,4.39827758107438));
#37441=CARTESIAN_POINT('Ctrl Pts',(18.3697419779996,0.0322267809866215,
4.41618095209965));
#37442=CARTESIAN_POINT('Ctrl Pts',(18.3733993439214,0.000382963303967157,
4.41588626824893));
#37443=CARTESIAN_POINT('Origin',(3.42660065607856,0.,4.));
#37444=CARTESIAN_POINT('',(17.6766006560786,-0.000263771022561219,4.41536107794487));
#37445=CARTESIAN_POINT('',(17.7733993439214,-0.000309142357869163,4.41544738986064));
#37446=CARTESIAN_POINT('',(3.42660065607856,4.87367679877478E-13,4.415875));
#37447=CARTESIAN_POINT('Ctrl Pts',(17.6766006560786,-0.000263771022561289,
4.41536107794487));
#37448=CARTESIAN_POINT('Ctrl Pts',(17.6825487540639,-0.0522183410383149,
4.41566152300153));
#37449=CARTESIAN_POINT('Ctrl Pts',(17.7044021307368,-0.24273028972288,4.38249735042552));
#37450=CARTESIAN_POINT('Ctrl Pts',(17.7421607860973,-0.48225726547346,4.09660825404716));
#37451=CARTESIAN_POINT('Ctrl Pts',(17.7898766221602,-0.342084653792828,
3.64661166616396));
#37452=CARTESIAN_POINT('Ctrl Pts',(17.837592458223,0.112229559114723,3.52113702282083));
#37453=CARTESIAN_POINT('Ctrl Pts',(17.8853082942859,0.463481641013499,3.83540961967535));
#37454=CARTESIAN_POINT('Ctrl Pts',(17.9316443602377,0.391261919872151,4.28736986940801));
#37455=CARTESIAN_POINT('Ctrl Pts',(17.962075147502,0.125831334120538,4.41565069513148));
#37456=CARTESIAN_POINT('Ctrl Pts',(17.9766006560786,-0.000210814279110157,
4.41643020456723));
#37457=CARTESIAN_POINT('Ctrl Pts',(17.7733993439214,-0.000309142357869142,
4.41544738986064));
#37458=CARTESIAN_POINT('Ctrl Pts',(17.7788786337482,-0.0481438769258273,
4.41577602216682));
#37459=CARTESIAN_POINT('Ctrl Pts',(17.8002632022627,-0.23443694547481,4.38601982759396));
#37460=CARTESIAN_POINT('Ctrl Pts',(17.8375530494648,-0.479202773223469,
4.11076970247734));
#37461=CARTESIAN_POINT('Ctrl Pts',(17.8852688855277,-0.352344189444135,
3.65683998336499));
#37462=CARTESIAN_POINT('Ctrl Pts',(17.9329847215905,0.0980774850139738,
3.51803938772416));
#37463=CARTESIAN_POINT('Ctrl Pts',(17.9807005576534,0.458433095867658,3.82183063825345));
#37464=CARTESIAN_POINT('Ctrl Pts',(18.0275054317636,0.3989600628602,4.28031410431705));
#37465=CARTESIAN_POINT('Ctrl Pts',(18.0584050271863,0.129907183855675,4.41591763216682));
#37466=CARTESIAN_POINT('Ctrl Pts',(18.0733993439214,-0.000144384975211439,
4.41650095473263));
#37467=CARTESIAN_POINT('Origin',(3.42660065607856,0.,4.));
#37468=CARTESIAN_POINT('',(17.3766006560786,0.000316824918469052,4.41546566829253));
#37469=CARTESIAN_POINT('',(17.4733993439214,0.000273208168652644,4.41537657040552));
#37470=CARTESIAN_POINT('',(3.42660065607856,4.87367679877478E-13,4.415875));
#37471=CARTESIAN_POINT('Ctrl Pts',(17.3766006560786,0.000316824918469058,
4.41546566829253));
#37472=CARTESIAN_POINT('Ctrl Pts',(17.3871170819382,-0.0914824399419538,
4.4148173972429));
#37473=CARTESIAN_POINT('Ctrl Pts',(17.4135387864855,-0.323087181591141,
4.33950699049548));
#37474=CARTESIAN_POINT('Ctrl Pts',(17.4558657697204,-0.489877595596684,
3.956123284257));
#37475=CARTESIAN_POINT('Ctrl Pts',(17.5035816057832,-0.228040769637767,
3.56422180844494));
#37476=CARTESIAN_POINT('Ctrl Pts',(17.551297441846,0.243209403937772,3.57250215124727));
#37477=CARTESIAN_POINT('Ctrl Pts',(17.5990132779089,0.491116639619549,3.97336034645914));
#37478=CARTESIAN_POINT('Ctrl Pts',(17.6407810159864,0.313340775136121,4.34566293955037));
#37479=CARTESIAN_POINT('Ctrl Pts',(17.6666434753763,0.0867087440962768,
4.41485812965324));
#37480=CARTESIAN_POINT('Ctrl Pts',(17.6766006560786,-0.000263771022561289,
4.41536107794487));
#37481=CARTESIAN_POINT('Ctrl Pts',(17.4733993439214,0.000273208168652693,
4.41537657040552));
#37482=CARTESIAN_POINT('Ctrl Pts',(17.4834469616226,-0.0874810350323011,
4.41484969107387));
#37483=CARTESIAN_POINT('Ctrl Pts',(17.5093998580114,-0.314919534962053,
4.34468516187688));
#37484=CARTESIAN_POINT('Ctrl Pts',(17.5512580330878,-0.490957336521241,
3.97057010757845));
#37485=CARTESIAN_POINT('Ctrl Pts',(17.5989738691507,-0.240776309167652,
3.57112706567612));
#37486=CARTESIAN_POINT('Ctrl Pts',(17.6466897052135,0.230513307714322,3.56552463842171));
#37487=CARTESIAN_POINT('Ctrl Pts',(17.6944055412763,0.490119007219086,3.95890762096741));
#37488=CARTESIAN_POINT('Ctrl Pts',(17.7366420875123,0.321513805022658,4.34052027563639));
#37489=CARTESIAN_POINT('Ctrl Pts',(17.7629733550606,0.090710757213051,4.41482206853766));
#37490=CARTESIAN_POINT('Ctrl Pts',(17.7733993439214,-0.000309142357869142,
4.41544738986064));
#37491=CARTESIAN_POINT('Origin',(3.42660065607856,0.,4.));
#37492=CARTESIAN_POINT('',(17.0766006560786,0.000130763213737631,4.41651185352269));
#37493=CARTESIAN_POINT('',(17.1733993439214,0.000198609043858391,4.41644558073401));
#37494=CARTESIAN_POINT('',(3.42660065607856,4.87367679877478E-13,4.415875));
#37495=CARTESIAN_POINT('Ctrl Pts',(17.0766006560786,0.000130763213737628,
4.41651185352269));
#37496=CARTESIAN_POINT('Ctrl Pts',(17.0916854098125,-0.130696083011285,
4.41597403242798));
#37497=CARTESIAN_POINT('Ctrl Pts',(17.1226754422341,-0.400436570105288,
4.2789290971087));
#37498=CARTESIAN_POINT('Ctrl Pts',(17.1695707533433,-0.457413284126125,
3.81922856321607));
#37499=CARTESIAN_POINT('Ctrl Pts',(17.2172865894061,-0.0953372598908034,
3.51748986360026));
#37500=CARTESIAN_POINT('Ctrl Pts',(17.265002425469,0.354288437054553,3.6588476466131));
#37501=CARTESIAN_POINT('Ctrl Pts',(17.3127182615318,0.478565610824392,4.11349088504481));
#37502=CARTESIAN_POINT('Ctrl Pts',(17.349917671735,0.232837083242772,4.38668157013213));
#37503=CARTESIAN_POINT('Ctrl Pts',(17.3712118032506,0.0473568302064652,
4.41579785693967));
#37504=CARTESIAN_POINT('Ctrl Pts',(17.3766006560786,0.000316824918469058,
4.41546566829253));
#37505=CARTESIAN_POINT('Ctrl Pts',(17.1733993439214,0.000198609043858397,
4.41644558073401));
#37506=CARTESIAN_POINT('Ctrl Pts',(17.1880152894969,-0.126615914365149,
4.41569892234974));
#37507=CARTESIAN_POINT('Ctrl Pts',(17.2185365137601,-0.392752582168809,
4.28602487069057));
#37508=CARTESIAN_POINT('Ctrl Pts',(17.2649630167107,-0.462538907526291,
3.83277863809798));
#37509=CARTESIAN_POINT('Ctrl Pts',(17.3126788527736,-0.109506707187599,
3.52050703244687));
#37510=CARTESIAN_POINT('Ctrl Pts',(17.3603946888365,0.344087187338735,3.64856119684745));
#37511=CARTESIAN_POINT('Ctrl Pts',(17.4081105248993,0.481700523269991,4.09934702176407));
#37512=CARTESIAN_POINT('Ctrl Pts',(17.4457787432609,0.241130489326423,4.3831889686244));
#37513=CARTESIAN_POINT('Ctrl Pts',(17.467541682935,0.0514330574063097,4.41568373580506));
#37514=CARTESIAN_POINT('Ctrl Pts',(17.4733993439214,0.000273208168652693,
4.41537657040552));
#37515=CARTESIAN_POINT('Origin',(3.42660065607856,0.,4.));
#37516=CARTESIAN_POINT('',(16.7766006560786,-0.000383680820852129,4.41586226484778));
#37517=CARTESIAN_POINT('',(16.8733993439214,-0.000374684679869397,4.41598699190495));
#37518=CARTESIAN_POINT('',(3.42660065607856,4.87367679877478E-13,4.415875));
#37519=CARTESIAN_POINT('Ctrl Pts',(16.7766006560786,-0.000383680820852189,
4.41586226484779));
#37520=CARTESIAN_POINT('Ctrl Pts',(16.7803484589992,-0.0330197262611539,
4.41616320579436));
#37521=CARTESIAN_POINT('Ctrl Pts',(16.8000015406075,-0.203823433586872,
4.39772119122577));
#37522=CARTESIAN_POINT('Ctrl Pts',(16.8355599009034,-0.464342533291602,
4.16214572651883));
#37523=CARTESIAN_POINT('Ctrl Pts',(16.8832757369663,-0.387520750342007,
3.69712561530174));
#37524=CARTESIAN_POINT('Ctrl Pts',(16.9309915730291,0.0451673004198413,
3.51023971187451));
#37525=CARTESIAN_POINT('Ctrl Pts',(16.978707409092,0.436377524217892,3.7731082169636));
#37526=CARTESIAN_POINT('Ctrl Pts',(17.0264232451548,0.426855552995382,4.24433493759383));
#37527=CARTESIAN_POINT('Ctrl Pts',(17.0590543274837,0.152277829190936,4.41314658311127));
#37528=CARTESIAN_POINT('Ctrl Pts',(17.0757801311249,0.00724700082869906,
4.41654110793655));
#37529=CARTESIAN_POINT('Ctrl Pts',(17.0766006560786,0.000130763213737628,
4.41651185352269));
#37530=CARTESIAN_POINT('Ctrl Pts',(16.8733993439214,-0.000374684679869387,
4.41598699190495));
#37531=CARTESIAN_POINT('Ctrl Pts',(16.8766783386836,-0.0289064002234668,
4.4162516892709));
#37532=CARTESIAN_POINT('Ctrl Pts',(16.8958626121335,-0.195546116663039,
4.40054826733105));
#37533=CARTESIAN_POINT('Ctrl Pts',(16.9309521642709,-0.459365614209645,
4.17575112327883));
#37534=CARTESIAN_POINT('Ctrl Pts',(16.9786680003337,-0.396272847821079,
3.70867019559999));
#37535=CARTESIAN_POINT('Ctrl Pts',(17.0263838363966,0.0307233721630972,
3.5091219099869));
#37536=CARTESIAN_POINT('Ctrl Pts',(17.0740996724594,0.429505846750062,3.76035452756312));
#37537=CARTESIAN_POINT('Ctrl Pts',(17.1218155085223,0.433866493469502,4.23165726989771));
#37538=CARTESIAN_POINT('Ctrl Pts',(17.1549153990096,0.160507997039396,4.41102293437065));
#37539=CARTESIAN_POINT('Ctrl Pts',(17.1721100108093,0.0113854435377776,
4.41651144656345));
#37540=CARTESIAN_POINT('Ctrl Pts',(17.1733993439214,0.000198609043858397,
4.41644558073401));
#37541=CARTESIAN_POINT('Origin',(3.42660065607856,0.,4.));
#37542=CARTESIAN_POINT('',(16.4766006560786,5.2409936866527E-5,4.41519222098806));
#37543=CARTESIAN_POINT('',(16.5733993439214,-1.52272386678698E-5,4.41518677123726));
#37544=CARTESIAN_POINT('',(3.42660065607856,4.87367679877478E-13,4.415875));
#37545=CARTESIAN_POINT('Ctrl Pts',(16.4766006560786,5.2409936866539E-5,
4.41519222098806));
#37546=CARTESIAN_POINT('Ctrl Pts',(16.4849167868736,-0.0726599781719204,
4.41511070701236));
#37547=CARTESIAN_POINT('Ctrl Pts',(16.5091381963562,-0.284551613766983,
4.36224737480062));
#37548=CARTESIAN_POINT('Ctrl Pts',(16.5492648845264,-0.4912502013546,4.02405128938415));
#37549=CARTESIAN_POINT('Ctrl Pts',(16.5969807205893,-0.285919008936969,
3.59980561575594));
#37550=CARTESIAN_POINT('Ctrl Pts',(16.6446965566521,0.181976008816936,3.54306460296116));
#37551=CARTESIAN_POINT('Ctrl Pts',(16.6924123927149,0.482759657613431,3.90593439612197));
#37552=CARTESIAN_POINT('Ctrl Pts',(16.7363804258571,0.351413532087107,4.31989995948535));
#37553=CARTESIAN_POINT('Ctrl Pts',(16.7644431803116,0.105484194296011,4.41488604428797));
#37554=CARTESIAN_POINT('Ctrl Pts',(16.7766006560786,-0.000383680820852189,
4.41586226484779));
#37555=CARTESIAN_POINT('Ctrl Pts',(16.5733993439214,-1.52272386678906E-5,
4.41518677123726));
#37556=CARTESIAN_POINT('Ctrl Pts',(16.5812466665579,-0.0686308195205231,
4.41520910309265));
#37557=CARTESIAN_POINT('Ctrl Pts',(16.6049992678821,-0.276289552895371,
4.36659242126669));
#37558=CARTESIAN_POINT('Ctrl Pts',(16.6446571478939,-0.490328743065594,
4.03850907134293));
#37559=CARTESIAN_POINT('Ctrl Pts',(16.6923729839567,-0.297581432841348,
3.60840005658827));
#37560=CARTESIAN_POINT('Ctrl Pts',(16.7400888200196,0.168439486040012,3.53790329540825));
#37561=CARTESIAN_POINT('Ctrl Pts',(16.7878046560824,0.479779833116189,3.89175704832657));
#37562=CARTESIAN_POINT('Ctrl Pts',(16.832241497383,0.359412856911567,4.31386464726761));
#37563=CARTESIAN_POINT('Ctrl Pts',(16.860773059996,0.109491163683573,4.41496773315674));
#37564=CARTESIAN_POINT('Ctrl Pts',(16.8733993439214,-0.000374684679869387,
4.41598699190495));
#37565=CARTESIAN_POINT('Origin',(3.42660065607856,0.,4.));
#37566=CARTESIAN_POINT('',(16.1766006560786,0.000364146841390381,4.41605523138122));
#37567=CARTESIAN_POINT('',(16.2733993439214,0.000380345806842055,4.41593091837313));
#37568=CARTESIAN_POINT('',(3.42660065607856,4.87367679877478E-13,4.415875));
#37569=CARTESIAN_POINT('Ctrl Pts',(16.1766006560786,0.000364146841390366,
4.41605523138122));
#37570=CARTESIAN_POINT('Ctrl Pts',(16.1894851147479,-0.111700864104492,
4.41502624848758));
#37571=CARTESIAN_POINT('Ctrl Pts',(16.2182748521048,-0.363797281821349,
4.31045679267864));
#37572=CARTESIAN_POINT('Ctrl Pts',(16.2629698681494,-0.477960913216358,
3.88398883549692));
#37573=CARTESIAN_POINT('Ctrl Pts',(16.3106857042122,-0.160921706883503,
3.53523185446324));
#37574=CARTESIAN_POINT('Ctrl Pts',(16.358401540275,0.303894378979202,3.6132786128531));
#37575=CARTESIAN_POINT('Ctrl Pts',(16.4061173763379,0.489639580609251,4.04645757153336));
#37576=CARTESIAN_POINT('Ctrl Pts',(16.4455170816057,0.271734615807756,4.36891289568356));
#37577=CARTESIAN_POINT('Ctrl Pts',(16.4690115081859,0.0664083969439258,
4.41526660914191));
#37578=CARTESIAN_POINT('Ctrl Pts',(16.4766006560786,5.2409936866539E-5,
4.41519222098806));
#37579=CARTESIAN_POINT('Ctrl Pts',(16.2733993439214,0.000380345806842052,
4.41593091837313));
#37580=CARTESIAN_POINT('Ctrl Pts',(16.2858149944323,-0.107690075887363,
4.41492720978183));
#37581=CARTESIAN_POINT('Ctrl Pts',(16.3141359236307,-0.35582464097624,4.31660057631701));
#37582=CARTESIAN_POINT('Ctrl Pts',(16.3583621315169,-0.481170314810987,
3.89811598262401));
#37583=CARTESIAN_POINT('Ctrl Pts',(16.4060779675797,-0.174540169679895,
3.54017290856226));
#37584=CARTESIAN_POINT('Ctrl Pts',(16.4537938036425,0.292372898913969,3.60449612791703));
#37585=CARTESIAN_POINT('Ctrl Pts',(16.5015096397054,0.490795435699827,4.0320166386149));
#37586=CARTESIAN_POINT('Ctrl Pts',(16.5413781531317,0.280003220364278,4.36466130212541));
#37587=CARTESIAN_POINT('Ctrl Pts',(16.5653413878703,0.0704421061260754,
4.4151638399628));
#37588=CARTESIAN_POINT('Ctrl Pts',(16.5733993439214,-1.52272386678906E-5,
4.41518677123726));
#37589=CARTESIAN_POINT('Origin',(3.42660065607856,0.,4.));
#37590=CARTESIAN_POINT('',(15.8766006560786,-0.00023258108979477,4.41639972388928));
#37591=CARTESIAN_POINT('',(15.9733993439214,-0.000169011902647176,4.4164782780785));
#37592=CARTESIAN_POINT('',(3.42660065607856,4.87367679877478E-13,4.415875));
#37593=CARTESIAN_POINT('Ctrl Pts',(15.8766006560786,-0.000232581089794846,
4.41639972388928));
#37594=CARTESIAN_POINT('Ctrl Pts',(15.8781481639346,-0.0136633580705269,
4.41648966084242));
#37595=CARTESIAN_POINT('Ctrl Pts',(15.8956009504782,-0.165044849757219,
4.40979870506104));
#37596=CARTESIAN_POINT('Ctrl Pts',(15.9289590157095,-0.437567097060412,
4.22458909239344));
#37597=CARTESIAN_POINT('Ctrl Pts',(15.9766748517724,-0.425562075928853,
3.75341909160864));
#37598=CARTESIAN_POINT('Ctrl Pts',(16.0243906878352,-0.0227568523576073,
3.50868813313462));
#37599=CARTESIAN_POINT('Ctrl Pts',(16.072106523898,0.400946338892803,3.71513642180785));
#37600=CARTESIAN_POINT('Ctrl Pts',(16.1198223599609,0.456454337785543,4.1831793175245));
#37601=CARTESIAN_POINT('Ctrl Pts',(16.1546537373544,0.190990792023167,4.40204523666471));
#37602=CARTESIAN_POINT('Ctrl Pts',(16.1735798360603,0.0266382990664043,
4.41629648110721));
#37603=CARTESIAN_POINT('Ctrl Pts',(16.1766006560786,0.000364146841390366,
4.41605523138122));
#37604=CARTESIAN_POINT('Ctrl Pts',(15.9733993439214,-0.000169011902647174,
4.4164782780785));
#37605=CARTESIAN_POINT('Ctrl Pts',(15.974478043619,-0.00952634975615679,
4.4165263696097));
#37606=CARTESIAN_POINT('Ctrl Pts',(15.9914620220042,-0.156808910032117,
4.4119928338179));
#37607=CARTESIAN_POINT('Ctrl Pts',(16.024351279077,-0.430762722000766,4.23737881579128));
#37608=CARTESIAN_POINT('Ctrl Pts',(16.0720671151398,-0.432639725453012,
3.76605963834362));
#37609=CARTESIAN_POINT('Ctrl Pts',(16.1197829512026,-0.0372170120039125,
3.50957149464017));
#37610=CARTESIAN_POINT('Ctrl Pts',(16.1674987872655,0.392382656225717,3.70345139362117));
#37611=CARTESIAN_POINT('Ctrl Pts',(16.2152146233283,0.461651293660056,4.16965644082667));
#37612=CARTESIAN_POINT('Ctrl Pts',(16.2505148088803,0.199264245432362,4.39929555075695));
#37613=CARTESIAN_POINT('Ctrl Pts',(16.2699097157447,0.0307553622657438,
4.41621302761729));
#37614=CARTESIAN_POINT('Ctrl Pts',(16.2733993439214,0.000380345806842052,
4.41593091837313));
#37615=CARTESIAN_POINT('Origin',(3.42660065607856,0.,4.));
#37616=CARTESIAN_POINT('',(15.5766006560786,-0.000245472137683418,4.41533389801214));
#37617=CARTESIAN_POINT('',(15.6733993439214,-0.00029394562308721,4.41541483535501));
#37618=CARTESIAN_POINT('',(3.42660065607856,4.87367679877478E-13,4.415875));
#37619=CARTESIAN_POINT('Ctrl Pts',(15.5766006560786,-0.000245472137683396,
4.41533389801214));
#37620=CARTESIAN_POINT('Ctrl Pts',(15.5827164918089,-0.0536739331835165,
4.41562024719655));
#37621=CARTESIAN_POINT('Ctrl Pts',(15.6047376062269,-0.245697356182912,
4.38119912149661));
#37622=CARTESIAN_POINT('Ctrl Pts',(15.6426639993325,-0.483248643997369,
4.09152034160055));
#37623=CARTESIAN_POINT('Ctrl Pts',(15.6903798353953,-0.338341267922855,
3.64302603558196));
#37624=CARTESIAN_POINT('Ctrl Pts',(15.7380956714582,0.117270100534806,3.52234641383892));
#37625=CARTESIAN_POINT('Ctrl Pts',(15.785811507521,0.465190531238913,3.84030342991275));
#37626=CARTESIAN_POINT('Ctrl Pts',(15.8319798357278,0.388490242362186,4.28984418805176));
#37627=CARTESIAN_POINT('Ctrl Pts',(15.862242885247,0.124378106492246,4.41556528924811));
#37628=CARTESIAN_POINT('Ctrl Pts',(15.8766006560786,-0.000232581089794846,
4.41639972388928));
#37629=CARTESIAN_POINT('Ctrl Pts',(15.6733993439214,-0.000293945623087231,
4.41541483535501));
#37630=CARTESIAN_POINT('Ctrl Pts',(15.6790463714933,-0.0496027558454661,
4.41573527017753));
#37631=CARTESIAN_POINT('Ctrl Pts',(15.7005986777528,-0.23740431922453,4.38477730872224));
#37632=CARTESIAN_POINT('Ctrl Pts',(15.7380562626999,-0.480343569999647,
4.1057131950703));
#37633=CARTESIAN_POINT('Ctrl Pts',(15.7857720987628,-0.348708030819167,
3.6531456586776));
#37634=CARTESIAN_POINT('Ctrl Pts',(15.8334879348256,0.103151458625294,3.5190998009613));
#37635=CARTESIAN_POINT('Ctrl Pts',(15.8812037708885,0.460285376424935,3.82667199562295));
#37636=CARTESIAN_POINT('Ctrl Pts',(15.9278409072537,0.396214095655672,4.28286244744368));
#37637=CARTESIAN_POINT('Ctrl Pts',(15.9585727649314,0.128446309981357,4.41581726659612));
#37638=CARTESIAN_POINT('Ctrl Pts',(15.9733993439214,-0.000169011902647174,
4.4164782780785));
#37639=CARTESIAN_POINT('Origin',(3.42660065607856,0.,4.));
#37640=CARTESIAN_POINT('',(15.2766006560786,0.000330084823988869,4.41550084660604));
#37641=CARTESIAN_POINT('',(15.3733993439214,0.000289868078815952,4.41540680128743));
#37642=CARTESIAN_POINT('',(3.42660065607856,4.87367679877478E-13,4.415875));
#37643=CARTESIAN_POINT('Ctrl Pts',(15.2766006560786,0.000330084823988861,
4.41550084660604));
#37644=CARTESIAN_POINT('Ctrl Pts',(15.2872848196833,-0.0929135079625664,
4.41481081573461));
#37645=CARTESIAN_POINT('Ctrl Pts',(15.3138742619755,-0.32600240339937,4.33760928826424));
#37646=CARTESIAN_POINT('Ctrl Pts',(15.3563689829555,-0.489387968817152,
3.95096286275689));
#37647=CARTESIAN_POINT('Ctrl Pts',(15.4040848190183,-0.223435404337718,
3.56184267101825));
#37648=CARTESIAN_POINT('Ctrl Pts',(15.4518006550811,0.24770132994065,3.57508909640066));
#37649=CARTESIAN_POINT('Ctrl Pts',(15.499516491144,0.491370121559653,3.97853774265298));
#37650=CARTESIAN_POINT('Ctrl Pts',(15.5411164914764,0.310410063586636,4.3474585185963));
#37651=CARTESIAN_POINT('Ctrl Pts',(15.5668112131213,0.0852759340546689,
4.41487554708019));
#37652=CARTESIAN_POINT('Ctrl Pts',(15.5766006560786,-0.000245472137683396,
4.41533389801214));
#37653=CARTESIAN_POINT('Ctrl Pts',(15.3733993439214,0.000289868078815973,
4.41540680128743));
#37654=CARTESIAN_POINT('Ctrl Pts',(15.3836146993676,-0.0889130762729256,
4.41483587894927));
#37655=CARTESIAN_POINT('Ctrl Pts',(15.4097353335015,-0.317845114095608,
4.34285359523591));
#37656=CARTESIAN_POINT('Ctrl Pts',(15.4517612463229,-0.490619905976795,
3.96539750426199));
#37657=CARTESIAN_POINT('Ctrl Pts',(15.4994770823858,-0.236243011612202,
3.56861332390027));
#37658=CARTESIAN_POINT('Ctrl Pts',(15.5471929184486,0.235079475381852,3.56797816593814));
#37659=CARTESIAN_POINT('Ctrl Pts',(15.5949087545115,0.490524862970081,3.9640753057054));
#37660=CARTESIAN_POINT('Ctrl Pts',(15.6369775630024,0.318592711010818,4.34238143198936));
#37661=CARTESIAN_POINT('Ctrl Pts',(15.6631410928057,0.0892792238074376,
4.41483274135358));
#37662=CARTESIAN_POINT('Ctrl Pts',(15.6733993439214,-0.000293945623087231,
4.41541483535501));
#37663=CARTESIAN_POINT('Origin',(3.42660065607856,0.,4.));
#37664=CARTESIAN_POINT('',(14.9766006560786,0.000104941934236194,4.41652945172571));
#37665=CARTESIAN_POINT('',(15.0733993439214,0.000175165248676303,4.41647198785975));
#37666=CARTESIAN_POINT('',(3.42660065607856,4.87367679877478E-13,4.415875));
#37667=CARTESIAN_POINT('Ctrl Pts',(14.9766006560786,0.000104941934236227,
4.41652945172572));
#37668=CARTESIAN_POINT('Ctrl Pts',(14.9918531475576,-0.132161740438444,
4.41608294134065));
#37669=CARTESIAN_POINT('Ctrl Pts',(15.0230109177242,-0.40316752945992,4.27633971254324));
#37670=CARTESIAN_POINT('Ctrl Pts',(15.0700739665785,-0.455482716161518,
3.8144178884426));
#37671=CARTESIAN_POINT('Ctrl Pts',(15.1177898026413,-0.0902467530057116,
3.51651189422706));
#37672=CARTESIAN_POINT('Ctrl Pts',(15.1655056387041,0.357864192060027,3.66260046696357));
#37673=CARTESIAN_POINT('Ctrl Pts',(15.2132214747669,0.47734294310866,4.11852822244656));
#37674=CARTESIAN_POINT('Ctrl Pts',(15.2502531472251,0.229869832763757,4.3878938710325));
#37675=CARTESIAN_POINT('Ctrl Pts',(15.2713795409956,0.0458961718568525,
4.41583804947224));
#37676=CARTESIAN_POINT('Ctrl Pts',(15.2766006560786,0.000330084823988861,
4.41550084660604));
#37677=CARTESIAN_POINT('Ctrl Pts',(15.0733993439214,0.000175165248676341,
4.41647198785975));
#37678=CARTESIAN_POINT('Ctrl Pts',(15.0881830272419,-0.128073190246274,
4.41579247653651));
#37679=CARTESIAN_POINT('Ctrl Pts',(15.1188719892501,-0.395510344386944,
4.28350986851547));
#37680=CARTESIAN_POINT('Ctrl Pts',(15.1654662299459,-0.46075086019608,3.82791319143947));
#37681=CARTESIAN_POINT('Ctrl Pts',(15.2131820660087,-0.104447211543591,
3.51937956259357));
#37682=CARTESIAN_POINT('Ctrl Pts',(15.2608979020716,0.347771918596306,3.652207076714));
#37683=CARTESIAN_POINT('Ctrl Pts',(15.3086137381344,0.480626744730421,4.10441818376995));
#37684=CARTESIAN_POINT('Ctrl Pts',(15.346114218751,0.238163166260598,4.38445638366753));
#37685=CARTESIAN_POINT('Ctrl Pts',(15.36770942068,0.0499756483669043,4.41572480336754));
#37686=CARTESIAN_POINT('Ctrl Pts',(15.3733993439214,0.000289868078815973,
4.41540680128743));
#37687=CARTESIAN_POINT('Origin',(3.42660065607856,0.,4.));
#37688=CARTESIAN_POINT('',(14.6766006560786,-0.000383732061438463,4.41581798673635));
#37689=CARTESIAN_POINT('',(14.7733993439214,-0.000379407362125217,4.41594234696178));
#37690=CARTESIAN_POINT('',(3.42660065607856,4.87367679877478E-13,4.415875));
#37691=CARTESIAN_POINT('Ctrl Pts',(14.6766006560786,-0.000383732061438387,
4.41581798673635));
#37692=CARTESIAN_POINT('Ctrl Pts',(14.6805161967443,-0.0344897130604965,
4.41612948839573));
#37693=CARTESIAN_POINT('Ctrl Pts',(14.7003370160976,-0.206786574235377,
4.39667515056147));
#37694=CARTESIAN_POINT('Ctrl Pts',(14.7360631141386,-0.466025611307368,
4.15724297904063));
#37695=CARTESIAN_POINT('Ctrl Pts',(14.7837789502014,-0.38430721152129,3.69305832471834));
#37696=CARTESIAN_POINT('Ctrl Pts',(14.8314947862642,0.0503264139313189,
3.51074293371195));
#37697=CARTESIAN_POINT('Ctrl Pts',(14.8792106223271,0.438744519099385,3.77771983486548));
#37698=CARTESIAN_POINT('Ctrl Pts',(14.9269264583899,0.42425678142631,4.24882003188202));
#37699=CARTESIAN_POINT('Ctrl Pts',(14.9593898029737,0.149335702075518,4.41387566524124));
#37700=CARTESIAN_POINT('Ctrl Pts',(14.97594786887,0.00576578747519492,4.41654856180149));
#37701=CARTESIAN_POINT('Ctrl Pts',(14.9766006560786,0.000104941934236227,
4.41652945172572));
#37702=CARTESIAN_POINT('Ctrl Pts',(14.7733993439214,-0.000379407362125234,
4.41594234696178));
#37703=CARTESIAN_POINT('Ctrl Pts',(14.7768460764287,-0.0303789312965351,
4.41622104989506));
#37704=CARTESIAN_POINT('Ctrl Pts',(14.7961980876235,-0.198506931257387,
4.39955296987463));
#37705=CARTESIAN_POINT('Ctrl Pts',(14.831455377506,-0.461192356972643,4.17090007232882));
#37706=CARTESIAN_POINT('Ctrl Pts',(14.8791712135689,-0.393180492164677,
3.7045100248179));
#37707=CARTESIAN_POINT('Ctrl Pts',(14.9268870496317,0.0358950684576197,
3.50947296821438));
#37708=CARTESIAN_POINT('Ctrl Pts',(14.9746028856945,0.432007635398663,3.76489443262817));
#37709=CARTESIAN_POINT('Ctrl Pts',(15.0223187217574,0.431400943461215,4.23621695712364));
#37710=CARTESIAN_POINT('Ctrl Pts',(15.0552508744997,0.157562060208247,4.41179740605063));
#37711=CARTESIAN_POINT('Ctrl Pts',(15.0722777485543,0.00990499767517082,
4.41652354042182));
#37712=CARTESIAN_POINT('Ctrl Pts',(15.0733993439214,0.000175165248676341,
4.41647198785975));
#37713=CARTESIAN_POINT('Origin',(3.42660065607856,0.,4.));
#37714=CARTESIAN_POINT('',(14.3766006560786,7.63317591858645E-5,4.41519896243726));
#37715=CARTESIAN_POINT('',(14.4733993439214,9.02664646690309E-6,4.41518644689786));
#37716=CARTESIAN_POINT('',(3.42660065607856,4.87367679877478E-13,4.415875));
#37717=CARTESIAN_POINT('Ctrl Pts',(14.3766006560786,7.63317591858798E-5,
4.41519896243726));
#37718=CARTESIAN_POINT('Ctrl Pts',(14.3850845246186,-0.0740996743586071,
4.41507773880187));
#37719=CARTESIAN_POINT('Ctrl Pts',(14.4094736718463,-0.287504468978829,
4.360651101065));
#37720=CARTESIAN_POINT('Ctrl Pts',(14.4497680977616,-0.491476396904638,
4.01887262932433));
#37721=CARTESIAN_POINT('Ctrl Pts',(14.4974839338244,-0.281685449746218,
3.59681451879656));
#37722=CARTESIAN_POINT('Ctrl Pts',(14.5451997698872,0.186781580201919,3.54500783946397));
#37723=CARTESIAN_POINT('Ctrl Pts',(14.59291560595,0.483724211046603,3.91102746210588));
#37724=CARTESIAN_POINT('Ctrl Pts',(14.6367159013472,0.348540265561382,4.32201186060262));
#37725=CARTESIAN_POINT('Ctrl Pts',(14.6646109180567,0.104051852208848,4.41486414061182));
#37726=CARTESIAN_POINT('Ctrl Pts',(14.6766006560786,-0.000383732061438387,
4.41581798673635));
#37727=CARTESIAN_POINT('Ctrl Pts',(14.4733993439214,9.0266464668684E-6,
4.41518644689786));
#37728=CARTESIAN_POINT('Ctrl Pts',(14.481414404303,-0.0700733710850898,
4.41517292627706));
#37729=CARTESIAN_POINT('Ctrl Pts',(14.5053347433722,-0.279247125311621,
4.3650573561381));
#37730=CARTESIAN_POINT('Ctrl Pts',(14.545160361129,-0.490707361486496,4.03333931965322));
#37731=CARTESIAN_POINT('Ctrl Pts',(14.5928761971918,-0.293437803431633,
3.60528557111603));
#37732=CARTESIAN_POINT('Ctrl Pts',(14.6405920332547,0.173300204635467,3.53970415608515));
#37733=CARTESIAN_POINT('Ctrl Pts',(14.6883078693175,0.480893968219416,3.89681949708321));
#37734=CARTESIAN_POINT('Ctrl Pts',(14.7325769728731,0.356556173733762,4.31604662460621));
#37735=CARTESIAN_POINT('Ctrl Pts',(14.760940797741,0.10805675748006,4.41493494840171));
#37736=CARTESIAN_POINT('Ctrl Pts',(14.7733993439214,-0.000379407362125234,
4.41594234696178));
#37737=CARTESIAN_POINT('Origin',(3.42660065607856,0.,4.));
#37738=CARTESIAN_POINT('',(14.0766006560786,0.000355193352615291,4.41609897421413));
#37739=CARTESIAN_POINT('',(14.1733993439214,0.000376051973931104,4.41597558743442));
#37740=CARTESIAN_POINT('',(3.42660065607856,4.87367679877478E-13,4.415875));
#37741=CARTESIAN_POINT('Ctrl Pts',(14.0766006560786,0.000355193352615277,
4.41609897421413));
#37742=CARTESIAN_POINT('Ctrl Pts',(14.0896528524929,-0.113137957382804,
4.41506966208575));
#37743=CARTESIAN_POINT('Ctrl Pts',(14.1186103275949,-0.366637448157006,
4.30821039815648));
#37744=CARTESIAN_POINT('Ctrl Pts',(14.1634730813845,-0.476711717661702,
3.87895801102093));
#37745=CARTESIAN_POINT('Ctrl Pts',(14.2111889174473,-0.156014541823709,
3.53356170012368));
#37746=CARTESIAN_POINT('Ctrl Pts',(14.2589047535102,0.307953188363286,3.61650285707861));
#37747=CARTESIAN_POINT('Ctrl Pts',(14.306620589573,0.4891227672074,4.05161534124029));
#37748=CARTESIAN_POINT('Ctrl Pts',(14.3458525570958,0.268773633406098,4.37039329245586));
#37749=CARTESIAN_POINT('Ctrl Pts',(14.369179245931,0.0649630708582953,4.4153050049005));
#37750=CARTESIAN_POINT('Ctrl Pts',(14.3766006560786,7.63317591858798E-5,
4.41519896243726));
#37751=CARTESIAN_POINT('Ctrl Pts',(14.1733993439214,0.000376051973931098,
4.41597558743442));
#37752=CARTESIAN_POINT('Ctrl Pts',(14.1859827321773,-0.109124255432428,
4.41495896305428));
#37753=CARTESIAN_POINT('Ctrl Pts',(14.2144713991208,-0.358682910161539,
4.31442504752535));
#37754=CARTESIAN_POINT('Ctrl Pts',(14.258865344752,-0.480069828122688,3.8930505494253));
#37755=CARTESIAN_POINT('Ctrl Pts',(14.3065811808148,-0.169684322438749,
3.53835895376334));
#37756=CARTESIAN_POINT('Ctrl Pts',(14.3542970168777,0.296524907469595,3.60759943412104));
#37757=CARTESIAN_POINT('Ctrl Pts',(14.4020128529405,0.49043075222644,4.0371873919842));
#37758=CARTESIAN_POINT('Ctrl Pts',(14.4417136286217,0.277046036654804,4.36620192284859));
#37759=CARTESIAN_POINT('Ctrl Pts',(14.4655091256154,0.0689998253659925,
4.41519975692232));
#37760=CARTESIAN_POINT('Ctrl Pts',(14.4733993439214,9.0266464668684E-6,
4.41518644689786));
#37761=CARTESIAN_POINT('Origin',(3.42660065607856,0.,4.));
#37762=CARTESIAN_POINT('',(13.7766006560786,-0.000253139125078747,4.41636688691614));
#37763=CARTESIAN_POINT('',(13.8733993439214,-0.000192710833643805,4.4164526008213));
#37764=CARTESIAN_POINT('',(3.42660065607856,4.87367679877478E-13,4.415875));
#37765=CARTESIAN_POINT('Ctrl Pts',(13.7766006560786,-0.000253139125078718,
4.41636688691614));
#37766=CARTESIAN_POINT('Ctrl Pts',(13.7783159016796,-0.0151427949580853,
4.41647347977994));
#37767=CARTESIAN_POINT('Ctrl Pts',(13.7959364259683,-0.167994124135391,
4.40898222403799));
#37768=CARTESIAN_POINT('Ctrl Pts',(13.8294622289446,-0.439909757638992,
4.21996506537626));
#37769=CARTESIAN_POINT('Ctrl Pts',(13.8771780650075,-0.422939705734467,
3.74894775411238));
#37770=CARTESIAN_POINT('Ctrl Pts',(13.9248939010703,-0.0175776142901187,
3.50847558318244));
#37771=CARTESIAN_POINT('Ctrl Pts',(13.9726097371332,0.403926270823208,3.71937784729135));
#37772=CARTESIAN_POINT('Ctrl Pts',(14.020325573196,0.454498446235019,4.18797975215946));
#37773=CARTESIAN_POINT('Ctrl Pts',(14.0549892128445,0.188032430710383,4.40299531219535));
#37774=CARTESIAN_POINT('Ctrl Pts',(14.0737475738053,0.0251636842930195,
4.41632397176197));
#37775=CARTESIAN_POINT('Ctrl Pts',(14.0766006560786,0.000355193352615277,
4.41609897421413));
#37776=CARTESIAN_POINT('Ctrl Pts',(13.8733993439214,-0.000192710833643682,
4.4164526008213));
#37777=CARTESIAN_POINT('Ctrl Pts',(13.874645781364,-0.0110068809386406,
4.41651469495978));
#37778=CARTESIAN_POINT('Ctrl Pts',(13.8917974974943,-0.15975450351916,4.41122255187585));
#37779=CARTESIAN_POINT('Ctrl Pts',(13.9248544923121,-0.433240552373761,
4.23282579030437));
#37780=CARTESIAN_POINT('Ctrl Pts',(13.9725703283749,-0.430150181893835,
3.76151300691929));
#37781=CARTESIAN_POINT('Ctrl Pts',(14.0202861644378,-0.032046280669499,
3.50920649887429));
#37782=CARTESIAN_POINT('Ctrl Pts',(14.0680020005006,0.39548621318905,3.70760321474174));
#37783=CARTESIAN_POINT('Ctrl Pts',(14.1157178365634,0.459837632138507,4.1745123976147));
#37784=CARTESIAN_POINT('Ctrl Pts',(14.1508502843704,0.196303200904851,4.40029544879449));
#37785=CARTESIAN_POINT('Ctrl Pts',(14.1700774534897,0.0292830534939708,
4.41624396624722));
#37786=CARTESIAN_POINT('Ctrl Pts',(14.1733993439214,0.000376051973931098,
4.41597558743442));
#37787=CARTESIAN_POINT('Origin',(3.42660065607856,0.,4.));
#37788=CARTESIAN_POINT('',(13.4766006560786,-0.000226204729293368,4.4153088088013));
#37789=CARTESIAN_POINT('',(13.5733993439214,-0.000277574767750837,4.41538411867388));
#37790=CARTESIAN_POINT('',(3.42660065607856,4.87367679877478E-13,4.415875));
#37791=CARTESIAN_POINT('Ctrl Pts',(13.4766006560786,-0.000226204729293314,
4.4153088088013));
#37792=CARTESIAN_POINT('Ctrl Pts',(13.482884229554,-0.0551283395969922,
4.41557894444213));
#37793=CARTESIAN_POINT('Ctrl Pts',(13.505073081717,-0.248664136397309,4.37988069596112));
#37794=CARTESIAN_POINT('Ctrl Pts',(13.5431672125676,-0.484186345555107,
4.08642226350871));
#37795=CARTESIAN_POINT('Ctrl Pts',(13.5908830486304,-0.334560300710407,
3.63948005597396));
#37796=CARTESIAN_POINT('Ctrl Pts',(13.6385988846933,0.122297616148583,3.52360886035071));
#37797=CARTESIAN_POINT('Ctrl Pts',(13.6863147207561,0.466847750307624,3.8452149784873));
#37798=CARTESIAN_POINT('Ctrl Pts',(13.7323153112179,0.38570983934117,4.29229218593957));
#37799=CARTESIAN_POINT('Ctrl Pts',(13.762410622992,0.122927301498021,4.41548505619568));
#37800=CARTESIAN_POINT('Ctrl Pts',(13.7766006560786,-0.000253139125078718,
4.41636688691614));
#37801=CARTESIAN_POINT('Ctrl Pts',(13.5733993439214,-0.000277574767750817,
4.41538411867388));
#37802=CARTESIAN_POINT('Ctrl Pts',(13.5792141092383,-0.0510604653080308,
4.41569425641003));
#37803=CARTESIAN_POINT('Ctrl Pts',(13.6009341532429,-0.240371663949131,
4.38351498152559));
#37804=CARTESIAN_POINT('Ctrl Pts',(13.6385594759351,-0.481431012491488,
4.10064494554323));
#37805=CARTESIAN_POINT('Ctrl Pts',(13.6862753119979,-0.345033139360895,
3.64948986092447));
#37806=CARTESIAN_POINT('Ctrl Pts',(13.7339911480608,0.108213974662067,3.52021363031051));
#37807=CARTESIAN_POINT('Ctrl Pts',(13.7817069841236,0.462086530666827,3.83153260544464));
#37808=CARTESIAN_POINT('Ctrl Pts',(13.8281763827438,0.393458703070077,4.28538422885222));
#37809=CARTESIAN_POINT('Ctrl Pts',(13.8587405026764,0.126988323162951,4.4157223370415));
#37810=CARTESIAN_POINT('Ctrl Pts',(13.8733993439214,-0.000192710833643682,
4.4164526008213));
#37811=CARTESIAN_POINT('Origin',(3.42660065607856,0.,4.));
#37812=CARTESIAN_POINT('',(13.1766006560786,0.000342007958933446,4.41553758638116));
#37813=CARTESIAN_POINT('',(13.2733993439214,0.000305371599794934,4.41543889539504));
#37814=CARTESIAN_POINT('',(3.42660065607856,4.87367679877478E-13,4.415875));
#37815=CARTESIAN_POINT('Ctrl Pts',(13.1766006560786,0.000342007958933428,
4.41553758638117));
#37816=CARTESIAN_POINT('Ctrl Pts',(13.1874525574283,-0.0943443719380771,
4.41480703635833));
#37817=CARTESIAN_POINT('Ctrl Pts',(13.2142097374657,-0.328913583769224,
4.33568767983454));
#37818=CARTESIAN_POINT('Ctrl Pts',(13.2568721961906,-0.488843983144383,
3.94580788806928));
#37819=CARTESIAN_POINT('Ctrl Pts',(13.3045880322534,-0.218805220893238,
3.55951220202843));
#37820=CARTESIAN_POINT('Ctrl Pts',(13.3523038683163,0.252165742455243,3.57772323864086));
#37821=CARTESIAN_POINT('Ctrl Pts',(13.4000197043791,0.491569024438394,3.98371752277252));
#37822=CARTESIAN_POINT('Ctrl Pts',(13.4414519669665,0.307476227900318,4.34923088347422));
#37823=CARTESIAN_POINT('Ctrl Pts',(13.4669789508664,0.0838425436168888,
4.41489516431802));
#37824=CARTESIAN_POINT('Ctrl Pts',(13.4766006560786,-0.000226204729293314,
4.4153088088013));
#37825=CARTESIAN_POINT('Ctrl Pts',(13.2733993439214,0.000305371599794949,
4.41543889539504));
#37826=CARTESIAN_POINT('Ctrl Pts',(13.2837824371127,-0.0903447040275099,
4.41482455235666));
#37827=CARTESIAN_POINT('Ctrl Pts',(13.3100708089916,-0.320767143545349,
4.3409984814332));
#37828=CARTESIAN_POINT('Ctrl Pts',(13.352264459558,-0.490227979701372,3.96022874442655));
#37829=CARTESIAN_POINT('Ctrl Pts',(13.3999802956209,-0.23168347330409,3.56614749850931));
#37830=CARTESIAN_POINT('Ctrl Pts',(13.4476961316837,0.239619531536799,3.57047968038978));
#37831=CARTESIAN_POINT('Ctrl Pts',(13.4954119677466,0.490876233547033,3.96924698078795));
#37832=CARTESIAN_POINT('Ctrl Pts',(13.5373130384925,0.315668023336251,4.34421900798688));
#37833=CARTESIAN_POINT('Ctrl Pts',(13.5633088305507,0.0878472949503496,
4.41484592860038));
#37834=CARTESIAN_POINT('Ctrl Pts',(13.5733993439214,-0.000277574767750817,
4.41538411867388));
#37835=CARTESIAN_POINT('Origin',(3.42660065607856,0.,4.));
#37836=CARTESIAN_POINT('',(12.8766006560786,7.85109994957766E-5,4.41654344863055));
#37837=CARTESIAN_POINT('',(12.9733993439214,0.000150764780949702,4.41649545414489));
#37838=CARTESIAN_POINT('',(3.42660065607856,4.87367679877478E-13,4.415875));
#37839=CARTESIAN_POINT('Ctrl Pts',(12.8766006560786,7.85109994958138E-5,
4.41654344863055));
#37840=CARTESIAN_POINT('Ctrl Pts',(12.8920208853026,-0.133630732206743,
4.41619751255639));
#37841=CARTESIAN_POINT('Ctrl Pts',(12.9233463932143,-0.405888408666218,
4.27372356364211));
#37842=CARTESIAN_POINT('Ctrl Pts',(12.9705771798136,-0.453501555338242,
3.80962782724943));
#37843=CARTESIAN_POINT('Ctrl Pts',(13.0182930158764,-0.0851462219395619,
3.51558762841831));
#37844=CARTESIAN_POINT('Ctrl Pts',(13.0660088519392,0.361400197209248,3.66639076405307));
#37845=CARTESIAN_POINT('Ctrl Pts',(13.1137246880021,0.476067254403989,4.1235523942958));
#37846=CARTESIAN_POINT('Ctrl Pts',(13.1505886227152,0.226902767145371,4.38908671404106));
#37847=CARTESIAN_POINT('Ctrl Pts',(13.1715472787407,0.0444343739838573,
4.41587777975472));
#37848=CARTESIAN_POINT('Ctrl Pts',(13.1766006560786,0.000342007958933428,
4.41553758638117));
#37849=CARTESIAN_POINT('Ctrl Pts',(12.9733993439214,0.000150764780949724,
4.4164954541449));
#37850=CARTESIAN_POINT('Ctrl Pts',(12.988350764987,-0.12953330947047,4.41589144324702));
#37851=CARTESIAN_POINT('Ctrl Pts',(13.0192074647402,-0.39825874617628,4.28096832590395));
#37852=CARTESIAN_POINT('Ctrl Pts',(13.065969443181,-0.458911634846768,3.82306685936703));
#37853=CARTESIAN_POINT('Ctrl Pts',(13.1136852792439,-0.0993761143989603,
3.51830547777773));
#37854=CARTESIAN_POINT('Ctrl Pts',(13.1614011153067,0.351418020999476,3.65589158776806));
#37855=CARTESIAN_POINT('Ctrl Pts',(13.2091169513695,0.479499580452807,4.10947774749948));
#37856=CARTESIAN_POINT('Ctrl Pts',(13.2464496942411,0.235195791588524,4.38570395495548));
#37857=CARTESIAN_POINT('Ctrl Pts',(13.2678771584251,0.0485170676377186,
4.41576563003508));
#37858=CARTESIAN_POINT('Ctrl Pts',(13.2733993439214,0.000305371599794949,
4.41543889539504));
#37859=CARTESIAN_POINT('Origin',(3.42660065607856,0.,4.));
#37860=CARTESIAN_POINT('',(12.5766006560786,-0.000382134531266273,4.41577416496379));
#37861=CARTESIAN_POINT('',(12.6733993439214,-0.000382453243898073,4.41589767499446));
#37862=CARTESIAN_POINT('',(3.42660065607856,4.87367679877478E-13,4.415875));
#37863=CARTESIAN_POINT('Ctrl Pts',(12.5766006560786,-0.000382134531266193,
4.41577416496379));
#37864=CARTESIAN_POINT('Ctrl Pts',(12.5806839344893,-0.0359587315295452,
4.41609477791077));
#37865=CARTESIAN_POINT('Ctrl Pts',(12.6006724915877,-0.209750441210566,
4.39561070447123));
#37866=CARTESIAN_POINT('Ctrl Pts',(12.6365663273737,-0.4676569254097,4.15232276575852));
#37867=CARTESIAN_POINT('Ctrl Pts',(12.6842821634365,-0.381050985679211,
3.68902512775968));
#37868=CARTESIAN_POINT('Ctrl Pts',(12.7319979994994,0.0554799374235607,
3.5113004999026));
#37869=CARTESIAN_POINT('Ctrl Pts',(12.7797138355622,0.441062780321708,3.78235614259331));
#37870=CARTESIAN_POINT('Ctrl Pts',(12.8274296716251,0.421610885427219,4.2532774884218));
#37871=CARTESIAN_POINT('Ctrl Pts',(12.8597252784638,0.146394963767536,4.4145887178469));
#37872=CARTESIAN_POINT('Ctrl Pts',(12.876115606615,0.00428438860018927,
4.4165543301878));
#37873=CARTESIAN_POINT('Ctrl Pts',(12.8766006560786,7.85109994958138E-5,
4.41654344863055));
#37874=CARTESIAN_POINT('Ctrl Pts',(12.6733993439214,-0.000382453243898042,
4.41589767499447));
#37875=CARTESIAN_POINT('Ctrl Pts',(12.6770138141737,-0.0318505807336982,
4.4161892599907));
#37876=CARTESIAN_POINT('Ctrl Pts',(12.6965335631136,-0.201468625965512,
4.39853963407534));
#37877=CARTESIAN_POINT('Ctrl Pts',(12.7319585907412,-0.462967872677167,
4.16603003860975));
#37878=CARTESIAN_POINT('Ctrl Pts',(12.779674426804,-0.390044463885,3.70038267566003));
#37879=CARTESIAN_POINT('Ctrl Pts',(12.8273902628668,0.0410627776982723,
3.50987851185683));
#37880=CARTESIAN_POINT('Ctrl Pts',(12.8751060989297,0.434461438689172,3.76946045210395));
#37881=CARTESIAN_POINT('Ctrl Pts',(12.9228219349925,0.42888747548329,4.24075040649094));
#37882=CARTESIAN_POINT('Ctrl Pts',(12.9555863499897,0.154617472482897,4.41255553662561));
#37883=CARTESIAN_POINT('Ctrl Pts',(12.9724454862994,0.00842423538524961,
4.41653398830136));
#37884=CARTESIAN_POINT('Ctrl Pts',(12.9733993439214,0.000150764780949724,
4.4164954541449));
#37885=CARTESIAN_POINT('Origin',(3.42660065607856,0.,4.));
#37886=CARTESIAN_POINT('',(12.2766006560786,9.99581421417901E-5,4.41520820259509));
#37887=CARTESIAN_POINT('',(12.3733993439214,3.32456539758885E-5,4.41518865831861));
#37888=CARTESIAN_POINT('',(3.42660065607856,4.87367679877478E-13,4.415875));
#37889=CARTESIAN_POINT('Ctrl Pts',(12.2766006560786,9.99581421418094E-5,
4.41520820259509));
#37890=CARTESIAN_POINT('Ctrl Pts',(12.2852522623637,-0.0755384113923865,
4.41504611816934));
#37891=CARTESIAN_POINT('Ctrl Pts',(12.3098091473364,-0.290455378639464,
4.35903266527152));
#37892=CARTESIAN_POINT('Ctrl Pts',(12.3502713109967,-0.49164800158875,4.0136918729824));
#37893=CARTESIAN_POINT('Ctrl Pts',(12.3979871470595,-0.277420602272412,
3.59386820576715));
#37894=CARTESIAN_POINT('Ctrl Pts',(12.4457029831224,0.191566404775332,3.54700161433684));
#37895=CARTESIAN_POINT('Ctrl Pts',(12.4934188191852,0.484635034689867,3.91613041073711));
#37896=CARTESIAN_POINT('Ctrl Pts',(12.5370513768373,0.345661459897227,4.32409890635003));
#37897=CARTESIAN_POINT('Ctrl Pts',(12.5647786558017,0.102620036091023,4.41484591908716));
#37898=CARTESIAN_POINT('Ctrl Pts',(12.5766006560786,-0.000382134531266193,
4.41577416496379));
#37899=CARTESIAN_POINT('Ctrl Pts',(12.3733993439214,3.32456539758746E-5,
4.41518865831861));
#37900=CARTESIAN_POINT('Ctrl Pts',(12.381582142048,-0.071514873974996,4.41513780400291));
#37901=CARTESIAN_POINT('Ctrl Pts',(12.4056702188623,-0.282203129244181,
4.36350051499509));
#37902=CARTESIAN_POINT('Ctrl Pts',(12.4456635743641,-0.491031474462283,
4.0281658647901));
#37903=CARTESIAN_POINT('Ctrl Pts',(12.493379410427,-0.289261580343189,3.60221492864948));
#37904=CARTESIAN_POINT('Ctrl Pts',(12.5410952464898,0.178141673866572,3.54155614424011));
#37905=CARTESIAN_POINT('Ctrl Pts',(12.5888110825527,0.481954687902679,3.90189340664049));
#37906=CARTESIAN_POINT('Ctrl Pts',(12.6329124483632,0.353693368040787,4.31820342736526));
#37907=CARTESIAN_POINT('Ctrl Pts',(12.6611085354861,0.106623193447456,4.41490615616012));
#37908=CARTESIAN_POINT('Ctrl Pts',(12.6733993439214,-0.000382453243898042,
4.41589767499447));
#37909=CARTESIAN_POINT('Origin',(3.42660065607856,0.,4.));
#37910=CARTESIAN_POINT('',(11.9766006560786,0.000344603143201134,4.41614202049347));
#37911=CARTESIAN_POINT('',(12.0733993439214,0.00037008249145147,4.41602009379307));
#37912=CARTESIAN_POINT('',(3.42660065607856,4.87367679877478E-13,4.415875));
#37913=CARTESIAN_POINT('Ctrl Pts',(11.9766006560786,0.000344603143201134,
4.41614202049347));
#37914=CARTESIAN_POINT('Ctrl Pts',(11.989820590238,-0.114576335025177,4.41511745277426));
#37915=CARTESIAN_POINT('Ctrl Pts',(12.018945803085,-0.369470719226983,4.30593844396252));
#37916=CARTESIAN_POINT('Ctrl Pts',(12.0639762946196,-0.475409571231627,
3.87394063131468));
#37917=CARTESIAN_POINT('Ctrl Pts',(12.1116921306825,-0.151090047408964,
3.53194335553704));
#37918=CARTESIAN_POINT('Ctrl Pts',(12.1594079667453,0.311977791768556,3.61976969834691));
#37919=CARTESIAN_POINT('Ctrl Pts',(12.2071238028081,0.488551624369653,4.05676737776005));
#37920=CARTESIAN_POINT('Ctrl Pts',(12.2461880325859,0.265811525316043,4.37185240566124));
#37921=CARTESIAN_POINT('Ctrl Pts',(12.269346983676,0.0635166157645696,4.41534409728183));
#37922=CARTESIAN_POINT('Ctrl Pts',(12.2766006560786,9.99581421418094E-5,
4.41520820259509));
#37923=CARTESIAN_POINT('Ctrl Pts',(12.0733993439214,0.000370082491451453,
4.41602009379308));
#37924=CARTESIAN_POINT('Ctrl Pts',(12.0861504699224,-0.110559366248508,
4.41499479059613));
#37925=CARTESIAN_POINT('Ctrl Pts',(12.1148068746109,-0.361534897467509,
4.3122242613332));
#37926=CARTESIAN_POINT('Ctrl Pts',(12.1593685579871,-0.478916017555994,
3.88799699566402));
#37927=CARTESIAN_POINT('Ctrl Pts',(12.2070843940499,-0.164809627468288,
3.53659627586117));
#37928=CARTESIAN_POINT('Ctrl Pts',(12.2548002301128,0.300643979445627,3.61074632631782));
#37929=CARTESIAN_POINT('Ctrl Pts',(12.3025160661756,0.490011594032383,4.04235401475446));
#37930=CARTESIAN_POINT('Ctrl Pts',(12.3420491041118,0.274087380788525,4.36772087084377));
#37931=CARTESIAN_POINT('Ctrl Pts',(12.3656768633604,0.0675564760281007,
4.41523665186048));
#37932=CARTESIAN_POINT('Ctrl Pts',(12.3733993439214,3.32456539758746E-5,
4.41518865831861));
#37933=CARTESIAN_POINT('Origin',(3.42660065607856,0.,4.));
#37934=CARTESIAN_POINT('',(11.6766006560786,-0.000272404999166542,4.41633191892761));
#37935=CARTESIAN_POINT('',(11.7733993439214,-0.000215373091504267,4.41642415578018));
#37936=CARTESIAN_POINT('',(3.42660065607856,4.87367679877478E-13,4.415875));
#37937=CARTESIAN_POINT('Ctrl Pts',(11.6766006560786,-0.000272404999166455,
4.41633191892761));
#37938=CARTESIAN_POINT('Ctrl Pts',(11.6784836394247,-0.0166217551361539,
4.41645573239506));
#37939=CARTESIAN_POINT('Ctrl Pts',(11.6962719014584,-0.170944672110958,
4.40814899119985));
#37940=CARTESIAN_POINT('Ctrl Pts',(11.7299654421798,-0.44220355512924,4.21531660568344));
#37941=CARTESIAN_POINT('Ctrl Pts',(11.7776812782426,-0.420270357404582,
3.74450430230823));
#37942=CARTESIAN_POINT('Ctrl Pts',(11.8253971143054,-0.0123964237846327,
3.50831762943));
#37943=CARTESIAN_POINT('Ctrl Pts',(11.8731129503683,0.406861336540243,3.72365044295193));
#37944=CARTESIAN_POINT('Ctrl Pts',(11.9208287864311,0.452492071153857,4.1927593068956));
#37945=CARTESIAN_POINT('Ctrl Pts',(11.9553246883346,0.185075114683736,4.40392780377));
#37946=CARTESIAN_POINT('Ctrl Pts',(11.9739153115504,0.0236883133891,4.41635013933017));
#37947=CARTESIAN_POINT('Ctrl Pts',(11.9766006560786,0.000344603143201134,
4.41614202049347));
#37948=CARTESIAN_POINT('Ctrl Pts',(11.7733993439214,-0.000215373091504231,
4.41642415578018));
#37949=CARTESIAN_POINT('Ctrl Pts',(11.7748135191091,-0.0124870613922979,
4.41650138834433));
#37950=CARTESIAN_POINT('Ctrl Pts',(11.7921329729843,-0.162701432614141,
4.41043584391465));
#37951=CARTESIAN_POINT('Ctrl Pts',(11.8253577055472,-0.435670260442099,
4.22824690363353));
#37952=CARTESIAN_POINT('Ctrl Pts',(11.8730735416101,-0.427612859293677,
3.75699286549843));
#37953=CARTESIAN_POINT('Ctrl Pts',(11.9207893776729,-0.0268719897862959,
3.50889601812151));
#37954=CARTESIAN_POINT('Ctrl Pts',(11.9685052137357,0.398545841420554,3.71178751390968));
#37955=CARTESIAN_POINT('Ctrl Pts',(12.0162210497986,0.457972894034889,4.17934897039372));
#37956=CARTESIAN_POINT('Ctrl Pts',(12.0511857598605,0.193343073938706,4.40127740506484));
#37957=CARTESIAN_POINT('Ctrl Pts',(12.0702451912347,0.0278098881012828,
4.41627371553856));
#37958=CARTESIAN_POINT('Ctrl Pts',(12.0733993439214,0.000370082491451453,
4.41602009379308));
#37959=CARTESIAN_POINT('Origin',(3.42660065607856,0.,4.));
#37960=CARTESIAN_POINT('',(11.3766006560786,-0.000206048103233091,4.41528588740701));
#37961=CARTESIAN_POINT('',(11.4733993439214,-0.000260100423148973,4.41535533657191));
#37962=CARTESIAN_POINT('',(3.42660065607856,4.87367679877478E-13,4.415875));
#37963=CARTESIAN_POINT('Ctrl Pts',(11.3766006560786,-0.000206048103232999,
4.41528588740701));
#37964=CARTESIAN_POINT('Ctrl Pts',(11.383051967299,-0.0565815589273492,
4.41553770218085));
#37965=CARTESIAN_POINT('Ctrl Pts',(11.4054085572071,-0.251630532720247,
4.37854193442951));
#37966=CARTESIAN_POINT('Ctrl Pts',(11.4436704258028,-0.485070265991237,
4.08131458604192));
#37967=CARTESIAN_POINT('Ctrl Pts',(11.4913862618656,-0.330742172127369,
3.63597412121053));
#37968=CARTESIAN_POINT('Ctrl Pts',(11.5391020979284,0.127311547523522,3.52492422212962));
#37969=CARTESIAN_POINT('Ctrl Pts',(11.5868179339912,0.468453114143607,3.85014371984754));
#37970=CARTESIAN_POINT('Ctrl Pts',(11.632650786708,0.382920955827079,4.29471395365306));
#37971=CARTESIAN_POINT('Ctrl Pts',(11.6625783607371,0.121478760105588,4.41540989855421));
#37972=CARTESIAN_POINT('Ctrl Pts',(11.6766006560786,-0.000272404999166455,
4.41633191892761));
#37973=CARTESIAN_POINT('Ctrl Pts',(11.4733993439214,-0.000260100423148869,
4.41535533657191));
#37974=CARTESIAN_POINT('Ctrl Pts',(11.4793818469834,-0.0525169974224216,
4.41565306322741));
#37975=CARTESIAN_POINT('Ctrl Pts',(11.501269628733,-0.243338890257842,4.3822327073369));
#37976=CARTESIAN_POINT('Ctrl Pts',(11.5390626891702,-0.482464979911041,
4.09556551685319));
#37977=CARTESIAN_POINT('Ctrl Pts',(11.586778525233,-0.341319923258817,3.64587299617429));
#37978=CARTESIAN_POINT('Ctrl Pts',(11.6344943612959,0.113264470804062,3.5213807520529));
#37979=CARTESIAN_POINT('Ctrl Pts',(11.6822101973587,0.463836358529674,3.83641192782507));
#37980=CARTESIAN_POINT('Ctrl Pts',(11.7285118582339,0.390694138047139,4.28787953265104));
#37981=CARTESIAN_POINT('Ctrl Pts',(11.7589082404215,0.125533053862222,4.41563275094549));
#37982=CARTESIAN_POINT('Ctrl Pts',(11.7733993439214,-0.000215373091504231,
4.41642415578018));
#37983=CARTESIAN_POINT('Origin',(3.42660065607856,0.,4.));
#37984=CARTESIAN_POINT('',(11.0766006560786,0.000352537510456688,4.41557576695298));
#37985=CARTESIAN_POINT('',(11.1733993439214,0.000319650745578964,4.41547275084625));
#37986=CARTESIAN_POINT('',(3.42660065607856,4.87367679877478E-13,4.415875));
#37987=CARTESIAN_POINT('Ctrl Pts',(11.0766006560786,0.000352537510456667,
4.41557576695298));
#37988=CARTESIAN_POINT('Ctrl Pts',(11.0876202951733,-0.0957751134661499,
4.41480617263661));
#37989=CARTESIAN_POINT('Ctrl Pts',(11.1145452129557,-0.331820540820521,
4.33374203885914));
#37990=CARTESIAN_POINT('Ctrl Pts',(11.1573754094257,-0.488245699001722,
3.94065893278431));
#37991=CARTESIAN_POINT('Ctrl Pts',(11.2050912454886,-0.214150733603143,
3.55723066033293));
#37992=CARTESIAN_POINT('Ctrl Pts',(11.2528070815514,0.256602145595791,3.58040428537983));
#37993=CARTESIAN_POINT('Ctrl Pts',(11.3005229176142,0.491713326162588,3.98889911147238));
#37994=CARTESIAN_POINT('Ctrl Pts',(11.3417874424566,0.304539430122629,4.35098016691413));
#37995=CARTESIAN_POINT('Ctrl Pts',(11.3671466886114,0.0824085130402235,
4.41491686960609));
#37996=CARTESIAN_POINT('Ctrl Pts',(11.3766006560786,-0.000206048103232999,
4.41528588740701));
#37997=CARTESIAN_POINT('Ctrl Pts',(11.1733993439214,0.000319650745578978,
4.41547275084625));
#37998=CARTESIAN_POINT('Ctrl Pts',(11.1839501748577,-0.0917759901056567,
4.4148158243975));
#37999=CARTESIAN_POINT('Ctrl Pts',(11.2104062844816,-0.32368545017211,4.33911969104981));
#38000=CARTESIAN_POINT('Ctrl Pts',(11.2527676727932,-0.489781601228288,
3.95506440219344));
#38001=CARTESIAN_POINT('Ctrl Pts',(11.300483508856,-0.227098200695192,3.56372986339542));
#38002=CARTESIAN_POINT('Ctrl Pts',(11.3481993449188,0.244132971891272,3.57302890392028));
#38003=CARTESIAN_POINT('Ctrl Pts',(11.3959151809817,0.491173079921361,3.97442207176994));
#38004=CARTESIAN_POINT('Ctrl Pts',(11.4376485139825,0.312739912806573,4.34603313379779));
#38005=CARTESIAN_POINT('Ctrl Pts',(11.4634765682958,0.0864149014017155,
4.41486151738456));
#38006=CARTESIAN_POINT('Ctrl Pts',(11.4733993439214,-0.000260100423148869,
4.41535533657191));
#38007=CARTESIAN_POINT('Origin',(3.42660065607856,0.,4.));
#38008=CARTESIAN_POINT('',(10.7766006560786,5.16128798610187E-5,4.41655360457584));
#38009=CARTESIAN_POINT('',(10.8733993439214,0.000125523266313186,4.41651574507477));
#38010=CARTESIAN_POINT('',(3.42660065607856,4.87367679877478E-13,4.415875));
#38011=CARTESIAN_POINT('Ctrl Pts',(10.7766006560786,5.16128798610299E-5,
4.41655360457584));
#38012=CARTESIAN_POINT('Ctrl Pts',(10.7921886230477,-0.135103241057852,
4.41631783152902));
#38013=CARTESIAN_POINT('Ctrl Pts',(10.8236818687044,-0.408598944994929,
4.27108057505162));
#38014=CARTESIAN_POINT('Ctrl Pts',(10.8710803930487,-0.451470021714238,
3.80485891169382));
#38015=CARTESIAN_POINT('Ctrl Pts',(10.9187962291115,-0.080036233235122,
3.51471716883706));
#38016=CARTESIAN_POINT('Ctrl Pts',(10.9665120651743,0.364896059739551,3.6702181168734));
#38017=CARTESIAN_POINT('Ctrl Pts',(11.0142279012372,0.47473868640782,4.1285628425314));
#38018=CARTESIAN_POINT('Ctrl Pts',(11.0509240982053,0.223935965514619,4.3902602363912));
#38019=CARTESIAN_POINT('Ctrl Pts',(11.0717150164857,0.0429714521173939,
4.4159169723618));
#38020=CARTESIAN_POINT('Ctrl Pts',(11.0766006560786,0.000352537510456667,
4.41557576695298));
#38021=CARTESIAN_POINT('Ctrl Pts',(10.8733993439214,0.000125523266313226,
4.41651574507477));
#38022=CARTESIAN_POINT('Ctrl Pts',(10.888518502732,-0.130996444363694,4.41599591363288));
#38023=CARTESIAN_POINT('Ctrl Pts',(10.9195429402303,-0.400997532511054,
4.27840016053723));
#38024=CARTESIAN_POINT('Ctrl Pts',(10.9664726564161,-0.45702143577077,3.81824018018824));
#38025=CARTESIAN_POINT('Ctrl Pts',(11.014188492479,-0.0942939790271268,
3.51728489730359));
#38026=CARTESIAN_POINT('Ctrl Pts',(11.0619043285418,0.355025089556487,3.65961432075161));
#38027=CARTESIAN_POINT('Ctrl Pts',(11.1096201646047,0.478319155637209,4.11452515096033));
#38028=CARTESIAN_POINT('Ctrl Pts',(11.1467851697312,0.23222845252417,4.38693182090163));
#38029=CARTESIAN_POINT('Ctrl Pts',(11.1680448961701,0.0470573247768451,
4.41580613485813));
#38030=CARTESIAN_POINT('Ctrl Pts',(11.1733993439214,0.000319650745578978,
4.41547275084625));
#38031=CARTESIAN_POINT('Origin',(3.42660065607856,0.,4.));
#38032=CARTESIAN_POINT('',(10.4766006560786,-0.000378910032885682,4.4157309619862));
#38033=CARTESIAN_POINT('',(10.5733993439214,-0.000383826598418624,4.41585315377736));
#38034=CARTESIAN_POINT('',(3.42660065607856,4.87367679877478E-13,4.415875));
#38035=CARTESIAN_POINT('Ctrl Pts',(10.4766006560786,-0.000378910032885704,
4.4157309619862));
#38036=CARTESIAN_POINT('Ctrl Pts',(10.4808516722344,-0.0374267536145521,
4.41605913507464));
#38037=CARTESIAN_POINT('Ctrl Pts',(10.5010079670778,-0.212714974368116,
4.3945277200383));
#38038=CARTESIAN_POINT('Ctrl Pts',(10.5370695406088,-0.469236294399976,
4.14738563318641));
#38039=CARTESIAN_POINT('Ctrl Pts',(10.5847853766716,-0.377752434501872,
3.68502647241413));
#38040=CARTESIAN_POINT('Ctrl Pts',(10.6325012127345,0.0606272984676223,
3.51191234851464));
#38041=CARTESIAN_POINT('Ctrl Pts',(10.6802170487973,0.443332050383407,3.78701662516801));
#38042=CARTESIAN_POINT('Ctrl Pts',(10.7279328848602,0.418918158891686,4.25770681210006));
#38043=CARTESIAN_POINT('Ctrl Pts',(10.7600607539539,0.143455624352724,4.41528584951654));
#38044=CARTESIAN_POINT('Ctrl Pts',(10.7762833443601,0.00280285164340033,
4.41655840401831));
#38045=CARTESIAN_POINT('Ctrl Pts',(10.7766006560786,5.16128798610299E-5,
4.41655360457584));
#38046=CARTESIAN_POINT('Ctrl Pts',(10.5733993439214,-0.000383826598418617,
4.41585315377736));
#38047=CARTESIAN_POINT('Ctrl Pts',(10.5771815519187,-0.0333213161677604,
4.41615637378185));
#38048=CARTESIAN_POINT('Ctrl Pts',(10.5968690386037,-0.20443114816448,4.39750812937281));
#38049=CARTESIAN_POINT('Ctrl Pts',(10.6324618039763,-0.464691964107356,
4.16114156306187));
#38050=CARTESIAN_POINT('Ctrl Pts',(10.6801776400391,-0.386865111317189,
3.69628860657276));
#38051=CARTESIAN_POINT('Ctrl Pts',(10.7278934761019,0.0462259258804368,
3.51033849586834));
#38052=CARTESIAN_POINT('Ctrl Pts',(10.7756093121648,0.436866984064762,3.77405207881873));
#38053=CARTESIAN_POINT('Ctrl Pts',(10.8233251482276,0.426326368719826,4.24525711444552));
#38054=CARTESIAN_POINT('Ctrl Pts',(10.8559218254798,0.151674250044741,4.4132974389186));
#38055=CARTESIAN_POINT('Ctrl Pts',(10.8726132240444,0.00694320316194716,
4.41654277368359));
#38056=CARTESIAN_POINT('Ctrl Pts',(10.8733993439214,0.000125523266313226,
4.41651574507477));
#38057=CARTESIAN_POINT('Origin',(3.42660065607856,0.,4.));
#38058=CARTESIAN_POINT('',(10.1766006560786,0.000123197149224082,4.41521991402453));
#38059=CARTESIAN_POINT('',(10.2733993439214,5.7336166378985E-5,4.41519339896199));
#38060=CARTESIAN_POINT('',(3.42660065607856,4.87367679877478E-13,4.415875));
#38061=CARTESIAN_POINT('Ctrl Pts',(10.1766006560786,0.000123197149224097,
4.41521991402453));
#38062=CARTESIAN_POINT('Ctrl Pts',(10.1854200001087,-0.0769762270984491,
4.41501595190525));
#38063=CARTESIAN_POINT('Ctrl Pts',(10.2101446228264,-0.293404201931947,
4.35739193013711));
#38064=CARTESIAN_POINT('Ctrl Pts',(10.2507745242318,-0.491764996345908,
4.00850959581219));
#38065=CARTESIAN_POINT('Ctrl Pts',(10.2984903602946,-0.273124940234581,
3.59096700393021));
#38066=CARTESIAN_POINT('Ctrl Pts',(10.3462061963575,0.196329951061554,3.54904570612073));
#38067=CARTESIAN_POINT('Ctrl Pts',(10.3939220324203,0.485492027373267,3.92124267520431));
#38068=CARTESIAN_POINT('Ctrl Pts',(10.4373868523273,0.34277731801193,4.32616121393696));
#38069=CARTESIAN_POINT('Ctrl Pts',(10.4649463935468,0.101188639822117,4.41483126760997));
#38070=CARTESIAN_POINT('Ctrl Pts',(10.4766006560786,-0.000378910032885704,
4.4157309619862));
#38071=CARTESIAN_POINT('Ctrl Pts',(10.2733993439214,5.73361663789851E-5,
4.41519339896199));
#38072=CARTESIAN_POINT('Ctrl Pts',(10.2817498797931,-0.0729553575157724,
4.41510384014646));
#38073=CARTESIAN_POINT('Ctrl Pts',(10.3060056943524,-0.285157432566911,
4.36192175935665));
#38074=CARTESIAN_POINT('Ctrl Pts',(10.3461667875993,-0.491301045992024,
4.02298928139638));
#38075=CARTESIAN_POINT('Ctrl Pts',(10.3938826236621,-0.285053227451061,
3.599188470261));
#38076=CARTESIAN_POINT('Ctrl Pts',(10.4415984597249,0.182963355965895,3.54345905416307));
#38077=CARTESIAN_POINT('Ctrl Pts',(10.4893142957878,0.482961874346273,3.9069782134126));
#38078=CARTESIAN_POINT('Ctrl Pts',(10.5332479238533,0.35082465130295,4.32033516829581));
#38079=CARTESIAN_POINT('Ctrl Pts',(10.5612762732311,0.105190355120073,4.41488124595214));
#38080=CARTESIAN_POINT('Ctrl Pts',(10.5733993439214,-0.000383826598418617,
4.41585315377736));
#38081=CARTESIAN_POINT('Origin',(3.42660065607856,0.,4.));
#38082=CARTESIAN_POINT('',(9.87660065607859,0.000332404019580576,4.41618417038907));
#38083=CARTESIAN_POINT('',(9.9733993439214,0.000362444897862246,4.41606425076498));
#38084=CARTESIAN_POINT('',(3.42660065607856,4.87367679877478E-13,4.415875));
#38085=CARTESIAN_POINT('Ctrl Pts',(9.87660065607859,0.000332404019580564,
4.41618417038907));
#38086=CARTESIAN_POINT('Ctrl Pts',(9.88998832798303,-0.116016130490024,
4.41516972706101));
#38087=CARTESIAN_POINT('Ctrl Pts',(9.91928127857509,-0.372296869871387,
4.30364082544554));
#38088=CARTESIAN_POINT('Ctrl Pts',(9.96447950785476,-0.474054618562381,
3.8689372536849));
#38089=CARTESIAN_POINT('Ctrl Pts',(10.0121953439176,-0.146148770628728,
3.53037700046135));
#38090=CARTESIAN_POINT('Ctrl Pts',(10.0599111799804,0.315967742161179,3.62307877379278));
#38091=CARTESIAN_POINT('Ctrl Pts',(10.1076270160433,0.487926215535836,4.06191310882887));
#38092=CARTESIAN_POINT('Ctrl Pts',(10.146523508076,0.262848409674369,4.37329037489646));
#38093=CARTESIAN_POINT('Ctrl Pts',(10.1695147214211,0.062069015396409,4.41538378814543));
#38094=CARTESIAN_POINT('Ctrl Pts',(10.1766006560786,0.000123197149224097,
4.41521991402453));
#38095=CARTESIAN_POINT('Ctrl Pts',(9.9733993439214,0.000362444897862267,
4.41606425076498));
#38096=CARTESIAN_POINT('Ctrl Pts',(9.9863182076674,-0.111995531308361,4.41503480155798));
#38097=CARTESIAN_POINT('Ctrl Pts',(10.015142350101,-0.364380386131072,4.30999810797653));
#38098=CARTESIAN_POINT('Ctrl Pts',(10.0598717712222,-0.477709011270712,
3.88295588266498));
#38099=CARTESIAN_POINT('Ctrl Pts',(10.1075876072851,-0.159916626226494,
3.53488507064564));
#38100=CARTESIAN_POINT('Ctrl Pts',(10.1553034433479,0.304729657315094,3.61393645496551));
#38101=CARTESIAN_POINT('Ctrl Pts',(10.2030192794107,0.489538007675758,4.04751593304174));
#38102=CARTESIAN_POINT('Ctrl Pts',(10.2423845796019,0.271127379494919,4.3692182851415));
#38103=CARTESIAN_POINT('Ctrl Pts',(10.2658446011055,0.0661120339180705,
4.41527442296197));
#38104=CARTESIAN_POINT('Ctrl Pts',(10.2733993439214,5.73361663789851E-5,
4.41519339896199));
#38105=CARTESIAN_POINT('Origin',(3.42660065607856,0.,4.));
#38106=CARTESIAN_POINT('',(9.57660065607859,-0.000290304052950346,4.41629504206998));
#38107=CARTESIAN_POINT('',(9.6733993439214,-0.000236899196693507,4.41639317328699));
#38108=CARTESIAN_POINT('',(3.42660065607856,4.87367679877478E-13,4.415875));
#38109=CARTESIAN_POINT('Ctrl Pts',(9.57660065607859,-0.000290304052950335,
4.41629504206998));
#38110=CARTESIAN_POINT('Ctrl Pts',(9.57865137716975,-0.0181001948149981,
4.41643644713422));
#38111=CARTESIAN_POINT('Ctrl Pts',(9.59660737694851,-0.173896467062472,
4.40729888742394));
#38112=CARTESIAN_POINT('Ctrl Pts',(9.63046865541489,-0.444448234747017,
4.21064422964382));
#38113=CARTESIAN_POINT('Ctrl Pts',(9.67818449147773,-0.41755432743774,3.74008922975375));
#38114=CARTESIAN_POINT('Ctrl Pts',(9.72590032754057,-0.00721385634321597,
3.50821428942208));
#38115=CARTESIAN_POINT('Ctrl Pts',(9.77361616360341,0.40975121003073,3.72795373420991));
#38116=CARTESIAN_POINT('Ctrl Pts',(9.82133199966624,0.450435435400681,4.19751745084266));
#38117=CARTESIAN_POINT('Ctrl Pts',(9.85566016382464,0.182118884769847,4.40484283743537));
#38118=CARTESIAN_POINT('Ctrl Pts',(9.87408304929542,0.0222122246324328,
4.41637494063069));
#38119=CARTESIAN_POINT('Ctrl Pts',(9.87660065607859,0.000332404019580564,
4.41618417038907));
#38120=CARTESIAN_POINT('Ctrl Pts',(9.6733993439214,-0.00023689919669354,
4.41639317328699));
#38121=CARTESIAN_POINT('Ctrl Pts',(9.67498125685411,-0.0139668454918635,
4.4164864708936));
#38122=CARTESIAN_POINT('Ctrl Pts',(9.69246844847443,-0.165649677201134,
4.40963259460397));
#38123=CARTESIAN_POINT('Ctrl Pts',(9.72586091878235,-0.438051576325333,
4.22364266437974));
#38124=CARTESIAN_POINT('Ctrl Pts',(9.77357675484519,-0.425028039486299,
3.75249971615691));
#38125=CARTESIAN_POINT('Ctrl Pts',(9.82129259090803,-0.0216947140899849,
3.50864008686857));
#38126=CARTESIAN_POINT('Ctrl Pts',(9.86900842697087,0.401561201071248,3.7160038263529));
#38127=CARTESIAN_POINT('Ctrl Pts',(9.91672426303371,0.456057286475463,4.18416562194019));
#38128=CARTESIAN_POINT('Ctrl Pts',(9.95152123535055,0.190383912560376,4.40224154849284));
#38129=CARTESIAN_POINT('Ctrl Pts',(9.97041292897978,0.0263359008882403,
4.4163022254471));
#38130=CARTESIAN_POINT('Ctrl Pts',(9.9733993439214,0.000362444897862267,
4.41606425076498));
#38131=CARTESIAN_POINT('Origin',(3.42660065607856,0.,4.));
#38132=CARTESIAN_POINT('',(9.27660065607858,-0.000185084181660103,4.41526520375254));
#38133=CARTESIAN_POINT('',(9.37339934392141,-0.000241596553487405,4.41532857883968));
#38134=CARTESIAN_POINT('',(3.42660065607856,4.87367679877478E-13,4.415875));
#38135=CARTESIAN_POINT('Ctrl Pts',(9.27660065607858,-0.000185084181660189,
4.41526520375254));
#38136=CARTESIAN_POINT('Ctrl Pts',(9.28321970504406,-0.0580335922681754,
4.4154966095816));
#38137=CARTESIAN_POINT('Ctrl Pts',(9.30574403269715,-0.254596444523232,
4.37718269734299));
#38138=CARTESIAN_POINT('Ctrl Pts',(9.34417363903789,-0.485900307124067,
4.07619787653679));
#38139=CARTESIAN_POINT('Ctrl Pts',(9.39188947510068,-0.326887306273347,
3.63250862071426));
#38140=CARTESIAN_POINT('Ctrl Pts',(9.43960531116356,0.13231133773591,3.52629235307153));
#38141=CARTESIAN_POINT('Ctrl Pts',(9.48732114722637,0.470006444430667,3.85508910653225));
#38142=CARTESIAN_POINT('Ctrl Pts',(9.53298626219807,0.380123833963086,4.29710958399465));
#38143=CARTESIAN_POINT('Ctrl Pts',(9.56274609848214,0.120032327051623,4.41533971732329));
#38144=CARTESIAN_POINT('Ctrl Pts',(9.57660065607859,-0.000290304052950335,
4.41629504206998));
#38145=CARTESIAN_POINT('Ctrl Pts',(9.3733993439214,-0.000241596553487357,
4.41532857883968));
#38146=CARTESIAN_POINT('Ctrl Pts',(9.37954958472843,-0.0539723465869793,
4.41561177485228));
#38147=CARTESIAN_POINT('Ctrl Pts',(9.40160510422307,-0.246305905820531,
4.3809303471886));
#38148=CARTESIAN_POINT('Ctrl Pts',(9.43956590240532,-0.483445357410111,
4.09047547319903));
#38149=CARTESIAN_POINT('Ctrl Pts',(9.48728173846818,-0.337568794959357,
3.64229546617122));
#38150=CARTESIAN_POINT('Ctrl Pts',(9.53499757453099,0.118302386066128,3.5226010365501));
#38151=CARTESIAN_POINT('Ctrl Pts',(9.58271341059386,0.465534665650901,3.84130942079228));
#38152=CARTESIAN_POINT('Ctrl Pts',(9.62884733372396,0.387920650713885,4.29034844530944));
#38153=CARTESIAN_POINT('Ctrl Pts',(9.65907597816649,0.124080336294106,4.41554841393524));
#38154=CARTESIAN_POINT('Ctrl Pts',(9.6733993439214,-0.00023689919669354,
4.41639317328699));
#38155=CARTESIAN_POINT('Origin',(3.42660065607856,0.,4.));
#38156=CARTESIAN_POINT('',(8.97660065607858,0.000361621133123973,4.41561526113518));
#38157=CARTESIAN_POINT('',(9.0733993439214,0.00033264130393823,4.41550825894961));
#38158=CARTESIAN_POINT('',(3.42660065607856,4.87367679877478E-13,4.415875));
#38159=CARTESIAN_POINT('Ctrl Pts',(8.97660065607858,0.000361621133123963,
4.41561526113518));
#38160=CARTESIAN_POINT('Ctrl Pts',(8.98778803291839,-0.097205817696177,
4.41480833810253));
#38161=CARTESIAN_POINT('Ctrl Pts',(9.01488068844582,-0.334723089553266,
4.33177224018802));
#38162=CARTESIAN_POINT('Ctrl Pts',(9.05787862266083,-0.487593182843731,
3.93551656882348));
#38163=CARTESIAN_POINT('Ctrl Pts',(9.10559445872368,-0.209472459465777,
3.55499829935456));
#38164=CARTESIAN_POINT('Ctrl Pts',(9.15331029478651,0.261010046587687,3.58313193881964));
#38165=CARTESIAN_POINT('Ctrl Pts',(9.20102613084934,0.491803010703882,3.99408193320625));
#38166=CARTESIAN_POINT('Ctrl Pts',(9.24212291794672,0.301599829163518,4.35270650246492));
#38167=CARTESIAN_POINT('Ctrl Pts',(9.26731442635645,0.0809737859182142,
4.41494055172187));
#38168=CARTESIAN_POINT('Ctrl Pts',(9.27660065607858,-0.000185084181660189,
4.41526520375254));
#38169=CARTESIAN_POINT('Ctrl Pts',(9.0733993439214,0.000332641303938268,
4.41550825894961));
#38170=CARTESIAN_POINT('Ctrl Pts',(9.08411791260276,-0.093207009794584,
4.4148098083896));
#38171=CARTESIAN_POINT('Ctrl Pts',(9.11074175997173,-0.326599857706223,
4.33721709571948));
#38172=CARTESIAN_POINT('Ctrl Pts',(9.1532708860283,-0.489280820139143,3.94990505119329));
#38173=CARTESIAN_POINT('Ctrl Pts',(9.20098672209113,-0.222487703095825,
3.56136068709803));
#38174=CARTESIAN_POINT('Ctrl Pts',(9.24870255815399,0.248619295113741,3.57562555337399));
#38175=CARTESIAN_POINT('Ctrl Pts',(9.29641839421681,0.49141536912078,3.97960000382683));
#38176=CARTESIAN_POINT('Ctrl Pts',(9.33798398947263,0.309808547095179,4.34782394055348));
#38177=CARTESIAN_POINT('Ctrl Pts',(9.36364430604082,0.0849819773478622,
4.41487939515448));
#38178=CARTESIAN_POINT('Ctrl Pts',(9.3733993439214,-0.000241596553487357,
4.41532857883968));
#38179=CARTESIAN_POINT('Origin',(3.42660065607856,0.,4.));
#38180=CARTESIAN_POINT('',(8.67660065607859,2.43999233753954E-5,4.41655967853978));
#38181=CARTESIAN_POINT('',(8.77339934392141,9.9565801791445E-5,4.41653262406943));
#38182=CARTESIAN_POINT('',(3.42660065607856,4.87367679877478E-13,4.415875));
#38183=CARTESIAN_POINT('Ctrl Pts',(8.67660065607859,2.43999233753836E-5,
4.41655967853978));
#38184=CARTESIAN_POINT('Ctrl Pts',(8.69235636079272,-0.136579453435425,
4.41644398151286));
#38185=CARTESIAN_POINT('Ctrl Pts',(8.72401734419445,-0.411298873006737,
4.26841067400337));
#38186=CARTESIAN_POINT('Ctrl Pts',(8.7715836062838,-0.449388340942622,3.80011167148426));
#38187=CARTESIAN_POINT('Ctrl Pts',(8.81929944234665,-0.0749173544856965,
3.51390061216986));
#38188=CARTESIAN_POINT('Ctrl Pts',(8.86701527840948,0.368351391347115,3.67408210030036));
#38189=CARTESIAN_POINT('Ctrl Pts',(8.91473111447233,0.473357386691186,4.13355901061654));
#38190=CARTESIAN_POINT('Ctrl Pts',(8.95125957369535,0.220969504140389,4.39141457480799));
#38191=CARTESIAN_POINT('Ctrl Pts',(8.97188275423077,0.0415074238114615,
4.41595555392421));
#38192=CARTESIAN_POINT('Ctrl Pts',(8.97660065607858,0.000361621133123963,
4.41561526113518));
#38193=CARTESIAN_POINT('Ctrl Pts',(8.77339934392141,9.95658017914599E-5,
4.41653262406943));
#38194=CARTESIAN_POINT('Ctrl Pts',(8.78868624047708,-0.132462770989084,
4.416105976883));
#38195=CARTESIAN_POINT('Ctrl Pts',(8.81987841572037,-0.403726445587972,
4.27580529254432));
#38196=CARTESIAN_POINT('Ctrl Pts',(8.86697586965126,-0.455080472922433,
3.81343369002772));
#38197=CARTESIAN_POINT('Ctrl Pts',(8.91469170571412,-0.0892013699275644,
3.51631793453238));
#38198=CARTESIAN_POINT('Ctrl Pts',(8.96240754177693,0.358592723611288,3.66337486216116));
#38199=CARTESIAN_POINT('Ctrl Pts',(9.0101233778398,0.477085601399612,4.11955983351088));
#38200=CARTESIAN_POINT('Ctrl Pts',(9.04712064522126,0.229261233371815,4.38814011953822));
#38201=CARTESIAN_POINT('Ctrl Pts',(9.06821263391514,0.0455964315317218,
4.41584623882512));
#38202=CARTESIAN_POINT('Ctrl Pts',(9.0733993439214,0.000332641303938268,
4.41550825894961));
#38203=CARTESIAN_POINT('Origin',(3.42660065607856,0.,4.));
#38204=CARTESIAN_POINT('',(8.37660065607859,-0.000374086211409503,4.41568853448753));
#38205=CARTESIAN_POINT('',(8.47339934392141,-0.000383538171196851,4.41580895574666));
#38206=CARTESIAN_POINT('',(3.42660065607856,4.87367679877478E-13,4.415875));
#38207=CARTESIAN_POINT('Ctrl Pts',(8.37660065607859,-0.000374086211409545,
4.41568853448753));
#38208=CARTESIAN_POINT('Ctrl Pts',(8.38101940997943,-0.0388937529272332,
4.41602262289185));
#38209=CARTESIAN_POINT('Ctrl Pts',(8.40134344256788,-0.215680110827853,
4.3934260635833));
#38210=CARTESIAN_POINT('Ctrl Pts',(8.43757275384394,-0.470763542849379,
4.14243212971755));
#38211=CARTESIAN_POINT('Ctrl Pts',(8.48528858990678,-0.37441192437669,3.68106280283335));
#38212=CARTESIAN_POINT('Ctrl Pts',(8.53300442596962,0.0657679253190804,
3.51257841158684));
#38213=CARTESIAN_POINT('Ctrl Pts',(8.58072026203246,0.445552077224736,3.79170076492532));
#38214=CARTESIAN_POINT('Ctrl Pts',(8.62843609809529,0.41617890091499,4.26210751092856));
#38215=CARTESIAN_POINT('Ctrl Pts',(8.66039622944401,0.140517691799823,4.41596716726027));
#38216=CARTESIAN_POINT('Ctrl Pts',(8.6764510821051,0.00132122424898086,
4.41656077688887));
#38217=CARTESIAN_POINT('Ctrl Pts',(8.67660065607859,2.43999233753836E-5,
4.41655967853978));
#38218=CARTESIAN_POINT('Ctrl Pts',(8.47339934392141,-0.000383538171196768,
4.41580895574666));
#38219=CARTESIAN_POINT('Ctrl Pts',(8.47734928966379,-0.0347911067166248,
4.41612244784963));
#38220=CARTESIAN_POINT('Ctrl Pts',(8.4972045140938,-0.207394442561863,4.39645832432586));
#38221=CARTESIAN_POINT('Ctrl Pts',(8.5329650172114,-0.466364439759318,4.15623518867385));
#38222=CARTESIAN_POINT('Ctrl Pts',(8.58068085327425,-0.383642787608637,
3.69222827230584));
#38223=CARTESIAN_POINT('Ctrl Pts',(8.62839668933707,0.0513839395061145,
3.51085286915611));
#38224=CARTESIAN_POINT('Ctrl Pts',(8.67611252539993,0.439224004328866,3.77866880275638));
#38225=CARTESIAN_POINT('Ctrl Pts',(8.72382836146275,0.42371790764641,4.24973658040369));
#38226=CARTESIAN_POINT('Ctrl Pts',(8.75625730096992,0.148732406864234,4.41402322426773));
#38227=CARTESIAN_POINT('Ctrl Pts',(8.77278096178947,0.00546194790078228,
4.41654988270631));
#38228=CARTESIAN_POINT('Ctrl Pts',(8.77339934392141,9.95658017914599E-5,
4.41653262406943));
#38229=CARTESIAN_POINT('Origin',(3.42660065607856,0.,4.));
#38230=CARTESIAN_POINT('',(8.07660065607859,0.000145957947245773,4.41523406184916));
#38231=CARTESIAN_POINT('',(8.1733993439214,8.12049300508987E-5,4.41520065480005));
#38232=CARTESIAN_POINT('',(3.42660065607856,4.87367679877478E-13,4.415875));
#38233=CARTESIAN_POINT('Ctrl Pts',(8.07660065607858,0.00014595794724577,
4.41523406184916));
#38234=CARTESIAN_POINT('Ctrl Pts',(8.08558773785375,-0.0784131624224431,
4.41498734772332));
#38235=CARTESIAN_POINT('Ctrl Pts',(8.11048009831652,-0.296350794919178,
4.35572875890285));
#38236=CARTESIAN_POINT('Ctrl Pts',(8.15127773746691,-0.491827368180951,
4.00332637343646));
#38237=CARTESIAN_POINT('Ctrl Pts',(8.19899357352975,-0.268798940774433,
3.58811123553743));
#38238=CARTESIAN_POINT('Ctrl Pts',(8.24670940959259,0.201071689948468,3.55113988776764));
#38239=CARTESIAN_POINT('Ctrl Pts',(8.29442524565542,0.486295093906121,3.92636368766143));
#38240=CARTESIAN_POINT('Ctrl Pts',(8.33772232781743,0.339888039743562,4.32819890206972));
#38241=CARTESIAN_POINT('Ctrl Pts',(8.36511413129181,0.0997575609540166,
4.41482007364463));
#38242=CARTESIAN_POINT('Ctrl Pts',(8.37660065607859,-0.000374086211409545,
4.41568853448753));
#38243=CARTESIAN_POINT('Ctrl Pts',(8.1733993439214,8.12049300509751E-5,
4.41520065480005));
#38244=CARTESIAN_POINT('Ctrl Pts',(8.18191761753811,-0.0743948540356096,
4.41507113968239));
#38245=CARTESIAN_POINT('Ctrl Pts',(8.20634116984244,-0.288109900049694,
4.36032095112539));
#38246=CARTESIAN_POINT('Ctrl Pts',(8.24667000083438,-0.491516046133,4.01781014446235));
#38247=CARTESIAN_POINT('Ctrl Pts',(8.29438583689722,-0.280813212199106,
3.59620653211525));
#38248=CARTESIAN_POINT('Ctrl Pts',(8.34210167296004,0.187764715363875,3.54541267448783));
#38249=CARTESIAN_POINT('Ctrl Pts',(8.38981750902289,0.483915415676709,3.91207335260334));
#38250=CARTESIAN_POINT('Ctrl Pts',(8.43358339934334,0.347950231939931,4.32244196179047));
#38251=CARTESIAN_POINT('Ctrl Pts',(8.46144401097618,0.1037581297464,4.41486010664565));
#38252=CARTESIAN_POINT('Ctrl Pts',(8.47339934392141,-0.000383538171196768,
4.41580895574666));
#38253=CARTESIAN_POINT('Origin',(3.42660065607856,0.,4.));
#38254=CARTESIAN_POINT('',(7.77660065607858,0.000318631424802313,4.41622521972442));
#38255=CARTESIAN_POINT('',(7.8733993439214,0.000353153796088606,4.4161078667978));
#38256=CARTESIAN_POINT('',(3.42660065607856,4.87367679877478E-13,4.415875));
#38257=CARTESIAN_POINT('Ctrl Pts',(7.77660065607859,0.000318631424802297,
4.41622521972442));
#38258=CARTESIAN_POINT('Ctrl Pts',(7.79015606572807,-0.117457481003694,
4.41522659035305));
#38259=CARTESIAN_POINT('Ctrl Pts',(7.81961675406517,-0.375115671948731,
4.30131743988157));
#38260=CARTESIAN_POINT('Ctrl Pts',(7.86498272108989,-0.472647010158531,
3.86394843388276));
#38261=CARTESIAN_POINT('Ctrl Pts',(7.91269855715272,-0.141191260335066,
3.52886280888004));
#38262=CARTESIAN_POINT('Ctrl Pts',(7.96041439321556,0.31992259635559,3.62642971585976));
#38263=CARTESIAN_POINT('Ctrl Pts',(8.0081302292784,0.48724661017382,4.0670519628834));
#38264=CARTESIAN_POINT('Ctrl Pts',(8.04685898356608,0.259884401562094,4.37470733986759));
#38265=CARTESIAN_POINT('Ctrl Pts',(8.06968245916614,0.0606202562326388,
4.41542398077349));
#38266=CARTESIAN_POINT('Ctrl Pts',(8.07660065607858,0.00014595794724577,
4.41523406184916));
#38267=CARTESIAN_POINT('Ctrl Pts',(7.8733993439214,0.000353153796088627,
4.4161078667978));
#38268=CARTESIAN_POINT('Ctrl Pts',(7.88648594541244,-0.113432877329791,
4.41507910421771));
#38269=CARTESIAN_POINT('Ctrl Pts',(7.9154778255911,-0.367219156371593,4.30774647947464));
#38270=CARTESIAN_POINT('Ctrl Pts',(7.96037498445733,-0.476448943335793,
3.87792777037096));
#38271=CARTESIAN_POINT('Ctrl Pts',(8.0080908205202,-0.1550058622045,3.53322552818936));
#38272=CARTESIAN_POINT('Ctrl Pts',(8.05580665658301,0.308781487260178,3.61716946571973));
#38273=CARTESIAN_POINT('Ctrl Pts',(8.10352249264587,0.489010045760349,4.0526725734847));
#38274=CARTESIAN_POINT('Ctrl Pts',(8.14272005509199,0.26816615642074,4.37069430501912));
#38275=CARTESIAN_POINT('Ctrl Pts',(8.1660123388505,0.064666477720629,4.4153129696744));
#38276=CARTESIAN_POINT('Ctrl Pts',(8.1733993439214,8.12049300509751E-5,
4.41520065480005));
#38277=CARTESIAN_POINT('Origin',(3.42660065607856,0.,4.));
#38278=CARTESIAN_POINT('',(7.47660065607859,-0.000306770237538029,4.41625647512786));
#38279=CARTESIAN_POINT('',(7.5733993439214,-0.000257198714157858,4.41635988094829));
#38280=CARTESIAN_POINT('',(3.42660065607856,4.87367679877478E-13,4.415875));
#38281=CARTESIAN_POINT('Ctrl Pts',(7.47660065607859,-0.00030677023753798,
4.41625647512786));
#38282=CARTESIAN_POINT('Ctrl Pts',(7.47881911491479,-0.0195780710793754,
4.41641565502598));
#38283=CARTESIAN_POINT('Ctrl Pts',(7.4969428524386,-0.176849480241104,4.4064317922735));
#38284=CARTESIAN_POINT('Ctrl Pts',(7.53097186865002,-0.44664354691983,4.20594845626764));
#38285=CARTESIAN_POINT('Ctrl Pts',(7.57868770471286,-0.414791917646955,
3.73570302684109));
#38286=CARTESIAN_POINT('Ctrl Pts',(7.62640354077569,-0.00203048755240202,
3.50816557464413));
#38287=CARTESIAN_POINT('Ctrl Pts',(7.67411937683853,0.412595570264971,3.73228724307244));
#38288=CARTESIAN_POINT('Ctrl Pts',(7.72183521290137,0.448328767436039,4.20225365549051));
#38289=CARTESIAN_POINT('Ctrl Pts',(7.75599563931472,0.179163779268806,4.40574053813273));
#38290=CARTESIAN_POINT('Ctrl Pts',(7.77425078704046,0.0207354574140521,
4.41639833498254));
#38291=CARTESIAN_POINT('Ctrl Pts',(7.77660065607859,0.000318631424802297,
4.41622521972442));
#38292=CARTESIAN_POINT('Ctrl Pts',(7.5733993439214,-0.000257198714157839,
4.41635988094829));
#38293=CARTESIAN_POINT('Ctrl Pts',(7.57514899459915,-0.0154461882200338,
4.41646996636401));
#38294=CARTESIAN_POINT('Ctrl Pts',(7.59280392396451,-0.168599214901356,
4.40881268721627));
#38295=CARTESIAN_POINT('Ctrl Pts',(7.62636413201748,-0.440384235482588,
4.21901358396786));
#38296=CARTESIAN_POINT('Ctrl Pts',(7.67407996808031,-0.422396009600076,
3.7480340579683));
#38297=CARTESIAN_POINT('Ctrl Pts',(7.72179580414317,-0.0165150286377962,
3.50843873354525));
#38298=CARTESIAN_POINT('Ctrl Pts',(7.76951164020598,0.404531957204003,3.72025168374225));
#38299=CARTESIAN_POINT('Ctrl Pts',(7.81722747626884,0.454091022239626,4.18896181724392));
#38300=CARTESIAN_POINT('Ctrl Pts',(7.85185671084063,0.187425762196077,4.40318800700955));
#38301=CARTESIAN_POINT('Ctrl Pts',(7.87058066672482,0.02486112795907,4.41632944836175));
#38302=CARTESIAN_POINT('Ctrl Pts',(7.8733993439214,0.000353153796088627,
4.4161078667978));
#38303=CARTESIAN_POINT('Origin',(3.42660065607856,0.,4.));
#38304=CARTESIAN_POINT('',(7.17660065607858,-0.000163391746992416,4.4152468210878));
#38305=CARTESIAN_POINT('',(7.2733993439214,-0.000222139526412562,4.4153039283715));
#38306=CARTESIAN_POINT('',(3.42660065607856,4.87367679877478E-13,4.415875));
#38307=CARTESIAN_POINT('Ctrl Pts',(7.17660065607859,-0.000163391746992363,
4.4152468210878));
#38308=CARTESIAN_POINT('Ctrl Pts',(7.18338744278911,-0.0594844418834033,
4.41545575762517));
#38309=CARTESIAN_POINT('Ctrl Pts',(7.20607950818724,-0.257561782965025,
4.37580284351512));
#38310=CARTESIAN_POINT('Ctrl Pts',(7.24467685227299,-0.486676365692783,
4.07107270446015));
#38311=CARTESIAN_POINT('Ctrl Pts',(7.29239268833582,-0.322996137187983,
3.62908393881966));
#38312=CARTESIAN_POINT('Ctrl Pts',(7.34010852439867,0.137296434535941,3.52771310152703));
#38313=CARTESIAN_POINT('Ctrl Pts',(7.3878243604615,0.471507566988788,3.86005058906394));
#38314=CARTESIAN_POINT('Ctrl Pts',(7.43332173768814,0.377318713751663,4.29947917201381));
#38315=CARTESIAN_POINT('Ctrl Pts',(7.46291383622717,0.118587850938607,4.41527441201542));
#38316=CARTESIAN_POINT('Ctrl Pts',(7.47660065607859,-0.00030677023753798,
4.41625647512786));
#38317=CARTESIAN_POINT('Ctrl Pts',(7.2733993439214,-0.000222139526412493,
4.4153039283715));
#38318=CARTESIAN_POINT('Ctrl Pts',(7.27971732247348,-0.0554265094472961,
4.41557047734173));
#38319=CARTESIAN_POINT('Ctrl Pts',(7.30194057971316,-0.249272617462211,
4.37960776139715));
#38320=CARTESIAN_POINT('Ctrl Pts',(7.34006911564044,-0.484372034479295,
4.08537538031203));
#38321=CARTESIAN_POINT('Ctrl Pts',(7.3877849517033,-0.333780171974684,3.63875766810317));
#38322=CARTESIAN_POINT('Ctrl Pts',(7.43550078776612,0.123327161313159,3.52387434835784));
#38323=CARTESIAN_POINT('Ctrl Pts',(7.48321662382897,0.467181263150904,3.84622454030349));
#38324=CARTESIAN_POINT('Ctrl Pts',(7.52918280921405,0.385138488472668,4.29279105563264));
#38325=CARTESIAN_POINT('Ctrl Pts',(7.55924371591154,0.122630008444172,4.41546922990911));
#38326=CARTESIAN_POINT('Ctrl Pts',(7.5733993439214,-0.000257198714157839,
4.41635988094829));
#38327=CARTESIAN_POINT('Origin',(3.42660065607856,0.,4.));
#38328=CARTESIAN_POINT('',(6.87660065607859,0.000369753976522709,4.4156559906262));
#38329=CARTESIAN_POINT('',(6.9733993439214,0.000344359613660638,4.41554532105972));
#38330=CARTESIAN_POINT('',(3.42660065607856,4.87367679877478E-13,4.415875));
#38331=CARTESIAN_POINT('Ctrl Pts',(6.87660065607859,0.000369753976522759,
4.4156559906262));
#38332=CARTESIAN_POINT('Ctrl Pts',(6.88795577066343,-0.0986361616094132,
4.41481368816743));
#38333=CARTESIAN_POINT('Ctrl Pts',(6.91521616393589,-0.337621850525623,
4.32977807754403));
#38334=CARTESIAN_POINT('Ctrl Pts',(6.95838183589596,-0.486886005735063,
3.93038141845316));
#38335=CARTESIAN_POINT('Ctrl Pts',(7.0060976719588,-0.204771183672361,3.55281534000283));
#38336=CARTESIAN_POINT('Ctrl Pts',(7.05381350802163,0.265389096458903,3.58590591031157));
#38337=CARTESIAN_POINT('Ctrl Pts',(7.10152934408448,0.491837993618785,3.99926540470374));
#38338=CARTESIAN_POINT('Ctrl Pts',(7.14245839343679,0.298657604039877,4.35441002681052));
#38339=CARTESIAN_POINT('Ctrl Pts',(7.16748216410149,0.0795383202432945,
4.41496610118));
#38340=CARTESIAN_POINT('Ctrl Pts',(7.17660065607859,-0.000163391746992363,
4.4152468210878));
#38341=CARTESIAN_POINT('Ctrl Pts',(6.9733993439214,0.00034435961366068,
4.41554532105972));
#38342=CARTESIAN_POINT('Ctrl Pts',(6.9842856503478,-0.0946377878655052,
4.41480662962373));
#38343=CARTESIAN_POINT('Ctrl Pts',(7.0110772354618,-0.329510302625179,4.33529054280597));
#38344=CARTESIAN_POINT('Ctrl Pts',(7.05377409926342,-0.488725618924084,
3.94475128051735));
#38345=CARTESIAN_POINT('Ctrl Pts',(7.10148993532626,-0.21785253135038,3.55904022429238));
#38346=CARTESIAN_POINT('Ctrl Pts',(7.14920577138909,0.253078023397415,3.57826934481931));
#38347=CARTESIAN_POINT('Ctrl Pts',(7.19692160745195,0.491603063369337,3.98478019943955));
#38348=CARTESIAN_POINT('Ctrl Pts',(7.2383194649627,0.306874094293292,4.34959156107453));
#38349=CARTESIAN_POINT('Ctrl Pts',(7.26381204378586,0.0835484619188193,
4.41489945011039));
#38350=CARTESIAN_POINT('Ctrl Pts',(7.2733993439214,-0.000222139526412493,
4.4153039283715));
#38351=CARTESIAN_POINT('Origin',(3.42660065607856,0.,4.));
#38352=CARTESIAN_POINT('',(6.57660065607858,1.8302248101926E-5,4.41656360501758));
#38353=CARTESIAN_POINT('',(6.6733993439214,7.63499956435865E-5,4.4165465803965));
#38354=CARTESIAN_POINT('',(3.42660065607856,4.87367679877478E-13,4.415875));
#38355=CARTESIAN_POINT('Ctrl Pts',(6.57660065607858,1.83022481018748E-5,
4.41656360501758));
#38356=CARTESIAN_POINT('Ctrl Pts',(6.57661881985014,-0.000139156870309867,
4.41656362372179));
#38357=CARTESIAN_POINT('Ctrl Pts',(6.59254226230931,-0.138177237712184,
4.41649399470799));
#38358=CARTESIAN_POINT('Ctrl Pts',(6.62437098345609,-0.41404349770976,4.26553045144514));
#38359=CARTESIAN_POINT('Ctrl Pts',(6.67208681951894,-0.447234019333667,
3.79538894860702));
#38360=CARTESIAN_POINT('Ctrl Pts',(6.71980265558177,-0.0698021891909718,
3.51313682319347));
#38361=CARTESIAN_POINT('Ctrl Pts',(6.76751849164461,0.371772181936036,3.67798293440124));
#38362=CARTESIAN_POINT('Ctrl Pts',(6.81523432770745,0.471920133146607,4.13853999974893));
#38363=CARTESIAN_POINT('Ctrl Pts',(6.85159504918544,0.21800401543618,4.39254992240466));
#38364=CARTESIAN_POINT('Ctrl Pts',(6.87205049197582,0.0400429038769189,
4.41599351380864));
#38365=CARTESIAN_POINT('Ctrl Pts',(6.87660065607859,0.000369753976522759,
4.4156559906262));
#38366=CARTESIAN_POINT('Ctrl Pts',(6.6733993439214,7.63499956435956E-5,
4.4165465803965));
#38367=CARTESIAN_POINT('Ctrl Pts',(6.68885397822212,-0.133927014866661,
4.41622291450327));
#38368=CARTESIAN_POINT('Ctrl Pts',(6.72021389121046,-0.406451392834186,
4.27318229388465));
#38369=CARTESIAN_POINT('Ctrl Pts',(6.76747908288639,-0.453085647428837,
3.80864864857145));
#38370=CARTESIAN_POINT('Ctrl Pts',(6.81519491894923,-0.0841006081168706,
3.51540431248109));
#38371=CARTESIAN_POINT('Ctrl Pts',(6.86291075501207,0.362121456530253,3.66717299786736));
#38372=CARTESIAN_POINT('Ctrl Pts',(6.91062659107491,0.475798562415156,4.124581128109));
#38373=CARTESIAN_POINT('Ctrl Pts',(6.94745612071136,0.226294304474162,4.38932900794447));
#38374=CARTESIAN_POINT('Ctrl Pts',(6.96838037166019,0.0441344886838037,
4.41588588393584));
#38375=CARTESIAN_POINT('Ctrl Pts',(6.9733993439214,0.00034435961366068,
4.41554532105972));
#38376=CARTESIAN_POINT('Origin',(3.42660065607856,0.,4.));
#38377=CARTESIAN_POINT('',(6.27660065607859,-8.94903747701068E-6,4.41582842213685));
#38378=CARTESIAN_POINT('',(6.3733993439214,-0.000441664590319634,4.4157663968931));
#38379=CARTESIAN_POINT('',(3.42660065607856,4.87367679877478E-13,4.415875));
#38380=CARTESIAN_POINT('Ctrl Pts',(6.27660065607859,-8.94903747701223E-6,
4.41582842213685));
#38381=CARTESIAN_POINT('Ctrl Pts',(6.28118714772447,-0.0399801639742102,
4.41579747358059));
#38382=CARTESIAN_POINT('Ctrl Pts',(6.29372627871415,-0.149263049162913,
4.40013952362907));
#38383=CARTESIAN_POINT('Ctrl Pts',(6.31421804904765,-0.307151379675736,
4.3060270879454));
#38384=CARTESIAN_POINT('Ctrl Pts',(6.33807596707907,-0.416657206472865,
4.12081787696614));
#38385=CARTESIAN_POINT('Ctrl Pts',(6.36193388511048,-0.422829889105799,
3.9075587958503));
#38386=CARTESIAN_POINT('Ctrl Pts',(6.39374444248571,-0.296437506874183,
3.64987069373525));
#38387=CARTESIAN_POINT('Ctrl Pts',(6.43350763920474,0.0703302468340302,
3.51324810367198));
#38388=CARTESIAN_POINT('Ctrl Pts',(6.48122347526758,0.448014600657906,3.7964368525222));
#38389=CARTESIAN_POINT('Ctrl Pts',(6.52892114755886,0.413253290380966,4.26628466471864));
#38390=CARTESIAN_POINT('Ctrl Pts',(6.56071354116253,0.137741412285014,4.41654724519979));
#38391=CARTESIAN_POINT('Ctrl Pts',(6.57660065607858,1.83022481018748E-5,
4.41656360501758));
#38392=CARTESIAN_POINT('Ctrl Pts',(6.3733993439214,-0.000441664590319611,
4.4157663968931));
#38393=CARTESIAN_POINT('Ctrl Pts',(6.37751702740883,-0.0362476131304844,
4.41610293027605));
#38394=CARTESIAN_POINT('Ctrl Pts',(6.39753998958387,-0.210006484715375,
4.39546152579387));
#38395=CARTESIAN_POINT('Ctrl Pts',(6.43346823044653,-0.468271923807345,
4.15124960425567));
#38396=CARTESIAN_POINT('Ctrl Pts',(6.48118406650937,-0.380227249479543,
3.6882349865083));
#38397=CARTESIAN_POINT('Ctrl Pts',(6.52889990257221,0.0564566449812287,
3.51140415777354));
#38398=CARTESIAN_POINT('Ctrl Pts',(6.57661573863504,0.441574375138847,3.78331933667001));
#38399=CARTESIAN_POINT('Ctrl Pts',(6.62433157469789,0.421040068198854,4.25418342072721));
#38400=CARTESIAN_POINT('Ctrl Pts',(6.65659277646,0.145792717270209,4.41473316952435));
#38401=CARTESIAN_POINT('Ctrl Pts',(6.6729486995345,0.00398377756883227,
4.41655601822694));
#38402=CARTESIAN_POINT('Ctrl Pts',(6.6733993439214,7.63499956435956E-5,
4.4165465803965));
#38403=CARTESIAN_POINT('Origin',(3.42660065607856,0.,4.));
#38404=CARTESIAN_POINT('',(5.97660065607859,-9.19412645702589E-6,4.41589218083175));
#38405=CARTESIAN_POINT('',(6.0733993439214,-6.65563173402051E-6,4.41590255337155));
#38406=CARTESIAN_POINT('',(3.42660065607856,4.87367679877478E-13,4.415875));
#38407=CARTESIAN_POINT('Ctrl Pts',(5.97660065607858,-9.19412645705893E-6,
4.41589218083175));
#38408=CARTESIAN_POINT('Ctrl Pts',(5.97780283625498,-0.0104787976275591,
4.4159022685469));
#38409=CARTESIAN_POINT('Ctrl Pts',(5.98695765577519,-0.0902010538040918,
4.41295272969856));
#38410=CARTESIAN_POINT('Ctrl Pts',(6.0040651146392,-0.23587461323539,4.36380751861078));
#38411=CARTESIAN_POINT('Ctrl Pts',(6.02792303267061,-0.381351759249696,
4.20630938167977));
#38412=CARTESIAN_POINT('Ctrl Pts',(6.05178095070204,-0.433578399193506,
3.9983625870902));
#38413=CARTESIAN_POINT('Ctrl Pts',(6.07563886873346,-0.379782579589031,
3.79081692866841));
#38414=CARTESIAN_POINT('Ctrl Pts',(6.09949678676487,-0.233120953551068,
3.63442082419035));
#38415=CARTESIAN_POINT('Ctrl Pts',(6.12335470479629,-0.0294522997972467,
3.5674214393556));
#38416=CARTESIAN_POINT('Ctrl Pts',(6.14721262282771,0.181413325723775,3.60619428643423));
#38417=CARTESIAN_POINT('Ctrl Pts',(6.17107054085913,0.347927737305898,3.74127281623538));
#38418=CARTESIAN_POINT('Ctrl Pts',(6.19492845889055,0.429346806292137,3.93959933010928));
#38419=CARTESIAN_POINT('Ctrl Pts',(6.21878637692197,0.405811992579865,4.15272917617017));
#38420=CARTESIAN_POINT('Ctrl Pts',(6.24264429495339,0.282982581651336,4.32844890303245));
#38421=CARTESIAN_POINT('Ctrl Pts',(6.26191572133893,0.127967070080381,4.40561019629887));
#38422=CARTESIAN_POINT('Ctrl Pts',(6.27323450838066,0.029326984292613,4.415851136102));
#38423=CARTESIAN_POINT('Ctrl Pts',(6.27660065607859,-8.94903747701223E-6,
4.41582842213685));
#38424=CARTESIAN_POINT('Ctrl Pts',(6.0733993439214,-6.65563173397714E-6,
4.41590255337156));
#38425=CARTESIAN_POINT('Ctrl Pts',(6.07413271593935,-0.00639299139291402,
4.41590724351385));
#38426=CARTESIAN_POINT('Ctrl Pts',(6.0828187273011,-0.0820297780542147,
4.41420140028919));
#38427=CARTESIAN_POINT('Ctrl Pts',(6.09945737800665,-0.2250554921608,4.3705991908187));
#38428=CARTESIAN_POINT('Ctrl Pts',(6.12331529603809,-0.375113923638194,
4.21744656883549));
#38429=CARTESIAN_POINT('Ctrl Pts',(6.1471732140695,-0.433431396087355,4.01114207710762));
#38430=CARTESIAN_POINT('Ctrl Pts',(6.17103113210093,-0.385792139046387,
3.80207577201042));
#38431=CARTESIAN_POINT('Ctrl Pts',(6.19488905013233,-0.243761337718234,
3.64147770828707));
#38432=CARTESIAN_POINT('Ctrl Pts',(6.21874696816376,-0.042227823444436,
3.56841523311022));
#38433=CARTESIAN_POINT('Ctrl Pts',(6.24260488619517,0.16982704650124,3.60113783246665));
#38434=CARTESIAN_POINT('Ctrl Pts',(6.2664628042266,0.339985970990829,3.73091992247201));
#38435=CARTESIAN_POINT('Ctrl Pts',(6.29032072225801,0.427700638223926,3.92738904240251));
#38436=CARTESIAN_POINT('Ctrl Pts',(6.31417864028943,0.409561128158778,4.13996490148311));
#38437=CARTESIAN_POINT('Ctrl Pts',(6.34187151417723,0.27471212230801,4.35031587281991));
#38438=CARTESIAN_POINT('Ctrl Pts',(6.36161174872122,0.102059178040878,4.41480301073152));
#38439=CARTESIAN_POINT('Ctrl Pts',(6.3733993439214,-0.000441664590319611,
4.4157663968931));
#38440=CARTESIAN_POINT('Origin',(3.42660065607856,0.,4.));
#38441=CARTESIAN_POINT('',(5.67660065607858,1.06631253201556E-5,4.41586554077139));
#38442=CARTESIAN_POINT('',(5.7733993439214,9.17748676071416E-6,4.4158542849441));
#38443=CARTESIAN_POINT('',(3.42660065607856,4.87367679877478E-13,4.415875));
#38444=CARTESIAN_POINT('Ctrl Pts',(5.67660065607858,1.06631253201268E-5,
4.41586554077139));
#38445=CARTESIAN_POINT('Ctrl Pts',(5.68237116412931,-0.050253077703417,
4.41581669384736));
#38446=CARTESIAN_POINT('Ctrl Pts',(5.69609431152383,-0.169828933264711,
4.3941204493343));
#38447=CARTESIAN_POINT('Ctrl Pts',(5.71777009826218,-0.329222253834466,
4.28214440376531));
#38448=CARTESIAN_POINT('Ctrl Pts',(5.74162801629359,-0.424158110434281,
4.08990358344764));
#38449=CARTESIAN_POINT('Ctrl Pts',(5.76548593432501,-0.415375755386326,
3.8756788878607));
#38450=CARTESIAN_POINT('Ctrl Pts',(5.78934385235642,-0.305022713182347,
3.69185409099321));
#38451=CARTESIAN_POINT('Ctrl Pts',(5.81320177038785,-0.120083309624962,
3.58337936191985));
#38452=CARTESIAN_POINT('Ctrl Pts',(5.83705968841926,0.0942197354074567,
3.57677972866706));
#38453=CARTESIAN_POINT('Ctrl Pts',(5.86091760645069,0.285483486244351,3.673668977605));
#38454=CARTESIAN_POINT('Ctrl Pts',(5.8847755244821,0.406938752801468,3.85035505520226));
#38455=CARTESIAN_POINT('Ctrl Pts',(5.90863344251353,0.428886400972996,4.06363338935351));
#38456=CARTESIAN_POINT('Ctrl Pts',(5.93249136054494,0.345959657594393,4.261351642888));
#38457=CARTESIAN_POINT('Ctrl Pts',(5.95514709839996,0.186877681905787,4.38841966610496));
#38458=CARTESIAN_POINT('Ctrl Pts',(5.96985019691118,0.0587795235055939,
4.41583553648629));
#38459=CARTESIAN_POINT('Ctrl Pts',(5.97660065607858,-9.19412645705893E-6,
4.41589218083175));
#38460=CARTESIAN_POINT('Ctrl Pts',(5.7733993439214,9.17748676073846E-6,
4.4158542849441));
#38461=CARTESIAN_POINT('Ctrl Pts',(5.77870104381367,-0.0461746181927863,
4.41581721944429));
#38462=CARTESIAN_POINT('Ctrl Pts',(5.79195538304975,-0.161664917198308,
4.3966319946429));
#38463=CARTESIAN_POINT('Ctrl Pts',(5.81316236162963,-0.320769768688322,
4.29171820750724));
#38464=CARTESIAN_POINT('Ctrl Pts',(5.83702027966105,-0.421326288178809,
4.10235681181338));
#38465=CARTESIAN_POINT('Ctrl Pts',(5.86087819769247,-0.418857046020503,
3.88796639709818));
#38466=CARTESIAN_POINT('Ctrl Pts',(5.88473611572389,-0.313965860818636,
3.70097123187977));
#38467=CARTESIAN_POINT('Ctrl Pts',(5.90859403375531,-0.132301443679057,
3.58709678011166));
#38468=CARTESIAN_POINT('Ctrl Pts',(5.93245195178673,0.0817142298265842,
3.57418834816524));
#38469=CARTESIAN_POINT('Ctrl Pts',(5.95630986981814,0.275748643515392,3.66540258613358));
#38470=CARTESIAN_POINT('Ctrl Pts',(5.98016778784957,0.402354822815078,3.83843477537114));
#38471=CARTESIAN_POINT('Ctrl Pts',(6.00402570588098,0.430574627524036,4.05097449853386));
#38472=CARTESIAN_POINT('Ctrl Pts',(6.02788362391241,0.353506566116634,4.25104874587108));
#38473=CARTESIAN_POINT('Ctrl Pts',(6.05100816992587,0.195023852357142,4.38547315270063));
#38474=CARTESIAN_POINT('Ctrl Pts',(6.06618007659554,0.06286002589468,4.4158563839102));
#38475=CARTESIAN_POINT('Ctrl Pts',(6.0733993439214,-6.65563173397714E-6,
4.41590255337156));
#38476=CARTESIAN_POINT('Origin',(3.42660065607856,0.,4.));
#38477=CARTESIAN_POINT('',(5.37660065607858,-1.01751121954902E-5,4.41586038335289));
#38478=CARTESIAN_POINT('',(5.4733993439214,-1.09014992595302E-5,4.41587264340464));
#38479=CARTESIAN_POINT('',(3.42660065607856,4.87367679877478E-13,4.415875));
#38480=CARTESIAN_POINT('Ctrl Pts',(5.37660065607859,-1.01751121954468E-5,
4.41586038335289));
#38481=CARTESIAN_POINT('Ctrl Pts',(5.37898685265982,-0.0207957689391596,
4.41587928195339));
#38482=CARTESIAN_POINT('Ctrl Pts',(5.38932568858487,-0.110842971866809,
4.40924760552439));
#38483=CARTESIAN_POINT('Ctrl Pts',(5.40761716385372,-0.26226226804932,4.34526983614494));
#38484=CARTESIAN_POINT('Ctrl Pts',(5.43147508188515,-0.395631058815178,
4.17739453851434));
#38485=CARTESIAN_POINT('Ctrl Pts',(5.45533299991656,-0.432257278927009,
3.96614144408682));
#38486=CARTESIAN_POINT('Ctrl Pts',(5.47919091794798,-0.363184819889405,
3.76316768886851));
#38487=CARTESIAN_POINT('Ctrl Pts',(5.5030488359794,-0.205303779432806,3.61810588490468));
#38488=CARTESIAN_POINT('Ctrl Pts',(5.52690675401082,0.00277962745745752,
3.56642759466814));
#38489=CARTESIAN_POINT('Ctrl Pts',(5.55076467204224,0.210183339719457,3.62076956781107));
#38490=CARTESIAN_POINT('Ctrl Pts',(5.57462259007365,0.36619150013966,3.76784371165257));
#38491=CARTESIAN_POINT('Ctrl Pts',(5.59848050810508,0.432655863921731,3.97168639180759));
#38492=CARTESIAN_POINT('Ctrl Pts',(5.62233842613649,0.393324083661671,4.18245252040861));
#38493=CARTESIAN_POINT('Ctrl Pts',(5.64619634416792,0.257813851021257,4.34860403787086));
#38494=CARTESIAN_POINT('Ctrl Pts',(5.66428375414861,0.107285005985459,4.40994309575933));
#38495=CARTESIAN_POINT('Ctrl Pts',(5.6744185247855,0.0190180158238588,4.41588401235146));
#38496=CARTESIAN_POINT('Ctrl Pts',(5.67660065607858,1.06631253201268E-5,
4.41586554077139));
#38497=CARTESIAN_POINT('Ctrl Pts',(5.4733993439214,-1.0901499259525E-5,
4.41587264340464));
#38498=CARTESIAN_POINT('Ctrl Pts',(5.47531673234419,-0.0167114040746605,
4.41588973972128));
#38499=CARTESIAN_POINT('Ctrl Pts',(5.48518676011079,-0.102669266038577,
4.41080986982701));
#38500=CARTESIAN_POINT('Ctrl Pts',(5.50300942722118,-0.251979671819092,
4.35284416104532));
#38501=CARTESIAN_POINT('Ctrl Pts',(5.52686734525261,-0.390234841353927,
4.18896964197264));
#38502=CARTESIAN_POINT('Ctrl Pts',(5.55072526328402,-0.433066962396004,
3.97888689800548));
#38503=CARTESIAN_POINT('Ctrl Pts',(5.57458318131544,-0.370002414621403,
3.77396688259));
#38504=CARTESIAN_POINT('Ctrl Pts',(5.59844109934686,-0.21646219781534,3.62431812139094));
#38505=CARTESIAN_POINT('Ctrl Pts',(5.62229901737828,-0.00999107731853999,
3.56653381289738));
#38506=CARTESIAN_POINT('Ctrl Pts',(5.64615693540971,0.198923133709572,3.61474379450078));
#38507=CARTESIAN_POINT('Ctrl Pts',(5.67001485344111,0.359195220034686,3.75715941257656));
#38508=CARTESIAN_POINT('Ctrl Pts',(5.69387277147254,0.431634290692432,3.95895616900985));
#38509=CARTESIAN_POINT('Ctrl Pts',(5.71773068950395,0.398527019959163,4.1707892603438));
#38510=CARTESIAN_POINT('Ctrl Pts',(5.74158860753538,0.267969036875697,4.34085972491723));
#38511=CARTESIAN_POINT('Ctrl Pts',(5.76014482567452,0.115458993192439,4.40830959117706));
#38512=CARTESIAN_POINT('Ctrl Pts',(5.77074840446986,0.0231018550196917,
4.41587281831976));
#38513=CARTESIAN_POINT('Ctrl Pts',(5.7733993439214,9.17748676073846E-6,
4.4158542849441));
#38514=CARTESIAN_POINT('Origin',(3.42660065607856,0.,4.));
#38515=CARTESIAN_POINT('',(5.07660065607859,8.10857529294212E-6,4.41589722116852));
#38516=CARTESIAN_POINT('',(5.1733993439214,1.02299162792543E-5,4.4158851107878));
#38517=CARTESIAN_POINT('',(3.42660065607856,4.87367679877478E-13,4.415875));
#38518=CARTESIAN_POINT('Ctrl Pts',(5.07660065607858,8.10857529294148E-6,
4.41589722116852));
#38519=CARTESIAN_POINT('Ctrl Pts',(5.08355518053415,-0.060555656273516,
4.41584370653314));
#38520=CARTESIAN_POINT('Ctrl Pts',(5.09846234433351,-0.190424342306974,
4.38715451669839));
#38521=CARTESIAN_POINT('Ctrl Pts',(5.1213221474767,-0.349282119693095,4.256894448863));
#38522=CARTESIAN_POINT('Ctrl Pts',(5.1451800655081,-0.4296670234643,4.05812921762123));
#38523=CARTESIAN_POINT('Ctrl Pts',(5.16903798353954,-0.404986636103755,
3.84514980926298));
#38524=CARTESIAN_POINT('Ctrl Pts',(5.19289590157095,-0.281275984601366,
3.67003549057442));
#38525=CARTESIAN_POINT('Ctrl Pts',(5.21675381960238,-0.0887856930599551,
3.5756064824932));
#38526=CARTESIAN_POINT('Ctrl Pts',(5.24061173763379,0.125415118908336,3.58495324968971));
#38527=CARTESIAN_POINT('Ctrl Pts',(5.26446965566521,0.308948518064291,3.69579025298356));
#38528=CARTESIAN_POINT('Ctrl Pts',(5.28832757369662,0.416935588964862,3.88101482593007));
#38529=CARTESIAN_POINT('Ctrl Pts',(5.31218549172805,0.422970551266107,4.09533451502773));
#38530=CARTESIAN_POINT('Ctrl Pts',(5.33604340975946,0.325577692296299,4.28634231834109));
#38531=CARTESIAN_POINT('Ctrl Pts',(5.35751513120965,0.166275769440666,4.39523064161658));
#38532=CARTESIAN_POINT('Ctrl Pts',(5.37103421331602,0.0484777907299229,
4.41581629730449));
#38533=CARTESIAN_POINT('Ctrl Pts',(5.37660065607859,-1.01751121954468E-5,
4.41586038335289));
#38534=CARTESIAN_POINT('Ctrl Pts',(5.1733993439214,1.02299162792474E-5,
4.4158851107878));
#38535=CARTESIAN_POINT('Ctrl Pts',(5.17988506021851,-0.0564756498766958,
4.41582730150705));
#38536=CARTESIAN_POINT('Ctrl Pts',(5.19432341585943,-0.182274442988225,
4.39002065289559));
#38537=CARTESIAN_POINT('Ctrl Pts',(5.21671441084416,-0.341564590845109,
4.26707000444592));
#38538=CARTESIAN_POINT('Ctrl Pts',(5.24057232887557,-0.427768622694993,
4.07075847957352));
#38539=CARTESIAN_POINT('Ctrl Pts',(5.264430246907,-0.409371574112622,3.85714457902312));
#38540=CARTESIAN_POINT('Ctrl Pts',(5.2882881649384,-0.290872024601924,3.6784627202051));
#38541=CARTESIAN_POINT('Ctrl Pts',(5.31214608296984,-0.101246341881189,
3.57840548479658));
#38542=CARTESIAN_POINT('Ctrl Pts',(5.33600400100125,0.113136829324483,3.58143959235932));
#38543=CARTESIAN_POINT('Ctrl Pts',(5.35986191903268,0.299854963974951,3.68682312094679));
#38544=CARTESIAN_POINT('Ctrl Pts',(5.38371983706408,0.413250392048343,3.8687869272297));
#38545=CARTESIAN_POINT('Ctrl Pts',(5.40757775509551,0.425594842551202,4.08283590397723));
#38546=CARTESIAN_POINT('Ctrl Pts',(5.43143567312693,0.333869761079625,4.27662924579771));
#38547=CARTESIAN_POINT('Ctrl Pts',(5.45337620273556,0.174437273907163,4.39264091290779));
#38548=CARTESIAN_POINT('Ctrl Pts',(5.46736409300038,0.0525562895569378,
4.41581883033293));
#38549=CARTESIAN_POINT('Ctrl Pts',(5.4733993439214,-1.0901499259525E-5,
4.41587264340464));
#38550=CARTESIAN_POINT('Origin',(3.42660065607856,0.,4.));
#38551=CARTESIAN_POINT('',(4.77660065607858,-3.27394476109793E-6,4.41584059078716));
#38552=CARTESIAN_POINT('',(4.8733993439214,-6.67049670156904E-6,4.4158459349409));
#38553=CARTESIAN_POINT('',(3.42660065607856,4.87367679877478E-13,4.415875));
#38554=CARTESIAN_POINT('Ctrl Pts',(4.77660065607858,-3.27394476113199E-6,
4.41584059078717));
#38555=CARTESIAN_POINT('Ctrl Pts',(4.78017086906467,-0.0311067951354469,
4.4158491206715));
#38556=CARTESIAN_POINT('Ctrl Pts',(4.79169372139456,-0.131487321212171,
4.40473555835468));
#38557=CARTESIAN_POINT('Ctrl Pts',(4.81116921306824,-0.287199161490599,
4.32482210305491));
#38558=CARTESIAN_POINT('Ctrl Pts',(4.83502713109967,-0.407721671464292,
4.14749845969467));
#38559=CARTESIAN_POINT('Ctrl Pts',(4.85888504913109,-0.42854512664958,3.93410742516172));
#38560=CARTESIAN_POINT('Ctrl Pts',(4.8827429671625,-0.344577625034195,3.73682892005441));
#38561=CARTESIAN_POINT('Ctrl Pts',(4.90660088519393,-0.176351507991885,
3.60390291263011));
#38562=CARTESIAN_POINT('Ctrl Pts',(4.93045880322534,0.0349973564730633,
3.56783343253575));
#38563=CARTESIAN_POINT('Ctrl Pts',(4.95431672125677,0.237788413971502,3.63744045016736));
#38564=CARTESIAN_POINT('Ctrl Pts',(4.97817463928818,0.382433727027559,3.79570315365689));
#38565=CARTESIAN_POINT('Ctrl Pts',(5.0020325573196,0.433563576539811,4.00392200101168));
#38566=CARTESIAN_POINT('Ctrl Pts',(5.02589047535102,0.378675321553375,4.21118181228595));
#38567=CARTESIAN_POINT('Ctrl Pts',(5.04974839338244,0.231190635538481,4.36680191797922));
#38568=CARTESIAN_POINT('Ctrl Pts',(5.0666517869583,0.086644022961884,4.4135113916189));
#38569=CARTESIAN_POINT('Ctrl Pts',(5.07560254119034,0.00870023350343714,
4.41590490160082));
#38570=CARTESIAN_POINT('Ctrl Pts',(5.07660065607858,8.10857529294148E-6,
4.41589722116852));
#38571=CARTESIAN_POINT('Ctrl Pts',(4.8733993439214,-6.67049670157252E-6,
4.41584593494091));
#38572=CARTESIAN_POINT('Ctrl Pts',(4.87650074874903,-0.0270249643080214,
4.41586127519519));
#38573=CARTESIAN_POINT('Ctrl Pts',(4.88755479292047,-0.123313358466266,
4.40662010077424));
#38574=CARTESIAN_POINT('Ctrl Pts',(4.90656147643571,-0.277507970732168,
4.33313973520738));
#38575=CARTESIAN_POINT('Ctrl Pts',(4.93041939446713,-0.403200703213916,
4.15944262266324));
#38576=CARTESIAN_POINT('Ctrl Pts',(4.95427731249855,-0.430299880793222,
3.94675744574809));
#38577=CARTESIAN_POINT('Ctrl Pts',(4.97813523052996,-0.352179016385168,
3.7470915236456));
#38578=CARTESIAN_POINT('Ctrl Pts',(5.00199314856139,-0.187940789307144,
3.60926861310034));
#38579=CARTESIAN_POINT('Ctrl Pts',(5.0258510665928,0.0222540801607904,3.56699016996131));
#38580=CARTESIAN_POINT('Ctrl Pts',(5.04970898462423,0.227007220840439,3.63059442521772));
#38581=CARTESIAN_POINT('Ctrl Pts',(5.07356690265564,0.376250912472057,3.7845284059142));
#38582=CARTESIAN_POINT('Ctrl Pts',(5.09742482068706,0.433491007135177,3.99115106069306));
#38583=CARTESIAN_POINT('Ctrl Pts',(5.12128273871848,0.384730742495793,4.19993752217271));
#38584=CARTESIAN_POINT('Ctrl Pts',(5.1451406567499,0.241893331461176,4.35983381329239));
#38585=CARTESIAN_POINT('Ctrl Pts',(5.16251285848421,0.0948160588051851,
4.41219316122439));
#38586=CARTESIAN_POINT('Ctrl Pts',(5.17193242087471,0.0127860645481494,
4.41589818594594));
#38587=CARTESIAN_POINT('Ctrl Pts',(5.1733993439214,1.02299162792474E-5,
4.4158851107878));
#38588=CARTESIAN_POINT('Origin',(3.42660065607856,0.,4.));
#38589=CARTESIAN_POINT('',(4.47660065607858,-1.72413508574122E-6,4.41591032029986));
#38590=CARTESIAN_POINT('',(4.5733993439214,2.6062779713001E-6,4.4159095790646));
#38591=CARTESIAN_POINT('',(3.42660065607856,4.87367679877478E-13,4.415875));
#38592=CARTESIAN_POINT('Ctrl Pts',(4.47660065607858,-1.72413508575881E-6,
4.41591032029986));
#38593=CARTESIAN_POINT('Ctrl Pts',(4.47678655759518,-0.00162050728124812,
4.41591069657345));
#38594=CARTESIAN_POINT('Ctrl Pts',(4.48492509845559,-0.0724886630755744,
4.4155056303295));
#38595=CARTESIAN_POINT('Ctrl Pts',(4.5010162786598,-0.212178818846594,4.37811758201071));
#38596=CARTESIAN_POINT('Ctrl Pts',(4.52487419669122,-0.367409789343613,
4.23022337776645));
#38597=CARTESIAN_POINT('Ctrl Pts',(4.54873211472264,-0.432799058467291,
4.02603328640456));
#38598=CARTESIAN_POINT('Ctrl Pts',(4.57259003275406,-0.392357168499796,
3.8154773474345));
#38599=CARTESIAN_POINT('Ctrl Pts',(4.59644795078547,-0.255973263285106,
3.65004222328625));
#38600=CARTESIAN_POINT('Ctrl Pts',(4.6203058688169,-0.0569969226013119,
3.57018130821703));
#38601=CARTESIAN_POINT('Ctrl Pts',(4.64416378684831,0.155916718210686,3.59542277130738));
#38602=CARTESIAN_POINT('Ctrl Pts',(4.66802170487973,0.330704474340828,3.71959438727947));
#38603=CARTESIAN_POINT('Ctrl Pts',(4.69187962291115,0.424625978282027,3.91233281365517));
#38604=CARTESIAN_POINT('Ctrl Pts',(4.71573754094257,0.41471486395576,4.1265082550995));
#38605=CARTESIAN_POINT('Ctrl Pts',(4.73959545897399,0.303394668785218,4.30974898215573));
#38606=CARTESIAN_POINT('Ctrl Pts',(4.75988316401932,0.145646585585232,4.40116103141851));
#38607=CARTESIAN_POINT('Ctrl Pts',(4.77221822972086,0.0381762104768988,
4.41583012037823));
#38608=CARTESIAN_POINT('Ctrl Pts',(4.77660065607858,-3.27394476113199E-6,
4.41584059078717));
#38609=CARTESIAN_POINT('Ctrl Pts',(4.5733993439214,2.60627797130011E-6,
4.4159095790646));
#38610=CARTESIAN_POINT('Ctrl Pts',(4.58106907662335,-0.0667838229435618,
4.4158868274511));
#38611=CARTESIAN_POINT('Ctrl Pts',(4.59669144866912,-0.202842099803805,
4.38250385602613));
#38612=CARTESIAN_POINT('Ctrl Pts',(4.62026646005868,-0.360469908510665,
4.24094439618412));
#38613=CARTESIAN_POINT('Ctrl Pts',(4.6441243780901,-0.431844582779732,4.03876871570463));
#38614=CARTESIAN_POINT('Ctrl Pts',(4.66798229612152,-0.397621493350665,
3.82711302819544));
#38615=CARTESIAN_POINT('Ctrl Pts',(4.69184021415294,-0.266169117804412,
3.65773291463971));
#38616=CARTESIAN_POINT('Ctrl Pts',(4.71569813218436,-0.0696311426542753,
3.57204642662242));
#38617=CARTESIAN_POINT('Ctrl Pts',(4.73955605021577,0.143933543589337,3.59100624451743));
#38618=CARTESIAN_POINT('Ctrl Pts',(4.76341396824719,0.322302557754209,3.70997617639404));
#38619=CARTESIAN_POINT('Ctrl Pts',(4.78727188627862,0.421859817202848,3.8998648332327));
#38620=CARTESIAN_POINT('Ctrl Pts',(4.81112980431003,0.41826086011465,4.11423926597311));
#38621=CARTESIAN_POINT('Ctrl Pts',(4.83498772234146,0.312385729531365,4.30067908636799));
#38622=CARTESIAN_POINT('Ctrl Pts',(4.85574423554524,0.15381688120809,4.39891624198015));
#38623=CARTESIAN_POINT('Ctrl Pts',(4.86854810940522,0.04225549351942,4.41582193963064));
#38624=CARTESIAN_POINT('Ctrl Pts',(4.8733993439214,-6.67049670157252E-6,
4.41584593494091));
#38625=CARTESIAN_POINT('Origin',(3.42660065607856,0.,4.));
#38626=CARTESIAN_POINT('',(4.17660065607858,5.88453344125852E-6,4.41584444980552));
#38627=CARTESIAN_POINT('',(4.2733993439214,2.51014653358805E-6,4.41583996132385));
#38628=CARTESIAN_POINT('',(3.42660065607856,4.87367679877478E-13,4.415875));
#38629=CARTESIAN_POINT('Ctrl Pts',(4.17660065607858,5.88453344126799E-6,
4.41584444980552));
#38630=CARTESIAN_POINT('Ctrl Pts',(4.18135488546951,-0.0414115481342504,
4.41582334930757));
#38631=CARTESIAN_POINT('Ctrl Pts',(4.19406175420423,-0.152126265423154,
4.3993918905015));
#38632=CARTESIAN_POINT('Ctrl Pts',(4.21472126228278,-0.310547447266788,
4.30257739619942));
#38633=CARTESIAN_POINT('Ctrl Pts',(4.23857918031418,-0.417556725585918,
4.11678647978038));
#38634=CARTESIAN_POINT('Ctrl Pts',(4.26243709834561,-0.422462345057068,
3.90243789311793));
#38635=CARTESIAN_POINT('Ctrl Pts',(4.28629501637703,-0.324064236326554,
3.71194600226016));
#38636=CARTESIAN_POINT('Ctrl Pts',(4.31015293440845,-0.146423688323203,
3.59189110566319));
#38637=CARTESIAN_POINT('Ctrl Pts',(4.33401085243986,0.0670214896752265,
3.5716299793216));
#38638=CARTESIAN_POINT('Ctrl Pts',(4.35786877047129,0.264078061498623,3.65611697628114));
#38639=CARTESIAN_POINT('Ctrl Pts',(4.38172668850271,0.396560367883193,3.82469274783887));
#38640=CARTESIAN_POINT('Ctrl Pts',(4.40558460653412,0.432072854850341,4.03613591352675));
#38641=CARTESIAN_POINT('Ctrl Pts',(4.42944252456555,0.361931763288092,4.23874286631049));
#38642=CARTESIAN_POINT('Ctrl Pts',(4.45311454108036,0.204524647174786,4.38184685695289));
#38643=CARTESIAN_POINT('Ctrl Pts',(4.46883391825138,0.0676290543833733,
4.4158946000499));
#38644=CARTESIAN_POINT('Ctrl Pts',(4.47660065607858,-1.72413508575881E-6,
4.41591032029986));
#38645=CARTESIAN_POINT('Ctrl Pts',(4.2733993439214,2.51014653359152E-6,
4.41583996132385));
#38646=CARTESIAN_POINT('Ctrl Pts',(4.27768476515387,-0.0373320337329404,
4.41583213221101));
#38647=CARTESIAN_POINT('Ctrl Pts',(4.28992282573015,-0.143955736965383,
4.40160880992953));
#38648=CARTESIAN_POINT('Ctrl Pts',(4.31011352565024,-0.301501118270308,
4.3115924136571));
#38649=CARTESIAN_POINT('Ctrl Pts',(4.33397144368164,-0.413936097932681,
4.12903358037428));
#38650=CARTESIAN_POINT('Ctrl Pts',(4.35782936171308,-0.425152419412173,
3.91492252699502));
#38651=CARTESIAN_POINT('Ctrl Pts',(4.38168727974448,-0.332407397051365,
3.72161523052345));
#38652=CARTESIAN_POINT('Ctrl Pts',(4.40554519777592,-0.158379709595794,
3.5963805946708));
#38653=CARTESIAN_POINT('Ctrl Pts',(4.42940311580732,0.0543761300157755,
3.56984189703405));
#38654=CARTESIAN_POINT('Ctrl Pts',(4.45326103383876,0.25383552520097,3.64848857324589));
#38655=CARTESIAN_POINT('Ctrl Pts',(4.47711895187016,0.39122521984844,3.81308936806525));
#38656=CARTESIAN_POINT('Ctrl Pts',(4.50097686990159,0.432949691632991,4.02339490384879));
#38657=CARTESIAN_POINT('Ctrl Pts',(4.524834787933,0.368806170420464,4.22797974831721));
#38658=CARTESIAN_POINT('Ctrl Pts',(4.54869270596443,0.214479494504121,4.37681733431002));
#38659=CARTESIAN_POINT('Ctrl Pts',(4.56488089129389,0.0741790848482271,
4.4152866170047));
#38660=CARTESIAN_POINT('Ctrl Pts',(4.57311643727954,0.0024660981813593,
4.41591041828323));
#38661=CARTESIAN_POINT('Ctrl Pts',(4.5733993439214,2.60627797130011E-6,
4.4159095790646));
#38662=CARTESIAN_POINT('Origin',(4.,0.,4.));
#38663=CARTESIAN_POINT('',(4.,-7.34788079488412E-17,4.6));
#38664=CARTESIAN_POINT('Origin',(4.,0.,4.));
#38665=CARTESIAN_POINT('',(4.,-0.219892372742957,4.3529863453938));
#38666=CARTESIAN_POINT('Ctrl Pts',(4.,-0.219914231356238,4.35301468169996));
#38667=CARTESIAN_POINT('Ctrl Pts',(4.,-0.219843051329574,4.3531167999744));
#38668=CARTESIAN_POINT('Ctrl Pts',(4.,-0.219771822781512,4.35321888245988));
#38669=CARTESIAN_POINT('Ctrl Pts',(4.,-0.21970054575756,4.3533209291203));
#38670=CARTESIAN_POINT('Ctrl Pts',(4.,-0.207925336055227,4.3701793886806));
#38671=CARTESIAN_POINT('Ctrl Pts',(4.,-0.194831304039315,4.38605734350833));
#38672=CARTESIAN_POINT('Ctrl Pts',(4.,-0.18064579384139,4.40088380688851));
#38673=CARTESIAN_POINT('Ctrl Pts',(4.,-0.168975273508986,4.41308164397169));
#38674=CARTESIAN_POINT('Ctrl Pts',(4.,-0.156565051628872,4.42456888924957));
#38675=CARTESIAN_POINT('Ctrl Pts',(4.,-0.143515931303371,4.43531683418355));
#38676=CARTESIAN_POINT('Ctrl Pts',(4.,-0.133182439541062,4.44382804395605));
#38677=CARTESIAN_POINT('Ctrl Pts',(4.,-0.122447811630206,4.45187590303098));
#38678=CARTESIAN_POINT('Ctrl Pts',(4.,-0.111352162047151,4.45944712768208));
#38679=CARTESIAN_POINT('Ctrl Pts',(4.,-0.105068105051177,4.46373511522897));
#38680=CARTESIAN_POINT('Ctrl Pts',(4.,-0.0986661212125077,4.46787107983396));
#38681=CARTESIAN_POINT('Ctrl Pts',(4.,-0.0921733602714696,4.47184061613108));
#38682=CARTESIAN_POINT('Ctrl Pts',(4.,-0.0718171345235072,4.48428598070136));
#38683=CARTESIAN_POINT('Ctrl Pts',(4.,-0.0505350523745213,4.49512244469223));
#38684=CARTESIAN_POINT('Ctrl Pts',(4.,-0.0285775088988711,4.50429938857761));
#38685=CARTESIAN_POINT('Ctrl Pts',(4.,-0.00645956782426854,4.51354336909515));
#38686=CARTESIAN_POINT('Ctrl Pts',(4.,0.0163444141029789,4.52110543571878));
#38687=CARTESIAN_POINT('Ctrl Pts',(4.,0.0396343143342583,4.52702898180467));
#38688=CARTESIAN_POINT('Ctrl Pts',(4.,0.0479455316904685,4.52914285427945));
#38689=CARTESIAN_POINT('Ctrl Pts',(4.,0.0563191235587283,4.53104786585874));
#38690=CARTESIAN_POINT('Ctrl Pts',(4.,0.0647475081636451,4.53274519105122));
#38691=CARTESIAN_POINT('Ctrl Pts',(4.,0.0709442475001029,4.53399310299165));
#38692=CARTESIAN_POINT('Ctrl Pts',(4.,0.0771669940275102,4.53512789739638));
#38693=CARTESIAN_POINT('Ctrl Pts',(4.,0.0834037601527001,4.53614909266968));
#38694=CARTESIAN_POINT('Ctrl Pts',(4.,0.108500755516298,4.54025842313435));
#38695=CARTESIAN_POINT('Ctrl Pts',(4.,0.133859781029961,4.54253781872753));
#38696=CARTESIAN_POINT('Ctrl Pts',(3.99999999999999,0.159256593756596,4.54305292380224));
#38697=CARTESIAN_POINT('Ctrl Pts',(3.99999999999999,0.185497795908202,4.5435851550133));
#38698=CARTESIAN_POINT('Ctrl Pts',(3.99999999999998,0.211780221987087,4.54223483664603));
#38699=CARTESIAN_POINT('Ctrl Pts',(3.99999999999998,0.237902321580844,4.5390442708621));
#38700=CARTESIAN_POINT('Ctrl Pts',(3.99999999999998,0.243507595489062,4.53835964001621));
#38701=CARTESIAN_POINT('Ctrl Pts',(3.99999999999998,0.249105619801251,4.53759013757336));
#38702=CARTESIAN_POINT('Ctrl Pts',(3.99999999999998,0.254694598474614,4.53673594206822));
#38703=CARTESIAN_POINT('',(4.,-0.219892372743086,3.64701365460628));
#38704=CARTESIAN_POINT('Ctrl Pts',(4.,0.254721014554616,3.46322028700966));
#38705=CARTESIAN_POINT('Ctrl Pts',(4.,0.254552373521139,3.46319452321125));
#38706=CARTESIAN_POINT('Ctrl Pts',(4.,0.254383724765285,3.46316883668624));
#38707=CARTESIAN_POINT('Ctrl Pts',(4.,0.254215068323085,3.46314322746093));
#38708=CARTESIAN_POINT('Ctrl Pts',(4.,0.228435861761457,3.4592288468388));
#38709=CARTESIAN_POINT('Ctrl Pts',(4.,0.202474691352968,3.45711700011808));
#38710=CARTESIAN_POINT('Ctrl Pts',(4.,0.176517231963435,3.45683380906617));
#38711=CARTESIAN_POINT('Ctrl Pts',(4.,0.151199179447316,3.45655759382427));
#38712=CARTESIAN_POINT('Ctrl Pts',(4.,0.125883695414598,3.45802192769867));
#38713=CARTESIAN_POINT('Ctrl Pts',(4.,0.1007794950383,3.46128259448669));
#38714=CARTESIAN_POINT('Ctrl Pts',(4.,0.0854593772715275,3.46327245269535));
#38715=CARTESIAN_POINT('Ctrl Pts',(4.,0.0702187270328167,3.46593187194604));
#38716=CARTESIAN_POINT('Ctrl Pts',(4.,0.0551140352340102,3.4692772918897));
#38717=CARTESIAN_POINT('Ctrl Pts',(4.,0.0468842919617017,3.47110003330284));
#38718=CARTESIAN_POINT('Ctrl Pts',(4.,0.0386923719445779,3.47312744960567));
#38719=CARTESIAN_POINT('Ctrl Pts',(4.,0.0305707631998946,3.47535548770785));
#38720=CARTESIAN_POINT('Ctrl Pts',(4.,0.0102648423897012,3.48092610391051));
#38721=CARTESIAN_POINT('Ctrl Pts',(4.,-0.00963556638195036,3.48775588581666));
#38722=CARTESIAN_POINT('Ctrl Pts',(4.,-0.0289965775380143,3.49587186612014));
#38723=CARTESIAN_POINT('Ctrl Pts',(4.,-0.047965755796229,3.50382359322137));
#38724=CARTESIAN_POINT('Ctrl Pts',(4.,-0.0664174073931304,3.51301096346156));
#38725=CARTESIAN_POINT('Ctrl Pts',(4.,-0.0841982143338667,3.52340033683134));
#38726=CARTESIAN_POINT('Ctrl Pts',(4.,-0.0930898199841631,3.5285957259532));
#38727=CARTESIAN_POINT('Ctrl Pts',(4.,-0.101813128894432,3.53409169793663));
#38728=CARTESIAN_POINT('Ctrl Pts',(4.,-0.110345561972859,3.53988353361915));
#38729=CARTESIAN_POINT('Ctrl Pts',(4.,-0.11586100642067,3.5436274303089));
#38730=CARTESIAN_POINT('Ctrl Pts',(4.,-0.121288652521606,3.54748953413154));
#38731=CARTESIAN_POINT('Ctrl Pts',(4.,-0.126621987542688,3.55146681430013));
#38732=CARTESIAN_POINT('Ctrl Pts',(4.,-0.143297831161627,3.56390265451229));
#38733=CARTESIAN_POINT('Ctrl Pts',(4.,-0.159061930875806,3.57746928852925));
#38734=CARTESIAN_POINT('Ctrl Pts',(4.,-0.173743808224101,3.59211536896244));
#38735=CARTESIAN_POINT('Ctrl Pts',(4.,-0.187864697165731,3.60620182877415));
#38736=CARTESIAN_POINT('Ctrl Pts',(4.,-0.200984288190684,3.62128798311348));
#38737=CARTESIAN_POINT('Ctrl Pts',(4.,-0.212904831975564,3.63731335989365));
#38738=CARTESIAN_POINT('Ctrl Pts',(4.,-0.21528245268753,3.64050971304978));
#38739=CARTESIAN_POINT('Ctrl Pts',(4.,-0.217612227418936,3.64374335030505));
#38740=CARTESIAN_POINT('Ctrl Pts',(4.,-0.219892372743211,3.64701365460636));
#38741=CARTESIAN_POINT('Origin',(4.,0.,4.));
#38742=CARTESIAN_POINT('Origin',(2.,0.,4.));
#38743=CARTESIAN_POINT('',(2.,-7.34788079488412E-17,4.6));
#38744=CARTESIAN_POINT('',(2.,-7.34788079488412E-17,4.6));
#38745=CARTESIAN_POINT('Origin',(2.,0.,4.));
#38746=CARTESIAN_POINT('Origin',(2.,0.,4.));
#38747=CARTESIAN_POINT('Ctrl Pts',(3.95224475517895,0.178288362465424,4.37571967666652));
#38748=CARTESIAN_POINT('Ctrl Pts',(3.96019739452275,0.115708609995841,4.40541533085819));
#38749=CARTESIAN_POINT('Ctrl Pts',(3.97610267321037,-0.0245105356436035,
4.43290545314371));
#38750=CARTESIAN_POINT('Ctrl Pts',(3.99996059124178,-0.228962993402626,
4.36819499612132));
#38751=CARTESIAN_POINT('Ctrl Pts',(4.0238185092732,-0.377374743411151,4.21349068386271));
#38752=CARTESIAN_POINT('Ctrl Pts',(4.04767642730463,-0.433534992178268,
4.00656196868444));
#38753=CARTESIAN_POINT('Ctrl Pts',(4.07153434533603,-0.383670022685343,
3.79803920418254));
#38754=CARTESIAN_POINT('Ctrl Pts',(4.09539226336747,-0.239994733226421,
3.63889579340969));
#38755=CARTESIAN_POINT('Ctrl Pts',(4.11925018139887,-0.0376302499649443,
3.56805514133307));
#38756=CARTESIAN_POINT('Ctrl Pts',(4.1431080994303,0.173933765839147,3.60283521426327));
#38757=CARTESIAN_POINT('Ctrl Pts',(4.16696601746172,0.342967344134064,3.73473372141871));
#38758=CARTESIAN_POINT('Ctrl Pts',(4.19082393549313,0.428135478754777,3.93149662217858));
#38759=CARTESIAN_POINT('Ctrl Pts',(4.21468185352456,0.40861313688017,4.1450106963618));
#38760=CARTESIAN_POINT('Ctrl Pts',(4.23853977155597,0.289173588337559,4.32306558264197));
#38761=CARTESIAN_POINT('Ctrl Pts',(4.2623976895874,0.0990233075312312,4.42212219878201));
#38762=CARTESIAN_POINT('Ctrl Pts',(4.28625560761881,-0.115340915390822,
4.41795840454656));
#38763=CARTESIAN_POINT('Ctrl Pts',(4.31011352565024,-0.301501118270308,
4.3115924136571));
#38764=CARTESIAN_POINT('Ctrl Pts',(4.33397144368164,-0.413936097932681,
4.12903358037428));
#38765=CARTESIAN_POINT('Ctrl Pts',(4.35782936171308,-0.425152419412173,
3.91492252699502));
#38766=CARTESIAN_POINT('Ctrl Pts',(4.38168727974448,-0.332407397051365,
3.72161523052345));
#38767=CARTESIAN_POINT('Ctrl Pts',(4.40554519777592,-0.158379709595794,
3.5963805946708));
#38768=CARTESIAN_POINT('Ctrl Pts',(4.42940311580732,0.0543761300157755,
3.56984189703405));
#38769=CARTESIAN_POINT('Ctrl Pts',(4.45326103383876,0.25383552520097,3.64848857324589));
#38770=CARTESIAN_POINT('Ctrl Pts',(4.47711895187016,0.39122521984844,3.81308936806525));
#38771=CARTESIAN_POINT('Ctrl Pts',(4.50097686990159,0.432949691632991,4.02339490384879));
#38772=CARTESIAN_POINT('Ctrl Pts',(4.524834787933,0.368806170420464,4.22797974831721));
#38773=CARTESIAN_POINT('Ctrl Pts',(4.54869270596443,0.214479494504121,4.37681733431002));
#38774=CARTESIAN_POINT('Ctrl Pts',(4.57255062399584,0.00770673985495463,
4.4335128177492));
#38775=CARTESIAN_POINT('Ctrl Pts',(4.59640854202726,-0.200950522604244,
4.38420260860549));
#38776=CARTESIAN_POINT('Ctrl Pts',(4.62026646005868,-0.360469908510665,
4.24094439618412));
#38777=CARTESIAN_POINT('Ctrl Pts',(4.6441243780901,-0.431844582779732,4.03876871570463));
#38778=CARTESIAN_POINT('Ctrl Pts',(4.66798229612152,-0.397621493350665,
3.82711302819544));
#38779=CARTESIAN_POINT('Ctrl Pts',(4.69184021415294,-0.266169117804412,
3.65773291463971));
#38780=CARTESIAN_POINT('Ctrl Pts',(4.71569813218436,-0.0696311426542753,
3.57204642662242));
#38781=CARTESIAN_POINT('Ctrl Pts',(4.73955605021577,0.143933543589337,3.59100624451743));
#38782=CARTESIAN_POINT('Ctrl Pts',(4.76341396824719,0.322302557754209,3.70997617639404));
#38783=CARTESIAN_POINT('Ctrl Pts',(4.78727188627862,0.421859817202848,3.8998648332327));
#38784=CARTESIAN_POINT('Ctrl Pts',(4.81112980431003,0.41826086011465,4.11423926597311));
#38785=CARTESIAN_POINT('Ctrl Pts',(4.83498772234146,0.312385729531365,4.30067908636799));
#38786=CARTESIAN_POINT('Ctrl Pts',(4.85884564037287,0.130123778861223,4.41359467981201));
#38787=CARTESIAN_POINT('Ctrl Pts',(4.88270355840429,-0.0839569802410516,
4.42537510794913));
#38788=CARTESIAN_POINT('Ctrl Pts',(4.90656147643571,-0.277507970732168,
4.33313973520738));
#38789=CARTESIAN_POINT('Ctrl Pts',(4.93041939446713,-0.403200703213916,
4.15944262266324));
#38790=CARTESIAN_POINT('Ctrl Pts',(4.95427731249855,-0.430299880793222,
3.94675744574809));
#38791=CARTESIAN_POINT('Ctrl Pts',(4.97813523052996,-0.352179016385168,
3.7470915236456));
#38792=CARTESIAN_POINT('Ctrl Pts',(5.00199314856139,-0.187940789307144,
3.60926861310034));
#38793=CARTESIAN_POINT('Ctrl Pts',(5.0258510665928,0.0222540801607904,3.56699016996131));
#38794=CARTESIAN_POINT('Ctrl Pts',(5.04970898462423,0.227007220840439,3.63059442521772));
#38795=CARTESIAN_POINT('Ctrl Pts',(5.07356690265564,0.376250912472057,3.7845284059142));
#38796=CARTESIAN_POINT('Ctrl Pts',(5.09742482068706,0.433491007135177,3.99115106069306));
#38797=CARTESIAN_POINT('Ctrl Pts',(5.12128273871848,0.384730742495793,4.19993752217271));
#38798=CARTESIAN_POINT('Ctrl Pts',(5.1451406567499,0.241893331461176,4.35983381329239));
#38799=CARTESIAN_POINT('Ctrl Pts',(5.16899857478132,0.0399064118422473,
4.43174093538579));
#38800=CARTESIAN_POINT('Ctrl Pts',(5.19285649281273,-0.171838712500945,
4.39807563839043));
#38801=CARTESIAN_POINT('Ctrl Pts',(5.21671441084416,-0.341564590845109,
4.26707000444592));
#38802=CARTESIAN_POINT('Ctrl Pts',(5.24057232887557,-0.427768622694993,
4.07075847957352));
#38803=CARTESIAN_POINT('Ctrl Pts',(5.264430246907,-0.409371574112622,3.85714457902312));
#38804=CARTESIAN_POINT('Ctrl Pts',(5.2882881649384,-0.290872024601924,3.6784627202051));
#38805=CARTESIAN_POINT('Ctrl Pts',(5.31214608296984,-0.101246341881189,
3.57840548479658));
#38806=CARTESIAN_POINT('Ctrl Pts',(5.33600400100125,0.113136829324483,3.58143959235932));
#38807=CARTESIAN_POINT('Ctrl Pts',(5.35986191903268,0.299854963974951,3.68682312094679));
#38808=CARTESIAN_POINT('Ctrl Pts',(5.38371983706408,0.413250392048343,3.8687869272297));
#38809=CARTESIAN_POINT('Ctrl Pts',(5.40757775509551,0.425594842551202,4.08283590397723));
#38810=CARTESIAN_POINT('Ctrl Pts',(5.43143567312693,0.333869761079625,4.27662924579771));
#38811=CARTESIAN_POINT('Ctrl Pts',(5.45529359115834,0.160504428594232,4.4027792017911));
#38812=CARTESIAN_POINT('Ctrl Pts',(5.47915150918977,-0.0521086087350157,
4.43043867146175));
#38813=CARTESIAN_POINT('Ctrl Pts',(5.50300942722118,-0.251979671819092,
4.35284416104532));
#38814=CARTESIAN_POINT('Ctrl Pts',(5.52686734525261,-0.390234841353927,
4.18896964197264));
#38815=CARTESIAN_POINT('Ctrl Pts',(5.55072526328402,-0.433066962396004,
3.97888689800548));
#38816=CARTESIAN_POINT('Ctrl Pts',(5.57458318131544,-0.370002414621403,
3.77396688259));
#38817=CARTESIAN_POINT('Ctrl Pts',(5.59844109934686,-0.21646219781534,3.62431812139094));
#38818=CARTESIAN_POINT('Ctrl Pts',(5.62229901737828,-0.00999107731853999,
3.56653381289738));
#38819=CARTESIAN_POINT('Ctrl Pts',(5.64615693540971,0.198923133709572,3.61474379450078));
#38820=CARTESIAN_POINT('Ctrl Pts',(5.67001485344111,0.359195220034686,3.75715941257656));
#38821=CARTESIAN_POINT('Ctrl Pts',(5.69387277147254,0.431634290692432,3.95895616900985));
#38822=CARTESIAN_POINT('Ctrl Pts',(5.71773068950395,0.398527019959163,4.1707892603438));
#38823=CARTESIAN_POINT('Ctrl Pts',(5.74158860753538,0.267969036875697,4.34085972491723));
#38824=CARTESIAN_POINT('Ctrl Pts',(5.76544652556679,0.0718853255354575,
4.42758070267197));
#38825=CARTESIAN_POINT('Ctrl Pts',(5.78930444359821,-0.141776307127955,
4.40974655013133));
#38826=CARTESIAN_POINT('Ctrl Pts',(5.81316236162963,-0.320769768688322,
4.29171820750724));
#38827=CARTESIAN_POINT('Ctrl Pts',(5.83702027966105,-0.421326288178809,
4.10235681181338));
#38828=CARTESIAN_POINT('Ctrl Pts',(5.86087819769247,-0.418857046020503,
3.88796639709818));
#38829=CARTESIAN_POINT('Ctrl Pts',(5.88473611572389,-0.313965860818636,
3.70097123187977));
#38830=CARTESIAN_POINT('Ctrl Pts',(5.90859403375531,-0.132301443679057,
3.58709678011166));
#38831=CARTESIAN_POINT('Ctrl Pts',(5.93245195178673,0.0817142298265842,
3.57418834816524));
#38832=CARTESIAN_POINT('Ctrl Pts',(5.95630986981814,0.275748643515392,3.66540258613358));
#38833=CARTESIAN_POINT('Ctrl Pts',(5.98016778784957,0.402354822815078,3.83843477537114));
#38834=CARTESIAN_POINT('Ctrl Pts',(6.00402570588098,0.430574627524036,4.05097449853386));
#38835=CARTESIAN_POINT('Ctrl Pts',(6.02788362391241,0.353506566116634,4.25104874587108));
#38836=CARTESIAN_POINT('Ctrl Pts',(6.05174154194382,0.189997730437525,4.38973628930191));
#38837=CARTESIAN_POINT('Ctrl Pts',(6.07559945997525,-0.0199730113800777,
4.43311976162365));
#38838=CARTESIAN_POINT('Ctrl Pts',(6.09945737800665,-0.2250554921608,4.3705991908187));
#38839=CARTESIAN_POINT('Ctrl Pts',(6.12331529603809,-0.375113923638194,
4.21744656883549));
#38840=CARTESIAN_POINT('Ctrl Pts',(6.1471732140695,-0.433431396087355,4.01114207710762));
#38841=CARTESIAN_POINT('Ctrl Pts',(6.17103113210093,-0.385792139046387,
3.80207577201042));
#38842=CARTESIAN_POINT('Ctrl Pts',(6.19488905013233,-0.243761337718234,
3.64147770828707));
#38843=CARTESIAN_POINT('Ctrl Pts',(6.21874696816376,-0.042227823444436,
3.56841523311022));
#38844=CARTESIAN_POINT('Ctrl Pts',(6.24260488619517,0.16982704650124,3.60113783246665));
#38845=CARTESIAN_POINT('Ctrl Pts',(6.2664628042266,0.339985970990829,3.73091992247201));
#38846=CARTESIAN_POINT('Ctrl Pts',(6.29032072225801,0.427700638223926,3.92738904240251));
#38847=CARTESIAN_POINT('Ctrl Pts',(6.31417864028943,0.409561128158778,4.13996490148311));
#38848=CARTESIAN_POINT('Ctrl Pts',(6.34598919766466,0.254661277208374,4.38159318714805));
#38849=CARTESIAN_POINT('Ctrl Pts',(6.38575239438369,-0.125272905304917,
4.47558432627151));
#38850=CARTESIAN_POINT('Ctrl Pts',(6.43346823044653,-0.468271923807345,
4.15124960425567));
#38851=CARTESIAN_POINT('Ctrl Pts',(6.48118406650937,-0.380227249479543,
3.6882349865083));
#38852=CARTESIAN_POINT('Ctrl Pts',(6.52889990257221,0.0564566449812287,
3.51140415777354));
#38853=CARTESIAN_POINT('Ctrl Pts',(6.57661573863504,0.441574375138847,3.78331933667001));
#38854=CARTESIAN_POINT('Ctrl Pts',(6.62433157469789,0.421040068198854,4.25418342072721));
#38855=CARTESIAN_POINT('Ctrl Pts',(6.67204741076071,0.0139362792425842,
4.49164405688148));
#38856=CARTESIAN_POINT('Ctrl Pts',(6.71976324682356,-0.406006764042365,
4.27761133505345));
#38857=CARTESIAN_POINT('Ctrl Pts',(6.76747908288639,-0.453085647428837,
3.80864864857145));
#38858=CARTESIAN_POINT('Ctrl Pts',(6.81519491894923,-0.0841006081168706,
3.51540431248109));
#38859=CARTESIAN_POINT('Ctrl Pts',(6.86291075501207,0.362121456530253,3.66717299786736));
#38860=CARTESIAN_POINT('Ctrl Pts',(6.91062659107491,0.475798562415156,4.124581128109));
#38861=CARTESIAN_POINT('Ctrl Pts',(6.95834242713775,0.152544250279933,4.46758486877347));
#38862=CARTESIAN_POINT('Ctrl Pts',(7.00605826320058,-0.310794706562241,
4.38119802990972));
#38863=CARTESIAN_POINT('Ctrl Pts',(7.05377409926342,-0.488725618924084,
3.94475128051735));
#38864=CARTESIAN_POINT('Ctrl Pts',(7.10148993532626,-0.21785253135038,3.55904022429238));
#38865=CARTESIAN_POINT('Ctrl Pts',(7.14920577138909,0.253078023397415,3.57826934481931));
#38866=CARTESIAN_POINT('Ctrl Pts',(7.19692160745195,0.491603063369337,3.98478019943955));
#38867=CARTESIAN_POINT('Ctrl Pts',(7.24463744351477,0.278681483980911,4.40526763942622));
#38868=CARTESIAN_POINT('Ctrl Pts',(7.29235327957762,-0.190157610347023,
4.45359156587464));
#38869=CARTESIAN_POINT('Ctrl Pts',(7.34006911564044,-0.484372034479295,
4.08537538031203));
#38870=CARTESIAN_POINT('Ctrl Pts',(7.3877849517033,-0.333780171974684,3.63875766810317));
#38871=CARTESIAN_POINT('Ctrl Pts',(7.43550078776612,0.123327161313159,3.52387434835784));
#38872=CARTESIAN_POINT('Ctrl Pts',(7.48321662382897,0.467181263150904,3.84622454030349));
#38873=CARTESIAN_POINT('Ctrl Pts',(7.5309324598918,0.382015623368301,4.30978910321172));
#38874=CARTESIAN_POINT('Ctrl Pts',(7.57864829595465,-0.0539608418635878,
4.4888695658253));
#38875=CARTESIAN_POINT('Ctrl Pts',(7.62636413201748,-0.440384235482588,
4.21901358396786));
#38876=CARTESIAN_POINT('Ctrl Pts',(7.67407996808031,-0.422396009600076,
3.7480340579683));
#38877=CARTESIAN_POINT('Ctrl Pts',(7.72179580414317,-0.0165150286377962,
3.50843873354525));
#38878=CARTESIAN_POINT('Ctrl Pts',(7.76951164020598,0.404531957204003,3.72025168374225));
#38879=CARTESIAN_POINT('Ctrl Pts',(7.81722747626884,0.454091022239626,4.18896181724392));
#38880=CARTESIAN_POINT('Ctrl Pts',(7.86494331233166,0.0866513144543145,
4.48414540641706));
#38881=CARTESIAN_POINT('Ctrl Pts',(7.91265914839452,-0.360361628691054,
4.33473081934393));
#38882=CARTESIAN_POINT('Ctrl Pts',(7.96037498445733,-0.476448943335793,
3.87792777037096));
#38883=CARTESIAN_POINT('Ctrl Pts',(8.0080908205202,-0.1550058622045,3.53322552818936));
#38884=CARTESIAN_POINT('Ctrl Pts',(8.05580665658301,0.308781487260178,3.61716946571973));
#38885=CARTESIAN_POINT('Ctrl Pts',(8.10352249264587,0.489010045760349,4.0526725734847));
#38886=CARTESIAN_POINT('Ctrl Pts',(8.1512383287087,0.220173154851853,4.43980564654689));
#38887=CARTESIAN_POINT('Ctrl Pts',(8.19895416477154,-0.250852131956433,
4.4230584271054));
#38888=CARTESIAN_POINT('Ctrl Pts',(8.24667000083438,-0.491516046133,4.01781014446235));
#38889=CARTESIAN_POINT('Ctrl Pts',(8.29438583689722,-0.280813212199106,
3.59620653211525));
#38890=CARTESIAN_POINT('Ctrl Pts',(8.34210167296004,0.187764715363875,3.54541267448783));
#38891=CARTESIAN_POINT('Ctrl Pts',(8.38981750902289,0.483915415676709,3.91207335260334));
#38892=CARTESIAN_POINT('Ctrl Pts',(8.43753334508573,0.335679143777854,4.35947842394856));
#38893=CARTESIAN_POINT('Ctrl Pts',(8.48524918114857,-0.120816450939738,
4.4767689272953));
#38894=CARTESIAN_POINT('Ctrl Pts',(8.5329650172114,-0.466364439759318,4.15623518867385));
#38895=CARTESIAN_POINT('Ctrl Pts',(8.58068085327425,-0.383642787608637,
3.69222827230584));
#38896=CARTESIAN_POINT('Ctrl Pts',(8.62839668933707,0.0513839395061145,
3.51085286915611));
#38897=CARTESIAN_POINT('Ctrl Pts',(8.67611252539993,0.439224004328866,3.77866880275638));
#38898=CARTESIAN_POINT('Ctrl Pts',(8.72382836146275,0.42371790764641,4.24973658040369));
#38899=CARTESIAN_POINT('Ctrl Pts',(8.7715441975256,0.0191051366342138,4.49146741357506));
#38900=CARTESIAN_POINT('Ctrl Pts',(8.81926003358843,-0.403052175319494,
4.28187615866228));
#38901=CARTESIAN_POINT('Ctrl Pts',(8.86697586965126,-0.455080472922433,
3.81343369002772));
#38902=CARTESIAN_POINT('Ctrl Pts',(8.91469170571412,-0.0892013699275644,
3.51631793453238));
#38903=CARTESIAN_POINT('Ctrl Pts',(8.96240754177693,0.358592723611288,3.66337486216116));
#38904=CARTESIAN_POINT('Ctrl Pts',(9.0101233778398,0.477085601399612,4.11955983351088));
#38905=CARTESIAN_POINT('Ctrl Pts',(9.05783921390261,0.157463430517111,4.46595117008304));
#38906=CARTESIAN_POINT('Ctrl Pts',(9.10555504996547,-0.306759831495564,
4.38445237758765));
#38907=CARTESIAN_POINT('Ctrl Pts',(9.1532708860283,-0.489280820139143,3.94990505119329));
#38908=CARTESIAN_POINT('Ctrl Pts',(9.20098672209113,-0.222487703095825,
3.56136068709803));
#38909=CARTESIAN_POINT('Ctrl Pts',(9.24870255815399,0.248619295113741,3.57562555337399));
#38910=CARTESIAN_POINT('Ctrl Pts',(9.29641839421681,0.49141536912078,3.97960000382683));
#38911=CARTESIAN_POINT('Ctrl Pts',(9.34413423027966,0.282937148266828,4.40230808465976));
#38912=CARTESIAN_POINT('Ctrl Pts',(9.39185006634249,-0.185366609388173,
4.45557046104408));
#38913=CARTESIAN_POINT('Ctrl Pts',(9.43956590240532,-0.483445357410111,
4.09047547319903));
#38914=CARTESIAN_POINT('Ctrl Pts',(9.48728173846818,-0.337568794959357,
3.64229546617122));
#38915=CARTESIAN_POINT('Ctrl Pts',(9.53499757453099,0.118302386066128,3.5226010365501));
#38916=CARTESIAN_POINT('Ctrl Pts',(9.58271341059386,0.465534665650901,3.84130942079228));
#38917=CARTESIAN_POINT('Ctrl Pts',(9.63042924665667,0.385259298596883,4.30574580568933));
#38918=CARTESIAN_POINT('Ctrl Pts',(9.67814508271952,-0.0488056103349303,
4.48941111271794));
#38919=CARTESIAN_POINT('Ctrl Pts',(9.72586091878235,-0.438051576325333,
4.22364266437974));
#38920=CARTESIAN_POINT('Ctrl Pts',(9.77357675484519,-0.425028039486299,
3.75249971615691));
#38921=CARTESIAN_POINT('Ctrl Pts',(9.82129259090803,-0.0216947140899849,
3.50864008686857));
#38922=CARTESIAN_POINT('Ctrl Pts',(9.86900842697087,0.401561201071248,3.7160038263529));
#38923=CARTESIAN_POINT('Ctrl Pts',(9.91672426303371,0.456057286475463,4.18416562194019));
#38924=CARTESIAN_POINT('Ctrl Pts',(9.96444009909655,0.0917489483659128,
4.48320529314746));
#38925=CARTESIAN_POINT('Ctrl Pts',(10.0121559351594,-0.356813860767086,
4.3385101085883));
#38926=CARTESIAN_POINT('Ctrl Pts',(10.0598717712222,-0.477709011270712,
3.88295588266498));
#38927=CARTESIAN_POINT('Ctrl Pts',(10.1075876072851,-0.159916626226494,
3.53488507064564));
#38928=CARTESIAN_POINT('Ctrl Pts',(10.1553034433479,0.304729657315094,3.61393645496551));
#38929=CARTESIAN_POINT('Ctrl Pts',(10.2030192794107,0.489538007675758,4.04751593304174));
#38930=CARTESIAN_POINT('Ctrl Pts',(10.2507351154736,0.224796073077312,4.43746079867915));
#38931=CARTESIAN_POINT('Ctrl Pts',(10.2984509515364,-0.246379554360218,
4.42567868168988));
#38932=CARTESIAN_POINT('Ctrl Pts',(10.3461667875993,-0.491301045992024,
4.02298928139638));
#38933=CARTESIAN_POINT('Ctrl Pts',(10.3938826236621,-0.285053227451061,
3.599188470261));
#38934=CARTESIAN_POINT('Ctrl Pts',(10.4415984597249,0.182963355965895,3.54345905416307));
#38935=CARTESIAN_POINT('Ctrl Pts',(10.4893142957878,0.482961874346273,3.9069782134126));
#38936=CARTESIAN_POINT('Ctrl Pts',(10.5370301318506,0.339449072190825,4.35592071060949));
#38937=CARTESIAN_POINT('Ctrl Pts',(10.5847459679134,-0.115785036052801,
4.47801574270962));
#38938=CARTESIAN_POINT('Ctrl Pts',(10.6324618039763,-0.464691964107356,
4.16114156306187));
#38939=CARTESIAN_POINT('Ctrl Pts',(10.6801776400391,-0.386865111317189,
3.69628860657276));
#38940=CARTESIAN_POINT('Ctrl Pts',(10.7278934761019,0.0462259258804368,
3.51033849586834));
#38941=CARTESIAN_POINT('Ctrl Pts',(10.7756093121648,0.436866984064762,3.77405207881873));
#38942=CARTESIAN_POINT('Ctrl Pts',(10.8233251482276,0.426326368719826,4.24525711444552));
#38943=CARTESIAN_POINT('Ctrl Pts',(10.8710409842905,0.0242836891050981,
4.49123876811122));
#38944=CARTESIAN_POINT('Ctrl Pts',(10.9187568203533,-0.400059075867425,
4.28610830234036));
#38945=CARTESIAN_POINT('Ctrl Pts',(10.9664726564161,-0.45702143577077,3.81824018018824));
#38946=CARTESIAN_POINT('Ctrl Pts',(11.014188492479,-0.0942939790271268,
3.51728489730359));
#38947=CARTESIAN_POINT('Ctrl Pts',(11.0619043285418,0.355025089556487,3.65961432075161));
#38948=CARTESIAN_POINT('Ctrl Pts',(11.1096201646047,0.478319155637209,4.11452515096033));
#38949=CARTESIAN_POINT('Ctrl Pts',(11.1573360006675,0.16236538121005,4.46426577284621));
#38950=CARTESIAN_POINT('Ctrl Pts',(11.2050518367304,-0.302691021094817,
4.38766399188028));
#38951=CARTESIAN_POINT('Ctrl Pts',(11.2527676727932,-0.489781601228288,
3.95506440219344));
#38952=CARTESIAN_POINT('Ctrl Pts',(11.300483508856,-0.227098200695192,3.56372986339542));
#38953=CARTESIAN_POINT('Ctrl Pts',(11.3481993449188,0.244132971891272,3.57302890392028));
#38954=CARTESIAN_POINT('Ctrl Pts',(11.3959151809817,0.491173079921361,3.97442207176994));
#38955=CARTESIAN_POINT('Ctrl Pts',(11.4436310170445,0.287161390990383,4.39930384468027));
#38956=CARTESIAN_POINT('Ctrl Pts',(11.4913468531074,-0.180555021833016,
4.45749875294131));
#38957=CARTESIAN_POINT('Ctrl Pts',(11.5390626891702,-0.482464979911041,
4.09556551685319));
#38958=CARTESIAN_POINT('Ctrl Pts',(11.586778525233,-0.341319923258817,3.64587299617429));
#38959=CARTESIAN_POINT('Ctrl Pts',(11.6344943612959,0.113264470804062,3.5213807520529));
#38960=CARTESIAN_POINT('Ctrl Pts',(11.6822101973587,0.463836358529674,3.83641192782507));
#38961=CARTESIAN_POINT('Ctrl Pts',(11.7299260334216,0.38846018117773,4.30166854740152));
#38962=CARTESIAN_POINT('Ctrl Pts',(11.7776418694844,-0.0436449577779122,
4.48989829813191));
#38963=CARTESIAN_POINT('Ctrl Pts',(11.8253577055472,-0.435670260442099,
4.22824690363353));
#38964=CARTESIAN_POINT('Ctrl Pts',(11.8730735416101,-0.427612859293677,
3.75699286549843));
#38965=CARTESIAN_POINT('Ctrl Pts',(11.9207893776729,-0.0268719897862959,
3.50889601812151));
#38966=CARTESIAN_POINT('Ctrl Pts',(11.9685052137357,0.398545841420554,3.71178751390968));
#38967=CARTESIAN_POINT('Ctrl Pts',(12.0162210497986,0.457972894034889,4.17934897039372));
#38968=CARTESIAN_POINT('Ctrl Pts',(12.0639368858614,0.0968363912382316,
4.48221150772657));
#38969=CARTESIAN_POINT('Ctrl Pts',(12.1116527219243,-0.353226459651896,
4.34225179773635));
#38970=CARTESIAN_POINT('Ctrl Pts',(12.1593685579871,-0.478916017555994,
3.88799699566402));
#38971=CARTESIAN_POINT('Ctrl Pts',(12.2070843940499,-0.164809627468288,
3.53659627586117));
#38972=CARTESIAN_POINT('Ctrl Pts',(12.2548002301128,0.300643979445627,3.61074632631782));
#38973=CARTESIAN_POINT('Ctrl Pts',(12.3025160661756,0.490011594032383,4.04235401475446));
#38974=CARTESIAN_POINT('Ctrl Pts',(12.3502319022385,0.229394022021679,4.43506735974179));
#38975=CARTESIAN_POINT('Ctrl Pts',(12.3979477383013,-0.241879610092261,
4.42825165390643));
#38976=CARTESIAN_POINT('Ctrl Pts',(12.4456635743641,-0.491031474462283,
4.0281658647901));
#38977=CARTESIAN_POINT('Ctrl Pts',(12.493379410427,-0.289261580343189,3.60221492864948));
#38978=CARTESIAN_POINT('Ctrl Pts',(12.5410952464898,0.178141673866572,3.54155614424011));
#38979=CARTESIAN_POINT('Ctrl Pts',(12.5888110825527,0.481954687902679,3.90189340664049));
#38980=CARTESIAN_POINT('Ctrl Pts',(12.6365269186155,0.343181296211668,4.35232346328687));
#38981=CARTESIAN_POINT('Ctrl Pts',(12.6842427546783,-0.110740760313508,
4.47920946240362));
#38982=CARTESIAN_POINT('Ctrl Pts',(12.7319585907412,-0.462967872677167,
4.16603003860975));
#38983=CARTESIAN_POINT('Ctrl Pts',(12.779674426804,-0.390044463885,3.70038267566003));
#38984=CARTESIAN_POINT('Ctrl Pts',(12.8273902628668,0.0410627776982723,
3.50987851185683));
#38985=CARTESIAN_POINT('Ctrl Pts',(12.8751060989297,0.434461438689172,3.76946045210395));
#38986=CARTESIAN_POINT('Ctrl Pts',(12.9228219349925,0.42888747548329,4.24075040649094));
#38987=CARTESIAN_POINT('Ctrl Pts',(12.9705377710553,0.0294595442590321,
4.49095555817611));
#38988=CARTESIAN_POINT('Ctrl Pts',(13.0182536071182,-0.397021539751646,
4.29030866646591));
#38989=CARTESIAN_POINT('Ctrl Pts',(13.065969443181,-0.458911634846768,3.82306685936703));
#38990=CARTESIAN_POINT('Ctrl Pts',(13.1136852792439,-0.0993761143989603,
3.51830547777773));
#38991=CARTESIAN_POINT('Ctrl Pts',(13.1614011153067,0.351418020999476,3.65589158776806));
#38992=CARTESIAN_POINT('Ctrl Pts',(13.2091169513695,0.479499580452807,4.10947774749948));
#38993=CARTESIAN_POINT('Ctrl Pts',(13.2568327874324,0.167249297126924,4.46252880717046));
#38994=CARTESIAN_POINT('Ctrl Pts',(13.3045486234952,-0.298588589211839,
4.39083254629632));
#38995=CARTESIAN_POINT('Ctrl Pts',(13.352264459558,-0.490227979701372,3.96022874442655));
#38996=CARTESIAN_POINT('Ctrl Pts',(13.3999802956209,-0.23168347330409,3.56614749850931));
#38997=CARTESIAN_POINT('Ctrl Pts',(13.4476961316837,0.239619531536799,3.57047968038978));
#38998=CARTESIAN_POINT('Ctrl Pts',(13.4954119677466,0.490876233547033,3.96924698078795));
#38999=CARTESIAN_POINT('Ctrl Pts',(13.5431278038094,0.291353737189313,4.39625525192456));
#39000=CARTESIAN_POINT('Ctrl Pts',(13.5908436398722,-0.175723379082843,
4.45937622804808));
#39001=CARTESIAN_POINT('Ctrl Pts',(13.6385594759351,-0.481431012491488,
4.10064494554323));
#39002=CARTESIAN_POINT('Ctrl Pts',(13.6862753119979,-0.345033139360895,
3.64948986092447));
#39003=CARTESIAN_POINT('Ctrl Pts',(13.7339911480608,0.108213974662067,3.52021363031051));
#39004=CARTESIAN_POINT('Ctrl Pts',(13.7817069841236,0.462086530666827,3.83153260544464));
#39005=CARTESIAN_POINT('Ctrl Pts',(13.8294228201864,0.391617915445045,4.297557781203));
#39006=CARTESIAN_POINT('Ctrl Pts',(13.8771386562493,-0.0384794573460961,
4.49033106796769));
#39007=CARTESIAN_POINT('Ctrl Pts',(13.9248544923121,-0.433240552373761,
4.23282579030437));
#39008=CARTESIAN_POINT('Ctrl Pts',(13.9725703283749,-0.430150181893835,
3.76151300691929));
#39009=CARTESIAN_POINT('Ctrl Pts',(14.0202861644378,-0.032046280669499,
3.50920649887429));
#39010=CARTESIAN_POINT('Ctrl Pts',(14.0680020005006,0.39548621318905,3.70760321474174));
#39011=CARTESIAN_POINT('Ctrl Pts',(14.1157178365634,0.459837632138507,4.1745123976147));
#39012=CARTESIAN_POINT('Ctrl Pts',(14.1634336726263,0.101913077983734,4.48116416053968));
#39013=CARTESIAN_POINT('Ctrl Pts',(14.2111495086891,-0.349599823817769,
4.34595547117883));
#39014=CARTESIAN_POINT('Ctrl Pts',(14.258865344752,-0.480069828122688,3.8930505494253));
#39015=CARTESIAN_POINT('Ctrl Pts',(14.3065811808148,-0.169684322438749,
3.53835895376334));
#39016=CARTESIAN_POINT('Ctrl Pts',(14.3542970168777,0.296524907469595,3.60759943412104));
#39017=CARTESIAN_POINT('Ctrl Pts',(14.4020128529405,0.49043075222644,4.0371873919842));
#39018=CARTESIAN_POINT('Ctrl Pts',(14.4497286890033,0.233966490966644,4.43262559558668));
#39019=CARTESIAN_POINT('Ctrl Pts',(14.4974445250662,-0.237352798985028,
4.43077705796148));
#39020=CARTESIAN_POINT('Ctrl Pts',(14.545160361129,-0.490707361486496,4.03333931965322));
#39021=CARTESIAN_POINT('Ctrl Pts',(14.5928761971918,-0.293437803431633,
3.60528557111603));
#39022=CARTESIAN_POINT('Ctrl Pts',(14.6405920332547,0.173300204635467,3.53970415608515));
#39023=CARTESIAN_POINT('Ctrl Pts',(14.6883078693175,0.480893968219416,3.89681949708321));
#39024=CARTESIAN_POINT('Ctrl Pts',(14.7360237053804,0.346875401282657,4.34868708154587));
#39025=CARTESIAN_POINT('Ctrl Pts',(14.7837395414432,-0.10568418401607,4.48034995378457));
#39026=CARTESIAN_POINT('Ctrl Pts',(14.831455377506,-0.461192356972643,4.17090007232882));
#39027=CARTESIAN_POINT('Ctrl Pts',(14.8791712135689,-0.393180492164677,
3.7045100248179));
#39028=CARTESIAN_POINT('Ctrl Pts',(14.9268870496317,0.0358950684576197,
3.50947296821438));
#39029=CARTESIAN_POINT('Ctrl Pts',(14.9746028856945,0.432007635398663,3.76489443262817));
#39030=CARTESIAN_POINT('Ctrl Pts',(15.0223187217574,0.431400943461215,4.23621695712364));
#39031=CARTESIAN_POINT('Ctrl Pts',(15.0700345578202,0.0346321271865876,
4.4906178152274));
#39032=CARTESIAN_POINT('Ctrl Pts',(15.1177503938831,-0.393939904367254,
4.2944767844824));
#39033=CARTESIAN_POINT('Ctrl Pts',(15.1654662299459,-0.46075086019608,3.82791319143947));
#39034=CARTESIAN_POINT('Ctrl Pts',(15.2131820660087,-0.104447211543591,
3.51937956259357));
#39035=CARTESIAN_POINT('Ctrl Pts',(15.2608979020716,0.347771918596306,3.652207076714));
#39036=CARTESIAN_POINT('Ctrl Pts',(15.3086137381344,0.480626744730421,4.10441818376995));
#39037=CARTESIAN_POINT('Ctrl Pts',(15.3563295741973,0.172114635785536,4.46074046598969));
#39038=CARTESIAN_POINT('Ctrl Pts',(15.4040454102601,-0.294452991525291,
4.39395768888776));
#39039=CARTESIAN_POINT('Ctrl Pts',(15.4517612463229,-0.490619905976795,
3.96539750426199));
#39040=CARTESIAN_POINT('Ctrl Pts',(15.4994770823858,-0.236243011612202,
3.56861332390027));
#39041=CARTESIAN_POINT('Ctrl Pts',(15.5471929184486,0.235079475381852,3.56797816593814));
#39042=CARTESIAN_POINT('Ctrl Pts',(15.5949087545115,0.490524862970081,3.9640753057054));
#39043=CARTESIAN_POINT('Ctrl Pts',(15.6426245905743,0.295513721197704,4.39316264501585));
#39044=CARTESIAN_POINT('Ctrl Pts',(15.6903404266371,-0.170872217813597,
4.46120267782338));
#39045=CARTESIAN_POINT('Ctrl Pts',(15.7380562626999,-0.480343569999647,
4.1057131950703));
#39046=CARTESIAN_POINT('Ctrl Pts',(15.7857720987628,-0.348708030819167,
3.6531456586776));
#39047=CARTESIAN_POINT('Ctrl Pts',(15.8334879348256,0.103151458625294,3.5190998009613));
#39048=CARTESIAN_POINT('Ctrl Pts',(15.8812037708885,0.460285376424935,3.82667199562295));
#39049=CARTESIAN_POINT('Ctrl Pts',(15.9289196069513,0.39473215065269,4.29341396369818));
#39050=CARTESIAN_POINT('Ctrl Pts',(15.9766354430142,-0.033309682798763,
4.49070937415524));
#39051=CARTESIAN_POINT('Ctrl Pts',(16.024351279077,-0.430762722000766,4.23737881579128));
#39052=CARTESIAN_POINT('Ctrl Pts',(16.0720671151398,-0.432639725453012,
3.76605963834362));
#39053=CARTESIAN_POINT('Ctrl Pts',(16.1197829512026,-0.0372170120039125,
3.50957149464017));
#39054=CARTESIAN_POINT('Ctrl Pts',(16.1674987872655,0.392382656225717,3.70345139362117));
#39055=CARTESIAN_POINT('Ctrl Pts',(16.2152146233283,0.461651293660056,4.16965644082667));
#39056=CARTESIAN_POINT('Ctrl Pts',(16.2629304593912,0.106978444708158,4.48006336792116));
#39057=CARTESIAN_POINT('Ctrl Pts',(16.310646295454,-0.345934356094203,4.34962071752925));
#39058=CARTESIAN_POINT('Ctrl Pts',(16.3583621315169,-0.481170314810987,
3.89811598262401));
#39059=CARTESIAN_POINT('Ctrl Pts',(16.4060779675797,-0.174540169679895,
3.54017290856226));
#39060=CARTESIAN_POINT('Ctrl Pts',(16.4537938036425,0.292372898913969,3.60449612791703));
#39061=CARTESIAN_POINT('Ctrl Pts',(16.5015096397054,0.490795435699827,4.0320166386149));
#39062=CARTESIAN_POINT('Ctrl Pts',(16.5492254757682,0.238512972024049,4.4301357774334));
#39063=CARTESIAN_POINT('Ctrl Pts',(16.596941311831,-0.23279962385521,4.43325461334514));
#39064=CARTESIAN_POINT('Ctrl Pts',(16.6446571478939,-0.490328743065594,
4.03850907134293));
#39065=CARTESIAN_POINT('Ctrl Pts',(16.6923729839567,-0.297581432841348,
3.60840005658827));
#39066=CARTESIAN_POINT('Ctrl Pts',(16.7400888200196,0.168439486040012,3.53790329540825));
#39067=CARTESIAN_POINT('Ctrl Pts',(16.7878046560824,0.479779833116189,3.89175704832657));
#39068=CARTESIAN_POINT('Ctrl Pts',(16.8355204921452,0.350530977080134,4.3450119692985));
#39069=CARTESIAN_POINT('Ctrl Pts',(16.8832363282081,-0.100615868820984,
4.4814370901721));
#39070=CARTESIAN_POINT('Ctrl Pts',(16.9309521642709,-0.459365614209645,
4.17575112327883));
#39071=CARTESIAN_POINT('Ctrl Pts',(16.9786680003337,-0.396272847821079,
3.70867019559999));
#39072=CARTESIAN_POINT('Ctrl Pts',(17.0263838363966,0.0307233721630972,
3.5091219099869));
#39073=CARTESIAN_POINT('Ctrl Pts',(17.0740996724594,0.429505846750062,3.76035452756312));
#39074=CARTESIAN_POINT('Ctrl Pts',(17.1218155085223,0.433866493469502,4.23165726989771));
#39075=CARTESIAN_POINT('Ctrl Pts',(17.1695313445851,0.039800863341802,4.49022557677993));
#39076=CARTESIAN_POINT('Ctrl Pts',(17.217247180648,-0.390814512007675,4.29861219341511));
#39077=CARTESIAN_POINT('Ctrl Pts',(17.2649630167107,-0.462538907526291,
3.83277863809798));
#39078=CARTESIAN_POINT('Ctrl Pts',(17.3126788527736,-0.109506707187599,
3.52050703244687));
#39079=CARTESIAN_POINT('Ctrl Pts',(17.3603946888365,0.344087187338735,3.64856119684745));
#39080=CARTESIAN_POINT('Ctrl Pts',(17.4081105248993,0.481700523269991,4.09934702176407));
#39081=CARTESIAN_POINT('Ctrl Pts',(17.4558263609621,0.176960856767158,4.45890094794434));
#39082=CARTESIAN_POINT('Ctrl Pts',(17.503542197025,-0.290284687397741,4.39703907252861));
#39083=CARTESIAN_POINT('Ctrl Pts',(17.5512580330878,-0.490957336521241,
3.97057010757845));
#39084=CARTESIAN_POINT('Ctrl Pts',(17.5989738691507,-0.240776309167652,
3.57112706567612));
#39085=CARTESIAN_POINT('Ctrl Pts',(17.6466897052135,0.230513307714322,3.56552463842171));
#39086=CARTESIAN_POINT('Ctrl Pts',(17.6944055412763,0.490119007219086,3.95890762096741));
#39087=CARTESIAN_POINT('Ctrl Pts',(17.7421213773392,0.299640880944266,4.39002636746625));
#39088=CARTESIAN_POINT('Ctrl Pts',(17.789837213402,-0.166002076869247,4.46297789939377));
#39089=CARTESIAN_POINT('Ctrl Pts',(17.8375530494648,-0.479202773223469,
4.11076970247734));
#39090=CARTESIAN_POINT('Ctrl Pts',(17.8852688855277,-0.352344189444135,
3.65683998336499));
#39091=CARTESIAN_POINT('Ctrl Pts',(17.9329847215905,0.0980774850139738,
3.51803938772416));
#39092=CARTESIAN_POINT('Ctrl Pts',(17.9807005576534,0.458433095867658,3.82183063825345));
#39093=CARTESIAN_POINT('Ctrl Pts',(18.0284163937162,0.397802540886209,4.28923755516265));
#39094=CARTESIAN_POINT('Ctrl Pts',(18.076132229779,-0.0281362083699241,
4.49103317467411));
#39095=CARTESIAN_POINT('Ctrl Pts',(18.1238480658419,-0.428237044548737,
4.24190547436581));
#39096=CARTESIAN_POINT('Ctrl Pts',(18.1715639019047,-0.435081213444543,
3.7706322547532));
#39097=CARTESIAN_POINT('Ctrl Pts',(18.2192797379675,-0.0423836094492617,
3.50999096487715));
#39098=CARTESIAN_POINT('Ctrl Pts',(18.2669955740304,0.389235515258945,3.69933251171255));
#39099=CARTESIAN_POINT('Ctrl Pts',(18.3147114100932,0.463413677146622,4.16478163940629));
#39100=CARTESIAN_POINT('Ctrl Pts',(18.3624272461561,0.112031928774586,4.4789092521418));
#39101=CARTESIAN_POINT('Ctrl Pts',(18.4101430822189,-0.342230463623947,
4.35324712966946));
#39102=CARTESIAN_POINT('Ctrl Pts',(18.4578589182817,-0.482217355384067,
3.90319273261591));
#39103=CARTESIAN_POINT('Ctrl Pts',(18.5055747543446,-0.179376629827252,
3.54203793877243));
#39104=CARTESIAN_POINT('Ctrl Pts',(18.5532905904074,0.288188414964166,3.60143675240633));
#39105=CARTESIAN_POINT('Ctrl Pts',(18.6010064264702,0.491105603945206,4.02684232898929));
#39106=CARTESIAN_POINT('Ctrl Pts',(18.6487222625331,0.243032960192409,4.42759818183915));
#39107=CARTESIAN_POINT('Ctrl Pts',(18.6964380985959,-0.228220590447982,
4.43568404486223));
#39108=CARTESIAN_POINT('Ctrl Pts',(18.7441539346588,-0.489895661254576,
4.0436745456279));
#39109=CARTESIAN_POINT('Ctrl Pts',(18.7918697707216,-0.301692008317894,
3.6115580391236));
#39110=CARTESIAN_POINT('Ctrl Pts',(18.8395856067845,0.163560057986223,3.53615376224111));
#39111=CARTESIAN_POINT('Ctrl Pts',(18.8873014428472,0.478612406344963,3.88670662268212));
#39112=CARTESIAN_POINT('Ctrl Pts',(18.9350172789101,0.35414761756175,4.34129853476112));
#39113=CARTESIAN_POINT('Ctrl Pts',(18.982733114973,-0.0955363776958117,
4.48247075080787));
#39114=CARTESIAN_POINT('Ctrl Pts',(19.0304489510358,-0.457487847288108,
4.18058265263639));
#39115=CARTESIAN_POINT('Ctrl Pts',(19.0781647870987,-0.399321187381313,
3.71286272589862));
#39116=CARTESIAN_POINT('Ctrl Pts',(19.1258806231614,0.0255482632835279,
3.50882537619781));
#39117=CARTESIAN_POINT('Ctrl Pts',(19.1735964592243,0.426956350589889,3.75584124112414));
#39118=CARTESIAN_POINT('Ctrl Pts',(19.2213122952871,0.436283851722622,4.22707185138688));
#39119=CARTESIAN_POINT('Ctrl Pts',(19.26902813135,0.0449651784623906,4.48977888620274));
#39120=CARTESIAN_POINT('Ctrl Pts',(19.3167439674128,-0.387645709555542,
4.3027144342981));
#39121=CARTESIAN_POINT('Ctrl Pts',(19.3644598034757,-0.464275578741542,
3.8376626582024));
#39122=CARTESIAN_POINT('Ctrl Pts',(19.4121756395385,-0.114554038379521,
3.52168776344319));
#39123=CARTESIAN_POINT('Ctrl Pts',(19.4598914756013,0.340364234683876,3.64495435060606));
#39124=CARTESIAN_POINT('Ctrl Pts',(19.5076073116642,0.482720800247919,4.09426482953845));
#39125=CARTESIAN_POINT('Ctrl Pts',(19.555323147727,0.181787415268628,4.45701044834135));
#39126=CARTESIAN_POINT('Ctrl Pts',(19.6030389837899,-0.28608412753634,4.40007637198121));
#39127=CARTESIAN_POINT('Ctrl Pts',(19.6507548198527,-0.491240257057309,
3.97574594767572));
#39128=CARTESIAN_POINT('Ctrl Pts',(19.6984706559155,-0.245282818621706,
3.57368850533185));
#39129=CARTESIAN_POINT('Ctrl Pts',(19.7461864919783,0.225921452997342,3.56311925573479));
#39130=CARTESIAN_POINT('Ctrl Pts',(19.7939023280412,0.489658867576397,3.95374471702426));
#39131=CARTESIAN_POINT('Ctrl Pts',(19.841618164104,0.303734463062876,4.38684635894002));
#39132=CARTESIAN_POINT('Ctrl Pts',(19.8893340001669,-0.161112940293692,
4.46470246728215));
#39133=CARTESIAN_POINT('Ctrl Pts',(19.9370498362297,-0.47800980043334,4.11581244897344));
#39134=CARTESIAN_POINT('Ctrl Pts',(19.9847656722926,-0.355939225796451,
3.66057517601247));
#39135=CARTESIAN_POINT('Ctrl Pts',(20.0324815083554,0.0929888682922082,
3.51702731322357));
#39136=CARTESIAN_POINT('Ctrl Pts',(20.0801973444182,0.456536973876988,3.81701888067549));
#39137=CARTESIAN_POINT('Ctrl Pts',(20.1279131804811,0.400815378068436,4.28501049648274));
#39138=CARTESIAN_POINT('Ctrl Pts',(20.1756290165439,-0.022934367574535,
4.49133741301101));
#39139=CARTESIAN_POINT('Ctrl Pts',(20.2233448526067,-0.425711472830213,
4.24633918020534));
#39140=CARTESIAN_POINT('Ctrl Pts',(20.2710606886696,-0.437384262562023,
3.77535541015343));
#39141=CARTESIAN_POINT('Ctrl Pts',(20.3187765247324,-0.0477164433392854,
3.51022640082505));
#39142=CARTESIAN_POINT('Ctrl Pts',(20.3664923607953,0.386374384143037,3.69571627142296));
#39143=CARTESIAN_POINT('Ctrl Pts',(20.4062555575143,0.45143962727185,4.08165775845481));
#39144=CARTESIAN_POINT('Ctrl Pts',(20.4380661148895,0.291471375703242,4.31996082336987));
#39145=CARTESIAN_POINT('Ctrl Pts',(20.461924032921,0.103697252552815,4.42124466395835));
#39146=CARTESIAN_POINT('Ctrl Pts',(20.4857819509523,-0.111451542568667,
4.41901444157942));
#39147=CARTESIAN_POINT('Ctrl Pts',(20.5096398689838,-0.298255971346869,
4.31460392554555));
#39148=CARTESIAN_POINT('Ctrl Pts',(20.5334977870152,-0.412709509332759,
4.13311446574462));
#39149=CARTESIAN_POINT('Ctrl Pts',(20.5573557050466,-0.425936384696969,
3.91915434697803));
#39150=CARTESIAN_POINT('Ctrl Pts',(20.581213623078,-0.335173342752607,3.72492109335083));
#39151=CARTESIAN_POINT('Ctrl Pts',(20.6050715411095,-0.162364888615448,
3.59797442377207));
#39152=CARTESIAN_POINT('Ctrl Pts',(20.6289294591408,0.0501004451364318,
3.56932214892951));
#39153=CARTESIAN_POINT('Ctrl Pts',(20.6527873771723,0.250339089241223,3.64598859455508));
#39154=CARTESIAN_POINT('Ctrl Pts',(20.6766452952037,0.389350172549011,3.80921715950176));
#39155=CARTESIAN_POINT('Ctrl Pts',(20.7005032132352,0.433161330121289,4.01909908002448));
#39156=CARTESIAN_POINT('Ctrl Pts',(20.7243611312665,0.371049143609512,4.22430982617278));
#39157=CARTESIAN_POINT('Ctrl Pts',(20.748219049298,0.218207240773441,4.37467120177868));
#39158=CARTESIAN_POINT('Ctrl Pts',(20.7720769673293,0.01200671405148,4.43341500212799));
#39159=CARTESIAN_POINT('Ctrl Pts',(20.7959348853608,-0.197129246586683,
4.38617716647524));
#39160=CARTESIAN_POINT('Ctrl Pts',(20.8197928033922,-0.358062019934396,
4.24450842127602));
#39161=CARTESIAN_POINT('Ctrl Pts',(20.8436507214237,-0.431438726014498,
4.04305074550709));
#39162=CARTESIAN_POINT('Ctrl Pts',(20.867508639455,-0.399316990859146,3.83106596928302));
#39163=CARTESIAN_POINT('Ctrl Pts',(20.8913665574865,-0.269551332195825,
3.66039017609669));
#39164=CARTESIAN_POINT('Ctrl Pts',(20.9152244755179,-0.0738730526583281,
3.57275822989076));
#39165=CARTESIAN_POINT('Ctrl Pts',(20.9390823935493,0.139869212314499,3.58959853735383));
#39166=CARTESIAN_POINT('Ctrl Pts',(20.9629403115807,0.319409638666883,3.70679317993256));
#39167=CARTESIAN_POINT('Ctrl Pts',(20.9867982296122,0.420845711130686,3.8956848776653));
#39168=CARTESIAN_POINT('Ctrl Pts',(21.0106561476436,0.419373541863394,4.11008446384341));
#39169=CARTESIAN_POINT('Ctrl Pts',(21.034514065675,0.315353119032788,4.29756540021079));
#39170=CARTESIAN_POINT('Ctrl Pts',(21.0583719837064,0.134220268060588,4.41228349058099));
#39171=CARTESIAN_POINT('Ctrl Pts',(21.0822299017379,-0.079733094278782,
4.42618703719455));
#39172=CARTESIAN_POINT('Ctrl Pts',(21.1060878197692,-0.274189543318984,
4.33587624407661));
#39173=CARTESIAN_POINT('Ctrl Pts',(21.1299457378007,-0.401599180171465,
4.16343456021562));
#39174=CARTESIAN_POINT('Ctrl Pts',(21.1538036558321,-0.430806878168669,
3.95102867450389));
#39175=CARTESIAN_POINT('Ctrl Pts',(21.1776615738635,-0.354670559489406,
3.75059761183336));
#39176=CARTESIAN_POINT('Ctrl Pts',(21.2015194918949,-0.191807627993766,
3.61115222665144));
#39177=CARTESIAN_POINT('Ctrl Pts',(21.2253774099264,0.0179574932869785,
3.56679071405539));
#39178=CARTESIAN_POINT('Ctrl Pts',(21.2492353279577,0.223331518303719,3.62836067225603));
#39179=CARTESIAN_POINT('Ctrl Pts',(21.2730932459892,0.374094903668402,3.78080656934254));
#39180=CARTESIAN_POINT('Ctrl Pts',(21.2969511640206,0.433381894944723,3.98685123093373));
#39181=CARTESIAN_POINT('Ctrl Pts',(21.320809082052,0.386695207821707,4.19611112472705));
#39182=CARTESIAN_POINT('Ctrl Pts',(21.3446670000834,0.245451009020076,4.35741650656472));
#39183=CARTESIAN_POINT('Ctrl Pts',(21.3685249181149,0.0441873525619181,
4.43132381671722));
#39184=CARTESIAN_POINT('Ctrl Pts',(21.3923828361462,-0.167881315237013,
4.39976070465745));
#39185=CARTESIAN_POINT('Ctrl Pts',(21.4162407541777,-0.338898428465248,
4.27044521104599));
#39186=CARTESIAN_POINT('Ctrl Pts',(21.4400986722091,-0.427045644525908,
4.07499849655415));
#39187=CARTESIAN_POINT('Ctrl Pts',(21.4639565902406,-0.410768568010174,
3.86121260673678));
#39188=CARTESIAN_POINT('Ctrl Pts',(21.4878145082719,-0.294047387504818,
3.68136401506497));
#39189=CARTESIAN_POINT('Ctrl Pts',(21.5116724263034,-0.105423611064507,
3.57943060117972));
#39190=CARTESIAN_POINT('Ctrl Pts',(21.5355303443348,0.108979109962582,3.58033786138646));
#39191=CARTESIAN_POINT('Ctrl Pts',(21.5593882623662,0.296733470072461,3.68386394585134));
#39192=CARTESIAN_POINT('Ctrl Pts',(21.5832461803976,0.411928413892185,3.86469390692879));
#39193=CARTESIAN_POINT('Ctrl Pts',(21.6071040984291,0.426395639810567,4.07860989342611));
#39194=CARTESIAN_POINT('Ctrl Pts',(21.6309620164605,0.33659751701124,4.27330361969026));
#39195=CARTESIAN_POINT('Ctrl Pts',(21.6548199344919,0.164492132570386,4.401167166299));
#39196=CARTESIAN_POINT('Ctrl Pts',(21.6786778525233,-0.0478360589596606,
4.43093441317345));
#39197=CARTESIAN_POINT('Ctrl Pts',(21.7025357705547,-0.248467031045983,
4.35532645760922));
#39198=CARTESIAN_POINT('Ctrl Pts',(21.7263936885861,-0.388341045935521,
4.1928315042612));
#39199=CARTESIAN_POINT('Ctrl Pts',(21.7502516066176,-0.433255096896122,
3.98318399549658));
#39200=CARTESIAN_POINT('Ctrl Pts',(21.774109524649,-0.372226475033738,3.77764845789182));
#39201=CARTESIAN_POINT('Ctrl Pts',(21.7979674426804,-0.220178340780001,
3.62648392906691));
#39202=CARTESIAN_POINT('Ctrl Pts',(21.8218253607118,-0.0142906046679706,
3.56665425395863));
#39203=CARTESIAN_POINT('Ctrl Pts',(21.8456832787432,0.195091573553633,3.61278941785858));
#39204=CARTESIAN_POINT('Ctrl Pts',(21.8695411967747,0.356768547853618,3.75360811649661));
#39205=CARTESIAN_POINT('Ctrl Pts',(21.8933991148061,0.431205894023261,3.95467634223136));
#39206=CARTESIAN_POINT('Ctrl Pts',(21.9172570328375,0.400201653291494,4.16682743688221));
#39207=CARTESIAN_POINT('Ctrl Pts',(21.941114950869,0.271337207055788,4.33818467892719));
#39208=CARTESIAN_POINT('Ctrl Pts',(21.9649728689003,0.0761234226178432,
4.4268465550088));
#39209=CARTESIAN_POINT('Ctrl Pts',(21.9888307869318,-0.137704612210607,
4.41113282132402));
#39210=CARTESIAN_POINT('Ctrl Pts',(22.0126887049632,-0.317860118355158,
4.29488591379237));
#39211=CARTESIAN_POINT('Ctrl Pts',(22.0365466229946,-0.420290167226249,
4.10653136780738));
#39212=CARTESIAN_POINT('Ctrl Pts',(22.060404541026,-0.419947821735935,3.89212700053744));
#39213=CARTESIAN_POINT('Ctrl Pts',(22.0842624590574,-0.316916794682727,
3.70410052003731));
#39214=CARTESIAN_POINT('Ctrl Pts',(22.1081203770888,-0.136390978688423,
3.58842952252864));
#39215=CARTESIAN_POINT('Ctrl Pts',(22.1319782951203,0.0774861468089536,
3.57339871771534));
#39216=CARTESIAN_POINT('Ctrl Pts',(22.1558362131517,0.27241579873489,3.66268354680831));
#39217=CARTESIAN_POINT('Ctrl Pts',(22.1796941311831,0.400732367405962,3.83445143701846));
#39218=CARTESIAN_POINT('Ctrl Pts',(22.2035520492145,0.431058956528623,4.04670046033727));
#39219=CARTESIAN_POINT('Ctrl Pts',(22.227409967246,0.355979888945518,4.24752994899471));
#39220=CARTESIAN_POINT('Ctrl Pts',(22.2512678852773,0.193854041863619,4.38783162256878));
#39221=CARTESIAN_POINT('Ctrl Pts',(22.2751258033088,-0.0156743990186396,
4.43329790005389));
#39222=CARTESIAN_POINT('Ctrl Pts',(22.2989837213402,-0.221370022215225,
4.37281103827166));
#39223=CARTESIAN_POINT('Ctrl Pts',(22.3228416393716,-0.372934645290675,
4.22116172228637));
#39224=CARTESIAN_POINT('Ctrl Pts',(22.346699557403,-0.43330658847365,4.01543234121164));
#39225=CARTESIAN_POINT('Ctrl Pts',(22.3705574754345,-0.387723268841402,
3.80592933171158));
#39226=CARTESIAN_POINT('Ctrl Pts',(22.3944153934659,-0.247331046528593,
3.64388188817752));
#39227=CARTESIAN_POINT('Ctrl Pts',(22.4182733114973,-0.0464596501027702,
3.56891502119853));
#39228=CARTESIAN_POINT('Ctrl Pts',(22.4421312295287,0.165772403721094,3.59936017830047));
#39229=CARTESIAN_POINT('Ctrl Pts',(22.4659891475602,0.337468575289321,3.7277726770023));
#39230=CARTESIAN_POINT('Ctrl Pts',(22.4898470655915,0.426644514167594,3.92275218663495));
#39231=CARTESIAN_POINT('Ctrl Pts',(22.513704983623,0.411494197867752,4.13662086224655));
#39232=CARTESIAN_POINT('Ctrl Pts',(22.5375629016544,0.295722435535401,4.31708206952049));
#39233=CARTESIAN_POINT('Ctrl Pts',(22.5614208196858,0.107638304484935,4.42000797176855));
#39234=CARTESIAN_POINT('Ctrl Pts',(22.5852787377172,-0.106765988085903,
4.42023067651324));
#39235=CARTESIAN_POINT('Ctrl Pts',(22.6091366557487,-0.295063722636797,
4.31769517074077));
#39236=CARTESIAN_POINT('Ctrl Pts',(22.6329945737801,-0.411209141905604,
4.13747522778479));
#39237=CARTESIAN_POINT('Ctrl Pts',(22.6568524918115,-0.426804986482714,
3.92363755172126));
#39238=CARTESIAN_POINT('Ctrl Pts',(22.6807104098429,-0.33803111495158,3.72847502015617));
#39239=CARTESIAN_POINT('Ctrl Pts',(22.7045683278743,-0.16660749730952,3.59970312177549));
#39240=CARTESIAN_POINT('Ctrl Pts',(22.7284262459057,0.0455714674079685,
3.56882345794434));
#39241=CARTESIAN_POINT('Ctrl Pts',(22.7522841639372,0.246577802732478,3.64336153500176));
#39242=CARTESIAN_POINT('Ctrl Pts',(22.7761420819686,0.387346815298129,3.80514019809748));
#39243=CARTESIAN_POINT('Ctrl Pts',(22.7920473606562,0.417963038852713,3.94471011778788));
#39244=CARTESIAN_POINT('Ctrl Pts',(22.8,0.415641328671541,4.01393920819689));
#39245=CARTESIAN_POINT('Ctrl Pts',(3.96816317011929,0.203757107801821,4.42939176513376));
#39246=CARTESIAN_POINT('Ctrl Pts',(3.9761158094631,0.132237748973037,4.46332948562603));
#39247=CARTESIAN_POINT('Ctrl Pts',(3.99202108815071,-0.0280119004087947,
4.49474661085258));
#39248=CARTESIAN_POINT('Ctrl Pts',(4.01587900618213,-0.261670681609628,
4.42079217330492));
#39249=CARTESIAN_POINT('Ctrl Pts',(4.03973692421355,-0.431283260509235,
4.24398813071681));
#39250=CARTESIAN_POINT('Ctrl Pts',(4.06359484224497,-0.495466080430727,
4.00749935521381));
#39251=CARTESIAN_POINT('Ctrl Pts',(4.08745276027639,-0.438477829352452,
3.76918881818141));
#39252=CARTESIAN_POINT('Ctrl Pts',(4.11131067830781,-0.274278321106756,
3.5873115455631));
#39253=CARTESIAN_POINT('Ctrl Pts',(4.13516859633923,-0.0430057845205295,
3.50635120590702));
#39254=CARTESIAN_POINT('Ctrl Pts',(4.15902651437064,0.198780450874126,3.54609966156282));
#39255=CARTESIAN_POINT('Ctrl Pts',(4.18288443240206,0.391960715466274,3.69684005745713));
#39256=CARTESIAN_POINT('Ctrl Pts',(4.20674235043348,0.489295238859844,3.92171081754005));
#39257=CARTESIAN_POINT('Ctrl Pts',(4.2306002684649,0.466984102771714,4.16572567991789));
#39258=CARTESIAN_POINT('Ctrl Pts',(4.25445818649632,0.330482445391075,4.36921595913043));
#39259=CARTESIAN_POINT('Ctrl Pts',(4.27831610452774,0.113168927396708,4.48242295331799));
#39260=CARTESIAN_POINT('Ctrl Pts',(4.30217402255916,-0.131817528672551,
4.47766435517297));
#39261=CARTESIAN_POINT('Ctrl Pts',(4.32603194059057,-0.344570980451485,
4.35610383169054));
#39262=CARTESIAN_POINT('Ctrl Pts',(4.349889858622,-0.473067456356951,4.14746621026076));
#39263=CARTESIAN_POINT('Ctrl Pts',(4.37374777665341,-0.485886045261059,
3.9027690893624));
#39264=CARTESIAN_POINT('Ctrl Pts',(4.39760569468484,-0.379892264971952,
3.68184757153936));
#39265=CARTESIAN_POINT('Ctrl Pts',(4.42146361271625,-0.181004475645389,
3.53872299041084));
#39266=CARTESIAN_POINT('Ctrl Pts',(4.44532153074767,0.0621438372772935,
3.50839320219298));
#39267=CARTESIAN_POINT('Ctrl Pts',(4.46917944877909,0.290096289836991,3.5982746675986));
#39268=CARTESIAN_POINT('Ctrl Pts',(4.49303736681051,0.447112297141319,3.78638891931142));
#39269=CARTESIAN_POINT('Ctrl Pts',(4.51689528484194,0.494797168872773,4.02673689903048));
#39270=CARTESIAN_POINT('Ctrl Pts',(4.54075320287334,0.421490654719143,4.26054697856981));
#39271=CARTESIAN_POINT('Ctrl Pts',(4.56461112090478,0.245118194360182,4.43064622472778));
#39272=CARTESIAN_POINT('Ctrl Pts',(4.58846903893618,0.00880765856895839,
4.49544073835303));
#39273=CARTESIAN_POINT('Ctrl Pts',(4.61232695696761,-0.229656589644598,
4.43908649592634));
#39274=CARTESIAN_POINT('Ctrl Pts',(4.63618487499902,-0.411963545977342,
4.2753636447643));
#39275=CARTESIAN_POINT('Ctrl Pts',(4.66004279303045,-0.493534193653132,
4.04430688170513));
#39276=CARTESIAN_POINT('Ctrl Pts',(4.68390071106186,-0.454422287381232,
3.80241587917234));
#39277=CARTESIAN_POINT('Ctrl Pts',(4.70775862909328,-0.304191753628974,
3.60883957626609));
#39278=CARTESIAN_POINT('Ctrl Pts',(4.7316165471247,-0.0795780500979935,
3.51091265195837));
#39279=CARTESIAN_POINT('Ctrl Pts',(4.75547446515612,0.164494654344808,3.53258090671894));
#39280=CARTESIAN_POINT('Ctrl Pts',(4.77933238318754,0.368343935055725,3.66854586202706));
#39281=CARTESIAN_POINT('Ctrl Pts',(4.80319030121895,0.482123090158262,3.88556038269908));
#39282=CARTESIAN_POINT('Ctrl Pts',(4.82704821925038,0.478010016947761,4.13055850707372));
#39283=CARTESIAN_POINT('Ctrl Pts',(4.85090613728179,0.357010473862124,4.34363152012653));
#39284=CARTESIAN_POINT('Ctrl Pts',(4.87476405531322,0.14871214514713,4.47267726617372));
#39285=CARTESIAN_POINT('Ctrl Pts',(4.89862197334463,-0.0959503538938319,
4.48614054517122));
#39286=CARTESIAN_POINT('Ctrl Pts',(4.92247989137606,-0.317150377772593,
4.38072921867179));
#39287=CARTESIAN_POINT('Ctrl Pts',(4.94633780940747,-0.460798495283114,
4.1822192273514));
#39288=CARTESIAN_POINT('Ctrl Pts',(4.97019572743889,-0.49176882879792,3.93915167139151));
#39289=CARTESIAN_POINT('Ctrl Pts',(4.99405364547031,-0.40248828815769,3.71096318925158));
#39290=CARTESIAN_POINT('Ctrl Pts',(5.01791156350173,-0.214788397502062,
3.55345208054429));
#39291=CARTESIAN_POINT('Ctrl Pts',(5.04176948153314,0.0254331070612992,
3.50513410186502));
#39292=CARTESIAN_POINT('Ctrl Pts',(5.06562739956457,0.259435524164246,3.57782431515618));
#39293=CARTESIAN_POINT('Ctrl Pts',(5.08948531759598,0.429998888727244,3.75374798322641));
#39294=CARTESIAN_POINT('Ctrl Pts',(5.11334323562741,0.495415812061873,3.98988697716804));
#39295=CARTESIAN_POINT('Ctrl Pts',(5.13720115365882,0.439690074491602,4.2284988806653));
#39296=CARTESIAN_POINT('Ctrl Pts',(5.16105907169025,0.276448136790977,4.41123658365534));
#39297=CARTESIAN_POINT('Ctrl Pts',(5.18491698972166,0.0456070993489057,
4.49341574008204));
#39298=CARTESIAN_POINT('Ctrl Pts',(5.20877490775308,-0.196386116196418,
4.45494130768376));
#39299=CARTESIAN_POINT('Ctrl Pts',(5.2326328257845,-0.390357576881318,4.3052213332044));
#39300=CARTESIAN_POINT('Ctrl Pts',(5.25649074381592,-0.488875976891831,
4.08086642869437));
#39301=CARTESIAN_POINT('Ctrl Pts',(5.28034866184734,-0.467850883838054,
3.83673747961128));
#39302=CARTESIAN_POINT('Ctrl Pts',(5.30420657987876,-0.332423505683668,
3.632530663945));
#39303=CARTESIAN_POINT('Ctrl Pts',(5.32806449791017,-0.115709525355139,
3.5181801106079));
#39304=CARTESIAN_POINT('Ctrl Pts',(5.3519224159416,0.129298585786916,3.52164764473745));
#39305=CARTESIAN_POINT('Ctrl Pts',(5.37578033397301,0.342689670681295,3.64208535978523));
#39306=CARTESIAN_POINT('Ctrl Pts',(5.39963825200445,0.472283796414913,3.85004295376459));
#39307=CARTESIAN_POINT('Ctrl Pts',(5.42349617003584,0.48639166917272,4.09466913029638));
#39308=CARTESIAN_POINT('Ctrl Pts',(5.44735408806728,0.381563529774833,4.31614612573549));
#39309=CARTESIAN_POINT('Ctrl Pts',(5.47121200609869,0.183432713764955,4.46031678178449));
#39310=CARTESIAN_POINT('Ctrl Pts',(5.49506992413012,-0.059552397366927,
4.49192744591021));
#39311=CARTESIAN_POINT('Ctrl Pts',(5.51892784216153,-0.287975325168481,
4.40324844967551));
#39312=CARTESIAN_POINT('Ctrl Pts',(5.54278576019295,-0.445980441674811,
4.21596422322942));
#39313=CARTESIAN_POINT('Ctrl Pts',(5.56664367822437,-0.494931191930538,
3.97587086145358));
#39314=CARTESIAN_POINT('Ctrl Pts',(5.59050159625579,-0.422857784100094,
3.74167773132221));
#39315=CARTESIAN_POINT('Ctrl Pts',(5.61435951428721,-0.247384129650275,
3.57065143242979));
#39316=CARTESIAN_POINT('Ctrl Pts',(5.63821743231862,-0.0114183168777074,
3.50461255354752));
#39317=CARTESIAN_POINT('Ctrl Pts',(5.66207535035005,0.227339585372105,3.55970939936999));
#39318=CARTESIAN_POINT('Ctrl Pts',(5.68593326838146,0.410506766445453,3.72246929038963));
#39319=CARTESIAN_POINT('Ctrl Pts',(5.70979118641288,0.493293861043031,3.9530929995654));
#39320=CARTESIAN_POINT('Ctrl Pts',(5.73364910444431,0.455457169749513,4.19518674831082));
#39321=CARTESIAN_POINT('Ctrl Pts',(5.75750702247572,0.306248793691327,4.38955201985635));
#39322=CARTESIAN_POINT('Ctrl Pts',(5.78136494050715,0.0821542461994931,
4.48866121222712));
#39323=CARTESIAN_POINT('Ctrl Pts',(5.80522285853855,-0.162029253596618,
4.46827942571263));
#39324=CARTESIAN_POINT('Ctrl Pts',(5.82908077656998,-0.366592184898752,
4.33339056701663));
#39325=CARTESIAN_POINT('Ctrl Pts',(5.85293869460139,-0.481513345756758,
4.11697862749145));
#39326=CARTESIAN_POINT('Ctrl Pts',(5.87679661263282,-0.478691368855474,
3.87196223809426));
#39327=CARTESIAN_POINT('Ctrl Pts',(5.90065453066423,-0.358816329143926,
3.65825454842257));
#39328=CARTESIAN_POINT('Ctrl Pts',(5.92451244869565,-0.151200892471453,
3.52811296978032));
#39329=CARTESIAN_POINT('Ctrl Pts',(5.94837036672708,0.093387223403125,3.5133605500302));
#39330=CARTESIAN_POINT('Ctrl Pts',(5.97222828475848,0.315139728168714,3.61760487120619));
#39331=CARTESIAN_POINT('Ctrl Pts',(5.99608620278992,0.459831779670103,3.81535495398299));
#39332=CARTESIAN_POINT('Ctrl Pts',(6.01994412082132,0.492082823488737,4.05825627791571));
#39333=CARTESIAN_POINT('Ctrl Pts',(6.04380203885276,0.404005480250355,4.28691141512903));
#39334=CARTESIAN_POINT('Ctrl Pts',(6.06765995688416,0.21713917558903,4.44541067075535));
#39335=CARTESIAN_POINT('Ctrl Pts',(6.09151787491559,-0.0228261843714051,
4.49499153360272));
#39336=CARTESIAN_POINT('Ctrl Pts',(6.11537579294701,-0.257204988275768,
4.42353981062321));
#39337=CARTESIAN_POINT('Ctrl Pts',(6.13923371097843,-0.428699479426561,
4.24850911946619));
#39338=CARTESIAN_POINT('Ctrl Pts',(6.16309162900984,-0.49534768549136,4.01273373861842));
#39339=CARTESIAN_POINT('Ctrl Pts',(6.18694954704127,-0.440903093044182,
3.77380201544612));
#39340=CARTESIAN_POINT('Ctrl Pts',(6.21080746507268,-0.278582990390117,
3.59026229064107));
#39341=CARTESIAN_POINT('Ctrl Pts',(6.23466538310411,-0.048260127889517,
3.50676273730504));
#39342=CARTESIAN_POINT('Ctrl Pts',(6.25852330113552,0.194087080856728,3.5441598063702));
#39343=CARTESIAN_POINT('Ctrl Pts',(6.28238121916694,0.388553448942855,3.69248145192407));
#39344=CARTESIAN_POINT('Ctrl Pts',(6.30623913719837,0.488798280742691,3.9170164641697));
#39345=CARTESIAN_POINT('Ctrl Pts',(6.33009705522977,0.468067515948433,4.15995908608738));
#39346=CARTESIAN_POINT('Ctrl Pts',(6.36190761260502,0.291040001689194,4.43610431491443));
#39347=CARTESIAN_POINT('Ctrl Pts',(6.40167080932402,-0.143168317426403,
4.54352222151223));
#39348=CARTESIAN_POINT('Ctrl Pts',(6.44938664538688,-0.535165231989368,
4.17285582464912));
#39349=CARTESIAN_POINT('Ctrl Pts',(6.49710248144971,-0.434543251113388,
3.64369891234367));
#39350=CARTESIAN_POINT('Ctrl Pts',(6.54481831751255,0.0645215567551043,
3.4416075490323));
#39351=CARTESIAN_POINT('Ctrl Pts',(6.59253415357539,0.504653900644641,3.75236619672659));
#39352=CARTESIAN_POINT('Ctrl Pts',(6.64024998963822,0.481186238846835,4.29049388273239));
#39353=CARTESIAN_POINT('Ctrl Pts',(6.68796582570107,0.01592709648968,4.56187610740764));
#39354=CARTESIAN_POINT('Ctrl Pts',(6.7356816617639,-0.464005405879062,4.31726850783359));
#39355=CARTESIAN_POINT('Ctrl Pts',(6.78339749782674,-0.517809574500644,
3.78131383674221));
#39356=CARTESIAN_POINT('Ctrl Pts',(6.83111333388957,-0.0961144992151805,
3.44617913151078));
#39357=CARTESIAN_POINT('Ctrl Pts',(6.87882916995242,0.413851019972934,3.61962818876606));
#39358=CARTESIAN_POINT('Ctrl Pts',(6.92654500601525,0.543767061592725,4.14237771887731));
#39359=CARTESIAN_POINT('Ctrl Pts',(6.97426084207809,0.174335412693353,4.53438003016987));
#39360=CARTESIAN_POINT('Ctrl Pts',(7.02197667814094,-0.355192171006393,
4.43565270890428));
#39361=CARTESIAN_POINT('Ctrl Pts',(7.06969251420376,-0.558540766450571,
3.93685892261342));
#39362=CARTESIAN_POINT('Ctrl Pts',(7.11740835026661,-0.248973074301851,
3.49604849518665));
#39363=CARTESIAN_POINT('Ctrl Pts',(7.16512418632944,0.289230577826905,3.51802452284194));
#39364=CARTESIAN_POINT('Ctrl Pts',(7.21284002239229,0.561829257914175,3.98260602935256));
#39365=CARTESIAN_POINT('Ctrl Pts',(7.26055585845511,0.318491529052478,4.46316069626365));
#39366=CARTESIAN_POINT('Ctrl Pts',(7.30827169451797,-0.217321894570402,
4.51838776411367));
#39367=CARTESIAN_POINT('Ctrl Pts',(7.35598753058078,-0.553565266295818,
4.09757137442565));
#39368=CARTESIAN_POINT('Ctrl Pts',(7.40370336664365,-0.381461142739227,
3.58715368886071));
#39369=CARTESIAN_POINT('Ctrl Pts',(7.45141920270646,0.140944621146953,3.45585912402047));
#39370=CARTESIAN_POINT('Ctrl Pts',(7.49913503876933,0.533918768911932,3.82425749787944));
#39371=CARTESIAN_POINT('Ctrl Pts',(7.54685087483214,0.436587096747522,4.3540429157916));
#39372=CARTESIAN_POINT('Ctrl Pts',(7.594566710895,-0.0616692246238245,4.5587052763707));
#39373=CARTESIAN_POINT('Ctrl Pts',(7.64228254695782,-0.503293747851232,
4.25029998493175));
#39374=CARTESIAN_POINT('Ctrl Pts',(7.68999838302067,-0.482735878399531,
3.7120403659385));
#39375=CARTESIAN_POINT('Ctrl Pts',(7.7377142190835,-0.0188742238918736,
3.43821850974892));
#39376=CARTESIAN_POINT('Ctrl Pts',(7.78543005514633,0.462319920793015,3.6802892401675));
#39377=CARTESIAN_POINT('Ctrl Pts',(7.83314589120918,0.518958568528469,4.21595528072725));
#39378=CARTESIAN_POINT('Ctrl Pts',(7.88086172727202,0.099029577569048,4.55330626409362));
#39379=CARTESIAN_POINT('Ctrl Pts',(7.92857756333485,-0.411839798232008,
4.38254759143289));
#39380=CARTESIAN_POINT('Ctrl Pts',(7.9762933993977,-0.544510350349916,3.86048957930736));
#39381=CARTESIAN_POINT('Ctrl Pts',(8.02400923546053,-0.177148669371157,
3.466546133148));
#39382=CARTESIAN_POINT('Ctrl Pts',(8.07172507152338,0.352891360472903,3.56248158116143));
#39383=CARTESIAN_POINT('Ctrl Pts',(8.1194409075862,0.558865824063627,4.06019692528064));
#39384=CARTESIAN_POINT('Ctrl Pts',(8.16715674364906,0.251625202160443,4.50263250666582));
#39385=CARTESIAN_POINT('Ctrl Pts',(8.21487257971187,-0.286686714637947,
4.48349292318459));
#39386=CARTESIAN_POINT('Ctrl Pts',(8.26258841577472,-0.561729810142263,
4.02035434884804));
#39387=CARTESIAN_POINT('Ctrl Pts',(8.31030425183756,-0.32092777766878,3.53852406277244));
#39388=CARTESIAN_POINT('Ctrl Pts',(8.3580200879004,0.21458717114652,3.4804742305729));
#39389=CARTESIAN_POINT('Ctrl Pts',(8.40573592396324,0.553043418849938,3.89951290636976));
#39390=CARTESIAN_POINT('Ctrl Pts',(8.45345176002607,0.383631385356639,4.41083042643994));
#39391=CARTESIAN_POINT('Ctrl Pts',(8.50116759608892,-0.13807525223727,4.54487604447167));
#39392=CARTESIAN_POINT('Ctrl Pts',(8.54888343215175,-0.532985261140852,
4.17855360686946));
#39393=CARTESIAN_POINT('Ctrl Pts',(8.59659926821459,-0.43844670370641,3.64826264467864));
#39394=CARTESIAN_POINT('Ctrl Pts',(8.64431510427743,0.0587242081113278,
3.4409775080543));
#39395=CARTESIAN_POINT('Ctrl Pts',(8.69203094034026,0.501967776032349,3.74705132745037));
#39396=CARTESIAN_POINT('Ctrl Pts',(8.73974677640311,0.484246611455832,4.28541180496438));
#39397=CARTESIAN_POINT('Ctrl Pts',(8.78746261246592,0.021834332487559,4.56167423035448));
#39398=CARTESIAN_POINT('Ctrl Pts',(8.83517844852879,-0.460628749968427,
4.32214256754115));
#39399=CARTESIAN_POINT('Ctrl Pts',(8.88289428459161,-0.520089363644054,
3.78678242815423));
#39400=CARTESIAN_POINT('Ctrl Pts',(8.93061012065447,-0.101943912081849,
3.44722326576734));
#39401=CARTESIAN_POINT('Ctrl Pts',(8.97832595671729,0.409818202553832,3.61528748398963));
#39402=CARTESIAN_POINT('Ctrl Pts',(9.02604179278014,0.545237955920739,4.1366391252272));
#39403=CARTESIAN_POINT('Ctrl Pts',(9.07375762884296,0.179957304801303,4.53251295530543));
#39404=CARTESIAN_POINT('Ctrl Pts',(9.12147346490582,-0.350580908316224,
4.43937194476168));
#39405=CARTESIAN_POINT('Ctrl Pts',(9.16918930096864,-0.559175278946307,
3.94274891673689));
#39406=CARTESIAN_POINT('Ctrl Pts',(9.21690513703149,-0.254270386902387,
3.49870043939378));
#39407=CARTESIAN_POINT('Ctrl Pts',(9.26462097309432,0.284134913886797,3.51500306204057));
#39408=CARTESIAN_POINT('Ctrl Pts',(9.31233680915716,0.56161475127612,3.97668583545263));
#39409=CARTESIAN_POINT('Ctrl Pts',(9.36005264522,0.323355121014866,4.45977836490307));
#39410=CARTESIAN_POINT('Ctrl Pts',(9.40776848128284,-0.211846492332409,
4.52064934726353));
#39411=CARTESIAN_POINT('Ctrl Pts',(9.45548431734568,-0.552506212093558,
4.10340002281193));
#39412=CARTESIAN_POINT('Ctrl Pts',(9.50320015340851,-0.385790975888367,
3.59119686639829));
#39413=CARTESIAN_POINT('Ctrl Pts',(9.55091598947136,0.135202049632292,3.45440391781584));
#39414=CARTESIAN_POINT('Ctrl Pts',(9.59863182553417,0.532036952624682,3.81864024657791));
#39415=CARTESIAN_POINT('Ctrl Pts',(9.64634766159704,0.440294135581046,4.34942202748599));
#39416=CARTESIAN_POINT('Ctrl Pts',(9.69406349765985,-0.0557775609627595,
4.55932418400469));
#39417=CARTESIAN_POINT('Ctrl Pts',(9.74177933372271,-0.500627865026369,
4.25559033604309));
#39418=CARTESIAN_POINT('Ctrl Pts',(9.78949516978553,-0.485743897486414,
3.71714394973028));
#39419=CARTESIAN_POINT('Ctrl Pts',(9.83721100584839,-0.0247938347541151,
3.43844862667992));
#39420=CARTESIAN_POINT('Ctrl Pts',(9.88492684191122,0.458924787935076,3.67543457032792));
#39421=CARTESIAN_POINT('Ctrl Pts',(9.93264267797406,0.521205716397956,4.21047394212484));
#39422=CARTESIAN_POINT('Ctrl Pts',(9.98035851403688,0.104855415711801,4.55223185431066));
#39423=CARTESIAN_POINT('Ctrl Pts',(10.0280743500997,-0.407785226630454,
4.3868667575037));
#39424=CARTESIAN_POINT('Ctrl Pts',(10.0757901861625,-0.54595042077573,3.86623596457089));
#39425=CARTESIAN_POINT('Ctrl Pts',(10.1235060222254,-0.182760942995651,
3.46844274359687));
#39426=CARTESIAN_POINT('Ctrl Pts',(10.1712218582882,0.34826072087591,3.55878673023755));
#39427=CARTESIAN_POINT('Ctrl Pts',(10.2189376943511,0.559469206087141,4.05430365143988));
#39428=CARTESIAN_POINT('Ctrl Pts',(10.2666535304139,0.256908510808291,4.49995269395588));
#39429=CARTESIAN_POINT('Ctrl Pts',(10.3143693664768,-0.281575222991369,
4.4864874848512));
#39430=CARTESIAN_POINT('Ctrl Pts',(10.3620852025396,-0.561484096926345,
4.02627333283551));
#39431=CARTESIAN_POINT('Ctrl Pts',(10.4098010386024,-0.325773485110519,
3.5419319750098));
#39432=CARTESIAN_POINT('Ctrl Pts',(10.4575168746653,0.209099930751681,3.47824153281512));
#39433=CARTESIAN_POINT('Ctrl Pts',(10.5052327107281,0.55195366278862,3.89368991932227));
#39434=CARTESIAN_POINT('Ctrl Pts',(10.552948546791,0.387939853388008,4.40676448870664));
#39435=CARTESIAN_POINT('Ctrl Pts',(10.6006643828538,-0.13232509260073,4.54630096923553));
#39436=CARTESIAN_POINT('Ctrl Pts',(10.6483802189166,-0.531073869970951,
4.18416086379456));
#39437=CARTESIAN_POINT('Ctrl Pts',(10.6960960549795,-0.442129340924997,
3.6529030034519));
#39438=CARTESIAN_POINT('Ctrl Pts',(10.7438118910423,0.0528293649267388,
3.44038965581316));
#39439=CARTESIAN_POINT('Ctrl Pts',(10.7915277271051,0.499274052081986,3.74177509795313));
#39440=CARTESIAN_POINT('Ctrl Pts',(10.839243563168,0.487227694891584,4.28029244094358));
#39441=CARTESIAN_POINT('Ctrl Pts',(10.8869593992308,0.0277526485205102,
4.56141292256198));
#39442=CARTESIAN_POINT('Ctrl Pts',(10.9346752352937,-0.457208082016334,
4.32697927894352));
#39443=CARTESIAN_POINT('Ctrl Pts',(10.9823910713565,-0.522307595786967,
3.79227553224832));
#39444=CARTESIAN_POINT('Ctrl Pts',(11.0301069074193,-0.107764007611043,
3.44832836054127));
#39445=CARTESIAN_POINT('Ctrl Pts',(11.0778227434822,0.405740926916492,3.61098974390844));
#39446=CARTESIAN_POINT('Ctrl Pts',(11.125538579545,0.54664772512998,4.13088523113667));
#39447=CARTESIAN_POINT('Ctrl Pts',(11.1732544156078,0.185559506100192,4.53058679668394));
#39448=CARTESIAN_POINT('Ctrl Pts',(11.2209702516707,-0.345930862581405,
4.4430423427091));
#39449=CARTESIAN_POINT('Ctrl Pts',(11.2686860877335,-0.559747597323992,
3.94864528834179));
#39450=CARTESIAN_POINT('Ctrl Pts',(11.3164019237964,-0.259539500620097,
3.50140805588402));
#39451=CARTESIAN_POINT('Ctrl Pts',(11.3641177598592,0.279007713031768,3.51203547753114));
#39452=CARTESIAN_POINT('Ctrl Pts',(11.411833595922,0.561337850721073,3.97076822846069));
#39453=CARTESIAN_POINT('Ctrl Pts',(11.4595494319849,0.328182802800164,4.45634496498341));
#39454=CARTESIAN_POINT('Ctrl Pts',(11.5072652680477,-0.206347562673641,
4.52285309839201));
#39455=CARTESIAN_POINT('Ctrl Pts',(11.5549811041106,-0.551385786278872,
4.10921718641821));
#39456=CARTESIAN_POINT('Ctrl Pts',(11.6026969401734,-0.390077958183356,
3.59528545163414));
#39457=CARTESIAN_POINT('Ctrl Pts',(11.6504127762362,0.129444461032819,3.45300931394821));
#39458=CARTESIAN_POINT('Ctrl Pts',(11.6981286122991,0.530096039923511,3.8130431397972));
#39459=CARTESIAN_POINT('Ctrl Pts',(11.7458444483619,0.443952268776438,4.34476232707146));
#39460=CARTESIAN_POINT('Ctrl Pts',(11.7935602844247,-0.0498797018717475,
4.55988096454574));
#39461=CARTESIAN_POINT('Ctrl Pts',(11.8412761204876,-0.497906374793238,
4.26085229740167));
#39462=CARTESIAN_POINT('Ctrl Pts',(11.8889919565504,-0.48869796246776,3.72227895182515));
#39463=CARTESIAN_POINT('Ctrl Pts',(11.9367077926133,-0.0307106916234339,
3.43874111807518));
#39464=CARTESIAN_POINT('Ctrl Pts',(11.9844236286761,0.455478679883424,3.67061595167475));
#39465=CARTESIAN_POINT('Ctrl Pts',(12.0321394647389,0.523394971212992,4.20496922507643));
#39466=CARTESIAN_POINT('Ctrl Pts',(12.0798553008018,0.110669607010866,4.5510961052335));
#39467=CARTESIAN_POINT('Ctrl Pts',(12.1275711368646,-0.403685360180124,
4.39114295225112));
#39468=CARTESIAN_POINT('Ctrl Pts',(12.1752869729274,-0.547329849620031,
3.8719972077086));
#39469=CARTESIAN_POINT('Ctrl Pts',(12.2230028089903,-0.188352916401613,
3.4703983969034));
#39470=CARTESIAN_POINT('Ctrl Pts',(12.2707186450531,0.34359139813055,3.55514088718992));
#39471=CARTESIAN_POINT('Ctrl Pts',(12.318434481116,0.560010444926212,4.04840434580723));
#39472=CARTESIAN_POINT('Ctrl Pts',(12.3661503171788,0.262163283277844,4.49721734887317));
#39473=CARTESIAN_POINT('Ctrl Pts',(12.4138661532417,-0.276432455305192,
4.48942800979656));
#39474=CARTESIAN_POINT('Ctrl Pts',(12.4615819893045,-0.561176016721412,
4.03218939850585));
#39475=CARTESIAN_POINT('Ctrl Pts',(12.5092978253673,-0.330583007179444,
3.54539076726965));
#39476=CARTESIAN_POINT('Ctrl Pts',(12.5570136614301,0.203589464528802,3.47606678951191));
#39477=CARTESIAN_POINT('Ctrl Pts',(12.604729497493,0.550802598333678,3.88787874069406));
#39478=CARTESIAN_POINT('Ctrl Pts',(12.6524453335558,0.392205230901379,4.40265336950419));
#39479=CARTESIAN_POINT('Ctrl Pts',(12.7001611696187,-0.126560234920843,
4.54766521348015));
#39480=CARTESIAN_POINT('Ctrl Pts',(12.7478770056815,-0.529103489635726,
4.18974766500481));
#39481=CARTESIAN_POINT('Ctrl Pts',(12.7955928417443,-0.44576286851447,3.65758191611243));
#39482=CARTESIAN_POINT('Ctrl Pts',(12.8433086778072,0.0469286537069902,
3.43986396243348));
#39483=CARTESIAN_POINT('Ctrl Pts',(12.89102451387,0.496524871139168,3.73652755085263));
#39484=CARTESIAN_POINT('Ctrl Pts',(12.9387403499328,0.490154659387074,4.27514194336855));
#39485=CARTESIAN_POINT('Ctrl Pts',(12.9864561859957,0.0336678819209607,
4.56108925568614));
#39486=CARTESIAN_POINT('Ctrl Pts',(13.0341720220585,-0.45373662956012,4.33177967103923));
#39487=CARTESIAN_POINT('Ctrl Pts',(13.0818878581214,-0.524467812480695,
3.79779170939055));
#39488=CARTESIAN_POINT('Ctrl Pts',(13.1296036941842,-0.113572133225654,
3.44949473238301));
#39489=CARTESIAN_POINT('Ctrl Pts',(13.177319530247,0.401618583502394,3.60673521324049));
#39490=CARTESIAN_POINT('Ctrl Pts',(13.2250353663099,0.547996775303968,4.12511679893576));
#39491=CARTESIAN_POINT('Ctrl Pts',(13.2727512023727,0.191141096329688,4.52860170299893));
#39492=CARTESIAN_POINT('Ctrl Pts',(13.3204670384356,-0.341242392487953,
4.4466635296155));
#39493=CARTESIAN_POINT('Ctrl Pts',(13.3681828744984,-0.560257741594785,
3.95454736418435));
#39494=CARTESIAN_POINT('Ctrl Pts',(13.4158987105612,-0.264779785921688,
3.5041710536014));
#39495=CARTESIAN_POINT('Ctrl Pts',(13.4636145466241,0.273849521323983,3.50912209380529));
#39496=CARTESIAN_POINT('Ctrl Pts',(13.5113303826869,0.560998599421335,3.96485386839523));
#39497=CARTESIAN_POINT('Ctrl Pts',(13.5590462187498,0.332974031597074,4.45286087643057));
#39498=CARTESIAN_POINT('Ctrl Pts',(13.6067620548126,-0.200825712906817,
4.52499877347948));
#39499=CARTESIAN_POINT('Ctrl Pts',(13.6544778908754,-0.550204115147588,
4.11502221869768));
#39500=CARTESIAN_POINT('Ctrl Pts',(13.7021937269383,-0.394321612469819,
3.5994189906415));
#39501=CARTESIAN_POINT('Ctrl Pts',(13.7499095630011,0.123672494356884,3.45167546721031));
#39502=CARTESIAN_POINT('Ctrl Pts',(13.7976253990639,0.528096246669736,3.80746679929733));
#39503=CARTESIAN_POINT('Ctrl Pts',(13.8453412351268,0.44756108986054,4.34006433209368));
#39504=CARTESIAN_POINT('Ctrl Pts',(13.8930570711896,-0.0439763023801491,
4.56037555616609));
#39505=CARTESIAN_POINT('Ctrl Pts',(13.9407729072525,-0.495129579482757,
4.26608528452492));
#39506=CARTESIAN_POINT('Ctrl Pts',(13.9884887433153,-0.491597745198497,
3.72744480185615));
#39507=CARTESIAN_POINT('Ctrl Pts',(14.0362045793781,-0.0366241372948624,
3.43909595144367));
#39508=CARTESIAN_POINT('Ctrl Pts',(14.083920415441,0.451981979421435,3.66583391943861));
#39509=CARTESIAN_POINT('Ctrl Pts',(14.1316362515038,0.525526089798339,4.19944174101915));
#39510=CARTESIAN_POINT('Ctrl Pts',(14.1793520875667,0.11647150565515,4.54989914301615));
#39511=CARTESIAN_POINT('Ctrl Pts',(14.2270679236295,-0.399540654275635,
4.39537570069553));
#39512=CARTESIAN_POINT('Ctrl Pts',(14.2747837596924,-0.548648483661927,
3.87777266878906));
#39513=CARTESIAN_POINT('Ctrl Pts',(14.3224995957551,-0.193923968459428,
3.47241287584284));
#39514=CARTESIAN_POINT('Ctrl Pts',(14.370215431818,0.338883910883161,3.5515444569815));
#39515=CARTESIAN_POINT('Ctrl Pts',(14.4179312678808,0.560489480462528,4.04249966364955));
#39516=CARTESIAN_POINT('Ctrl Pts',(14.4656471039437,0.267388935893957,4.49442677524682));
#39517=CARTESIAN_POINT('Ctrl Pts',(14.5133629400065,-0.271258982813659,
4.49231417140114));
#39518=CARTESIAN_POINT('Ctrl Pts',(14.5610787760694,-0.560805603747543,
4.03810188873054));
#39519=CARTESIAN_POINT('Ctrl Pts',(14.6087946121322,-0.335355809656676,
3.54890005536578));
#39520=CARTESIAN_POINT('Ctrl Pts',(14.656510448195,0.198056384554314,3.47395024222346));
#39521=CARTESIAN_POINT('Ctrl Pts',(14.7042262842579,0.549590353339887,3.88208001596329));
#39522=CARTESIAN_POINT('Ctrl Pts',(14.7519421203207,0.396427044118869,4.3984975254762));
#39523=CARTESIAN_POINT('Ctrl Pts',(14.7996579563836,-0.120781319530639,
4.54896862567174));
#39524=CARTESIAN_POINT('Ctrl Pts',(14.8473737924464,-0.527074338995675,
4.19531338994486));
#39525=CARTESIAN_POINT('Ctrl Pts',(14.8950896285092,-0.449346882879826,
3.66229886294881));
#39526=CARTESIAN_POINT('Ctrl Pts',(14.9428054645721,0.041022729875082,3.43940048630678));
#39527=CARTESIAN_POINT('Ctrl Pts',(14.9905213006349,0.493720538569869,3.73130926902151));
#39528=CARTESIAN_POINT('Ctrl Pts',(15.0382371366977,0.493027179828974,4.2699608843321));
#39529=CARTESIAN_POINT('Ctrl Pts',(15.0859529727606,0.0395793756528551,
4.56070326567839));
#39530=CARTESIAN_POINT('Ctrl Pts',(15.1336688088234,-0.450214778192253,
4.33654321062351));
#39531=CARTESIAN_POINT('Ctrl Pts',(15.1813846448863,-0.526569773778615,
3.80333034687015));
#39532=CARTESIAN_POINT('Ctrl Pts',(15.2291004809491,-0.119367643786657,
3.45072225173751));
#39533=CARTESIAN_POINT('Ctrl Pts',(15.2768163170119,0.397451630201876,3.60252436455885));
#39534=CARTESIAN_POINT('Ctrl Pts',(15.3245321530748,0.549284956596614,4.11933446935456));
#39535=CARTESIAN_POINT('Ctrl Pts',(15.3722479891376,0.196701455513243,4.52655789474516));
#39536=CARTESIAN_POINT('Ctrl Pts',(15.4199638252005,-0.336516018808871,
4.45023510325662));
#39537=CARTESIAN_POINT('Ctrl Pts',(15.4676796612633,-0.560705655094284,
3.96045448869));
#39538=CARTESIAN_POINT('Ctrl Pts',(15.5153954973261,-0.269990660741143,
3.50698912564524));
#39539=CARTESIAN_POINT('Ctrl Pts',(15.5631113333889,0.268660911710894,3.50626323446785));
#39540=CARTESIAN_POINT('Ctrl Pts',(15.6108271694518,0.560597035059331,3.95894341219528));
#39541=CARTESIAN_POINT('Ctrl Pts',(15.6585430055146,0.337728275218647,4.44932648624059));
#39542=CARTESIAN_POINT('Ctrl Pts',(15.7062588415775,-0.1952815563728,4.52708613419449));
#39543=CARTESIAN_POINT('Ctrl Pts',(15.7539746776403,-0.548961329954127,
4.12081447485494));
#39544=CARTESIAN_POINT('Ctrl Pts',(15.8016905137031,-0.398521467382777,
3.60359702428645));
#39545=CARTESIAN_POINT('Ctrl Pts',(15.849406349766,0.117886790727162,3.4504025257595));
#39546=CARTESIAN_POINT('Ctrl Pts',(15.8971221858288,0.526037794990907,3.80191184447176));
#39547=CARTESIAN_POINT('Ctrl Pts',(15.9448380218916,0.451120197982628,4.33532856438364));
#39548=CARTESIAN_POINT('Ctrl Pts',(15.9925538579545,-0.0380680182095728,
4.56080790392885));
#39549=CARTESIAN_POINT('Ctrl Pts',(16.0402696940173,-0.492297787528177,
4.27128871615743));
#39550=CARTESIAN_POINT('Ctrl Pts',(16.0879855300802,-0.494442923584513,
3.73264092602517));
#39551=CARTESIAN_POINT('Ctrl Pts',(16.135701366143,-0.0425335149309099,
3.43951308737216));
#39552=CARTESIAN_POINT('Ctrl Pts',(16.1834172022058,0.448435074945997,3.66108900478495));
#39553=CARTESIAN_POINT('Ctrl Pts',(16.2311330382687,0.52759883543946,4.19389210391969));
#39554=CARTESIAN_POINT('Ctrl Pts',(16.2788488743315,0.122260467197297,4.54864110061148));
#39555=CARTESIAN_POINT('Ctrl Pts',(16.3265647103944,-0.395351569291248,
4.39956453268331));
#39556=CARTESIAN_POINT('Ctrl Pts',(16.3742805464572,-0.549906176433804,
3.88356170630145));
#39557=CARTESIAN_POINT('Ctrl Pts',(16.42199638252,-0.199473480363076,3.47448595665642));
#39558=CARTESIAN_POINT('Ctrl Pts',(16.4697122185829,0.334138782019088,3.54799783908671));
#39559=CARTESIAN_POINT('Ctrl Pts',(16.5174280546457,0.560906259487099,4.0365902608309));
#39560=CARTESIAN_POINT('Ctrl Pts',(16.5651438907085,0.272584888215931,4.49158128304055));
#39561=CARTESIAN_POINT('Ctrl Pts',(16.6128597267714,-0.26605538016154,4.49514564908375));
#39562=CARTESIAN_POINT('Ctrl Pts',(16.6605755628342,-0.560372899148451,
4.04401014677825));
#39563=CARTESIAN_POINT('Ctrl Pts',(16.7082913988971,-0.340091362401967,
3.55245944950311));
#39564=CARTESIAN_POINT('Ctrl Pts',(16.7560072349599,0.19250130541649,3.4718921260458));
#39565=CARTESIAN_POINT('Ctrl Pts',(16.8037230710227,0.548317062457662,3.87629438922476));
#39566=CARTESIAN_POINT('Ctrl Pts',(16.8514389070856,0.400604824101502,4.39429741823411));
#39567=CARTESIAN_POINT('Ctrl Pts',(16.8991547431484,-0.114988988324618,
4.55021106103346));
#39568=CARTESIAN_POINT('Ctrl Pts',(16.9468705792113,-0.524986643439221,
4.20085742040038));
#39569=CARTESIAN_POINT('Ctrl Pts',(16.9945864152741,-0.45288098592576,3.66705332002498));
#39570=CARTESIAN_POINT('Ctrl Pts',(17.0423022513369,0.0351122494330066,
3.4389992789138));
#39571=CARTESIAN_POINT('Ctrl Pts',(17.0900180873998,0.490861365866046,3.72612083208173));
#39572=CARTESIAN_POINT('Ctrl Pts',(17.1377339234626,0.49584493715134,4.26474983932169));
#39573=CARTESIAN_POINT('Ctrl Pts',(17.1854497595254,0.0454864730955262,
4.56025499541263));
#39574=CARTESIAN_POINT('Ctrl Pts',(17.2331655955883,-0.446642919103261,
4.34126936858499));
#39575=CARTESIAN_POINT('Ctrl Pts',(17.2808814316511,-0.528613246204851,
3.80889082948154));
#39576=CARTESIAN_POINT('Ctrl Pts',(17.328597267714,-0.125149895556227,3.45201078225777));
#39577=CARTESIAN_POINT('Ctrl Pts',(17.3763131037768,0.393240529860342,3.59835766558462));
#39578=CARTESIAN_POINT('Ctrl Pts',(17.4240289398397,0.55051212592285,4.1135388846668));
#39579=CARTESIAN_POINT('Ctrl Pts',(17.4717447759024,0.202239966032548,4.52445559893916));
#39580=CARTESIAN_POINT('Ctrl Pts',(17.5194606119653,-0.331752266527324,
4.45375666691904));
#39581=CARTESIAN_POINT('Ctrl Pts',(17.5671764480281,-0.561091288070378,
3.96636600572338));
#39582=CARTESIAN_POINT('Ctrl Pts',(17.614892284091,-0.275171546279217,3.50986195899749));
#39583=CARTESIAN_POINT('Ctrl Pts',(17.6626081201538,0.263442460518632,3.50345921706735));
#39584=CARTESIAN_POINT('Ctrl Pts',(17.7103239562167,0.560133202238927,3.95303751636628));
#39585=CARTESIAN_POINT('Ctrl Pts',(17.7580397922795,0.342445005586054,4.44574218699675));
#39586=CARTESIAN_POINT('Ctrl Pts',(17.8057556283423,-0.189715708890181,
4.52911494868296));
#39587=CARTESIAN_POINT('Ctrl Pts',(17.8534714644052,-0.547657568741173,
4.12659331151364));
#39588=CARTESIAN_POINT('Ctrl Pts',(17.901187300468,-0.402677056422281,3.60781908849286));
#39589=CARTESIAN_POINT('Ctrl Pts',(17.9489031365308,0.112087992792125,3.44919063098808));
#39590=CARTESIAN_POINT('Ctrl Pts',(17.9966189725937,0.523920913530056,3.79637889233847));
#39591=CARTESIAN_POINT('Ctrl Pts',(18.0443348086565,0.454629197813879,4.33055554996792));
#39592=CARTESIAN_POINT('Ctrl Pts',(18.0920506447194,-0.0321555056241734,
4.56117795981091));
#39593=CARTESIAN_POINT('Ctrl Pts',(18.1397664807822,-0.489411313471489,
4.27646201432672));
#39594=CARTESIAN_POINT('Ctrl Pts',(18.1874823168451,-0.497233181596917,
3.73786674717144));
#39595=CARTESIAN_POINT('Ctrl Pts',(18.2351981529079,-0.0484381681459794,
3.43999247952716));
#39596=CARTESIAN_POINT('Ctrl Pts',(18.2829139889707,0.444838360430441,3.65638173475637));
#39597=CARTESIAN_POINT('Ctrl Pts',(18.3306298250336,0.529612977905601,4.18832093020544));
#39598=CARTESIAN_POINT('Ctrl Pts',(18.3783456610964,0.128035848626906,4.54732211775687));
#39599=CARTESIAN_POINT('Ctrl Pts',(18.4260614971592,-0.391118570530631,
4.40370898293889));
#39600=CARTESIAN_POINT('Ctrl Pts',(18.4737773332221,-0.551102788237131,
3.88936367722697));
#39601=CARTESIAN_POINT('Ctrl Pts',(18.5214931692849,-0.205000835699102,
3.47661740907615));
#39602=CARTESIAN_POINT('Ctrl Pts',(18.5692090053478,0.329356538604741,3.54450142744705));
#39603=CARTESIAN_POINT('Ctrl Pts',(18.6169248414106,0.561260735706054,4.03067679373969));
#39604=CARTESIAN_POINT('Ctrl Pts',(18.6646406774734,0.2777505631021,4.48868118831814));
#39605=CARTESIAN_POINT('Ctrl Pts',(18.7123565135363,-0.260822225340423,
4.49792212833724));
#39606=CARTESIAN_POINT('Ctrl Pts',(18.7600723495991,-0.559877950986752,
4.04991351638789));
#39607=CARTESIAN_POINT('Ctrl Pts',(18.8077881856619,-0.344789139412875,
3.55606855432066));
#39608=CARTESIAN_POINT('Ctrl Pts',(18.8555040217248,0.186924844147682,3.46989266958543));
#39609=CARTESIAN_POINT('Ctrl Pts',(18.9032198577876,0.546982867117114,3.87052250311704));
#39610=CARTESIAN_POINT('Ctrl Pts',(18.9509356938504,0.404738106803207,4.39005351430856));
#39611=CARTESIAN_POINT('Ctrl Pts',(18.9986515299133,-0.109183884691052,
4.55139238155646));
#39612=CARTESIAN_POINT('Ctrl Pts',(19.0463673659761,-0.522840634850846,
4.20637914057629));
#39613=CARTESIAN_POINT('Ctrl Pts',(19.094083202039,-0.456364785113784,3.67184475922049));
#39614=CARTESIAN_POINT('Ctrl Pts',(19.1417990381018,0.029197868913272,3.43866038485254));
#39615=CARTESIAN_POINT('Ctrl Pts',(19.1895148741647,0.487947670564988,3.72096281627648));
#39616=CARTESIAN_POINT('Ctrl Pts',(19.2372307102275,0.498607618457993,4.25950938727589));
#39617=CARTESIAN_POINT('Ctrl Pts',(19.2849465462903,0.0513885179525073,
4.55974449445321));
#39618=CARTESIAN_POINT('Ctrl Pts',(19.3326623823531,-0.44302144872845,4.34595762039384));
#39619=CARTESIAN_POINT('Ctrl Pts',(19.380378218416,-0.530598003365269,3.81447253878192));
#39620=CARTESIAN_POINT('Ctrl Pts',(19.4280940544788,-0.130918245164485,
3.45336018235082));
#39621=CARTESIAN_POINT('Ctrl Pts',(19.4758098905417,0.38898574814073,3.59423557624425));
#39622=CARTESIAN_POINT('Ctrl Pts',(19.5235257266045,0.551678150913516,4.10773069407674));
#39623=CARTESIAN_POINT('Ctrl Pts',(19.5712415626673,0.207756005258534,4.52229503878775));
#39624=CARTESIAN_POINT('Ctrl Pts',(19.6189573987302,-0.326951650734615,
4.4572278489044));
#39625=CARTESIAN_POINT('Ctrl Pts',(19.666673234793,-0.561414624206118,3.9722812219163));
#39626=CARTESIAN_POINT('Ctrl Pts',(19.7143890708559,-0.280321816997631,
3.51278930393937));
#39627=CARTESIAN_POINT('Ctrl Pts',(19.7621049069187,0.258194652845487,3.5007102220535));
#39628=CARTESIAN_POINT('Ctrl Pts',(19.8098207429815,0.559607330995945,3.94713708427543));
#39629=CARTESIAN_POINT('Ctrl Pts',(19.8575365790444,0.347123361713752,4.44210790974427));
#39630=CARTESIAN_POINT('Ctrl Pts',(19.9052524151072,-0.184128152223511,
4.53108587353909));
#39631=CARTESIAN_POINT('Ctrl Pts',(19.9529682511701,-0.546294178096705,
4.13235642149579));
#39632=CARTESIAN_POINT('Ctrl Pts',(20.0006840872329,-0.406785648814185,
3.61208785870539));
#39633=CARTESIAN_POINT('Ctrl Pts',(20.0483999232957,0.106272459957556,3.44803398021027));
#39634=CARTESIAN_POINT('Ctrl Pts',(20.0961157593586,0.5217539278249,3.7908797683689));
#39635=CARTESIAN_POINT('Ctrl Pts',(20.1438315954214,0.458072423058868,4.32572464996293));
#39636=CARTESIAN_POINT('Ctrl Pts',(20.1915474314842,-0.0262105744965466,
4.56152565902554));
#39637=CARTESIAN_POINT('Ctrl Pts',(20.2392632675471,-0.486524960252488,
4.28152908133109));
#39638=CARTESIAN_POINT('Ctrl Pts',(20.2869791036099,-0.499865224545849,
3.74326461201656));
#39639=CARTESIAN_POINT('Ctrl Pts',(20.3346949396728,-0.0545328049175168,
3.440261547834));
#39640=CARTESIAN_POINT('Ctrl Pts',(20.3824107757356,0.441568512678419,3.6522489094147));
#39641=CARTESIAN_POINT('Ctrl Pts',(20.4221739724547,0.515928418030698,4.09332268501583));
#39642=CARTESIAN_POINT('Ctrl Pts',(20.4539845298298,0.333108474939506,4.36566768059473));
#39643=CARTESIAN_POINT('Ctrl Pts',(20.4778424478613,0.118510552090848,4.48142006140068));
#39644=CARTESIAN_POINT('Ctrl Pts',(20.5017003658927,-0.127372553428812,
4.47887124859312));
#39645=CARTESIAN_POINT('Ctrl Pts',(20.5255582839241,-0.340862259689409,
4.35954554232165));
#39646=CARTESIAN_POINT('Ctrl Pts',(20.5494162019555,-0.471665647836603,
4.15213005589169));
#39647=CARTESIAN_POINT('Ctrl Pts',(20.5732741199869,-0.486782001098211,
3.90760543082941));
#39648=CARTESIAN_POINT('Ctrl Pts',(20.5971320380184,-0.38305332993788,3.68562568155832));
#39649=CARTESIAN_POINT('Ctrl Pts',(20.6209899560498,-0.185558943137764,
3.54054450025879));
#39650=CARTESIAN_POINT('Ctrl Pts',(20.6448478740812,0.0572573647513246,
3.50779920733485));
#39651=CARTESIAN_POINT('Ctrl Pts',(20.6687057921126,0.28610038304352,3.59541756340761));
#39652=CARTESIAN_POINT('Ctrl Pts',(20.6925637101441,0.444969396676924,3.78196356026503));
#39653=CARTESIAN_POINT('Ctrl Pts',(20.7164216281754,0.495039040219165,4.02182741068269));
#39654=CARTESIAN_POINT('Ctrl Pts',(20.7402795462069,0.424054039808096,4.25635280284423));
#39655=CARTESIAN_POINT('Ctrl Pts',(20.7641374642383,0.249378454468877,4.42819351412177));
#39656=CARTESIAN_POINT('Ctrl Pts',(20.7879953822697,0.0137218901755031,
4.49532894963167));
#39657=CARTESIAN_POINT('Ctrl Pts',(20.8118533003011,-0.22528943893053,4.44134312218709));
#39658=CARTESIAN_POINT('Ctrl Pts',(20.8357112183326,-0.409211687104306,
4.27943679589328));
#39659=CARTESIAN_POINT('Ctrl Pts',(20.859569136364,-0.493070359673604,4.04920060553547));
#39660=CARTESIAN_POINT('Ctrl Pts',(20.8834270543954,-0.456359989112496,
3.80693350349834));
#39661=CARTESIAN_POINT('Ctrl Pts',(20.9072849724268,-0.308057122141145,
3.61187643128937));
#39662=CARTESIAN_POINT('Ctrl Pts',(20.9311428904583,-0.0844259229598539,
3.51172613733272));
#39663=CARTESIAN_POINT('Ctrl Pts',(20.9550008084896,0.159849727585384,3.53097210659131));
#39664=CARTESIAN_POINT('Ctrl Pts',(20.9788587265211,0.365037758375503,3.66490817000854));
#39665=CARTESIAN_POINT('Ctrl Pts',(21.0027166445525,0.480964117596,3.88078331455297));
#39666=CARTESIAN_POINT('Ctrl Pts',(21.026574562584,0.479281646861755,4.12581018556955));
#39667=CARTESIAN_POINT('Ctrl Pts',(21.0504324806153,0.360401759160676,4.34007303948752));
#39668=CARTESIAN_POINT('Ctrl Pts',(21.0742903986468,0.153393823636192,4.47117877170218));
#39669=CARTESIAN_POINT('Ctrl Pts',(21.0981483166782,-0.0911230798336762,
4.48706845966041));
#39670=CARTESIAN_POINT('Ctrl Pts',(21.1220062347096,-0.313357908298923,
4.38385664171252));
#39671=CARTESIAN_POINT('Ctrl Pts',(21.145864152741,-0.458968192403581,4.18678141884249));
#39672=CARTESIAN_POINT('Ctrl Pts',(21.1697220707724,-0.492348251467217,
3.94403305123036));
#39673=CARTESIAN_POINT('Ctrl Pts',(21.1935799888039,-0.405335751726616,
3.71497012710753));
#39674=CARTESIAN_POINT('Ctrl Pts',(21.2174379068353,-0.21920761957706,3.55560477096155));
#39675=CARTESIAN_POINT('Ctrl Pts',(21.2412958248667,0.0205227466613194,
3.50490615340017));
#39676=CARTESIAN_POINT('Ctrl Pts',(21.2651537428981,0.255234742309135,3.57527146741714));
#39677=CARTESIAN_POINT('Ctrl Pts',(21.2890116609295,0.427534891009427,3.74949447702405));
#39678=CARTESIAN_POINT('Ctrl Pts',(21.312869578961,0.495291113040325,3.98497291063177));
#39679=CARTESIAN_POINT('Ctrl Pts',(21.3367274969923,0.441935166474334,4.22412587691986));
#39680=CARTESIAN_POINT('Ctrl Pts',(21.3605854150238,0.280514033632862,4.40847396123464));
#39681=CARTESIAN_POINT('Ctrl Pts',(21.3844433330552,0.0504995785194436,
4.49293903542029));
#39682=CARTESIAN_POINT('Ctrl Pts',(21.4083012510867,-0.191863399122956,
4.45686708805594));
#39683=CARTESIAN_POINT('Ctrl Pts',(21.432159169118,-0.387310549425693,4.3090786928523));
#39684=CARTESIAN_POINT('Ctrl Pts',(21.4560170871495,-0.488049720266331,
4.08571213811173));
#39685=CARTESIAN_POINT('Ctrl Pts',(21.4798750051809,-0.469447440294381,
3.84138663085107));
#39686=CARTESIAN_POINT('Ctrl Pts',(21.5037329232123,-0.336052473678932,
3.63584641288874));
#39687=CARTESIAN_POINT('Ctrl Pts',(21.5275908412437,-0.120483523363382,
3.51935166631968));
#39688=CARTESIAN_POINT('Ctrl Pts',(21.5514487592752,0.124546930319796,3.5203885299332));
#39689=CARTESIAN_POINT('Ctrl Pts',(21.5753066773065,0.339122266949511,3.63870346233219));
#39690=CARTESIAN_POINT('Ctrl Pts',(21.599164595338,0.470772971804989,3.84536523971104));
#39691=CARTESIAN_POINT('Ctrl Pts',(21.6230225133694,0.487306861455871,4.08983942814686));
#39692=CARTESIAN_POINT('Ctrl Pts',(21.6468804314008,0.384680949508402,4.31234542922385));
#39693=CARTESIAN_POINT('Ctrl Pts',(21.6707383494323,0.187990066907445,4.45847446473699));
#39694=CARTESIAN_POINT('Ctrl Pts',(21.6945962674636,-0.0546695077989956,
4.49249400502822));
#39695=CARTESIAN_POINT('Ctrl Pts',(21.7184541854951,-0.283960898681086,
4.40608534582272));
#39696=CARTESIAN_POINT('Ctrl Pts',(21.7423121035264,-0.443816114896065,
4.22037775802082));
#39697=CARTESIAN_POINT('Ctrl Pts',(21.766170021558,-0.495146201710716,3.98078180541326));
#39698=CARTESIAN_POINT('Ctrl Pts',(21.7900279395893,-0.425399554695369,
3.74588522487523));
#39699=CARTESIAN_POINT('Ctrl Pts',(21.8138858576208,-0.25163112890579,3.57312662880273));
#39700=CARTESIAN_POINT('Ctrl Pts',(21.8377437756521,-0.0163320378044167,
3.50475019978512));
#39701=CARTESIAN_POINT('Ctrl Pts',(21.8616016936836,0.222960681415914,3.55747583725374));
#39702=CARTESIAN_POINT('Ctrl Pts',(21.885459611715,0.407733440703041,3.71841068663001));
#39703=CARTESIAN_POINT('Ctrl Pts',(21.9093175297464,0.492804267302335,3.94820179346412));
#39704=CARTESIAN_POINT('Ctrl Pts',(21.9331754477779,0.457371026827486,4.19065897275109));
#39705=CARTESIAN_POINT('Ctrl Pts',(21.9570333658092,0.310098111756678,4.38649483975425));
#39706=CARTESIAN_POINT('Ctrl Pts',(21.9808912838407,0.0869977614584207,
4.48782219052945));
#39707=CARTESIAN_POINT('Ctrl Pts',(22.0047492018721,-0.15737591128791,4.46986372771052));
#39708=CARTESIAN_POINT('Ctrl Pts',(22.0286071199035,-0.363266886890503,
4.33701078463543));
#39709=CARTESIAN_POINT('Ctrl Pts',(22.0524650379349,-0.480329213457224,
4.12174952472744));
#39710=CARTESIAN_POINT('Ctrl Pts',(22.0763229559664,-0.479937963428243,
3.87671718963328));
#39711=CARTESIAN_POINT('Ctrl Pts',(22.1001808739978,-0.362188808094022,
3.66183085982978));
#39712=CARTESIAN_POINT('Ctrl Pts',(22.1240387920292,-0.155874623354616,
3.529636096341));
#39713=CARTESIAN_POINT('Ctrl Pts',(22.1478967100606,0.0885551527323001,
3.51245811975107));
#39714=CARTESIAN_POINT('Ctrl Pts',(22.1717546280921,0.311330781786364,3.61449741325855));
#39715=CARTESIAN_POINT('Ctrl Pts',(22.1956125461234,0.457977554205651,3.81080259009947));
#39716=CARTESIAN_POINT('Ctrl Pts',(22.2194704641549,0.492636339578261,4.05337168730347));
#39717=CARTESIAN_POINT('Ctrl Pts',(22.2433283821863,0.406832120751761,4.28288995313029));
#39718=CARTESIAN_POINT('Ctrl Pts',(22.2671863002177,0.22154636656941,4.44323391967918));
#39719=CARTESIAN_POINT('Ctrl Pts',(22.2910442182491,-0.0179135091400202,
4.49519511936025));
#39720=CARTESIAN_POINT('Ctrl Pts',(22.3149021362805,-0.2529930437236,4.42606762362056));
#39721=CARTESIAN_POINT('Ctrl Pts',(22.338760054312,-0.426208888077552,4.25275498785448));
#39722=CARTESIAN_POINT('Ctrl Pts',(22.3626179723434,-0.495205048933098,
4.01763687303198));
#39723=CARTESIAN_POINT('Ctrl Pts',(22.3864758903748,-0.443110087468167,
3.77820606161377));
#39724=CARTESIAN_POINT('Ctrl Pts',(22.4103338084062,-0.282662637164788,
3.59300991103726));
#39725=CARTESIAN_POINT('Ctrl Pts',(22.4341917264377,-0.0530964769854286,
3.50733392083031));
#39726=CARTESIAN_POINT('Ctrl Pts',(22.458049644469,0.189453226607198,3.5421282117862));
#39727=CARTESIAN_POINT('Ctrl Pts',(22.4819075625005,0.385676439696491,3.6888846179772));
#39728=CARTESIAN_POINT('Ctrl Pts',(22.5057654805319,0.487591287867653,3.9117172269821));
#39729=CARTESIAN_POINT('Ctrl Pts',(22.5296233985634,0.470276727405835,4.15613734610506));
#39730=CARTESIAN_POINT('Ctrl Pts',(22.5534813165947,0.337966804695391,4.36237769267677));
#39731=CARTESIAN_POINT('Ctrl Pts',(22.5773392346262,0.123014588878675,4.48000670597833));
#39732=CARTESIAN_POINT('Ctrl Pts',(22.6011971526576,-0.122017660845505,
4.48026122441149));
#39733=CARTESIAN_POINT('Ctrl Pts',(22.625055070689,-0.337213993725473,4.36307837627545));
#39734=CARTESIAN_POINT('Ctrl Pts',(22.6489129887204,-0.469950950795418,
4.15711375897153));
#39735=CARTESIAN_POINT('Ctrl Pts',(22.6727709067518,-0.487774683880463,
3.912729067726));
#39736=CARTESIAN_POINT('Ctrl Pts',(22.6966288247832,-0.386319338946922,
3.6896872918462));
#39737=CARTESIAN_POINT('Ctrl Pts',(22.7204867428147,-0.190407614498503,
3.54252014522276));
#39738=CARTESIAN_POINT('Ctrl Pts',(22.7443446608461,0.0520814161336476,
3.50722927763546));
#39739=CARTESIAN_POINT('Ctrl Pts',(22.7682025788775,0.281801791424649,3.59241522467272));
#39740=CARTESIAN_POINT('Ctrl Pts',(22.7920604969089,0.442679857002608,3.77730419914427));
#39741=CARTESIAN_POINT('Ctrl Pts',(22.8079657755965,0.477669651496365,3.93681187972983));
#39742=CARTESIAN_POINT('Ctrl Pts',(22.8159184149403,0.475016281724327,4.01593044384941));
#39743=CARTESIAN_POINT('Ctrl Pts',(3.98408158505964,0.229225853138217,4.48306385360099));
#39744=CARTESIAN_POINT('Ctrl Pts',(3.99203422440344,0.148766887950233,4.52124364039387));
#39745=CARTESIAN_POINT('Ctrl Pts',(4.00793950309106,-0.0315132651739855,
4.55658776856145));
#39746=CARTESIAN_POINT('Ctrl Pts',(4.03179742112247,-0.29437836981663,4.47338935048851));
#39747=CARTESIAN_POINT('Ctrl Pts',(4.0556553391539,-0.485191777607318,4.27448557757091));
#39748=CARTESIAN_POINT('Ctrl Pts',(4.07951325718531,-0.557397168683185,
4.00843674174317));
#39749=CARTESIAN_POINT('Ctrl Pts',(4.10337117521674,-0.493285636019562,
3.74033843218029));
#39750=CARTESIAN_POINT('Ctrl Pts',(4.12722909324815,-0.308561908987092,
3.53572729771651));
#39751=CARTESIAN_POINT('Ctrl Pts',(4.15108701127957,-0.0483813190761145,
3.44464727048097));
#39752=CARTESIAN_POINT('Ctrl Pts',(4.17494492931099,0.223627135909104,3.48936410886239));
#39753=CARTESIAN_POINT('Ctrl Pts',(4.19880284734241,0.440954086798485,3.65894639349553));
#39754=CARTESIAN_POINT('Ctrl Pts',(4.22266076537383,0.55045499896491,3.91192501290154));
#39755=CARTESIAN_POINT('Ctrl Pts',(4.24651868340524,0.525355068663259,4.18644066347397));
#39756=CARTESIAN_POINT('Ctrl Pts',(4.27037660143667,0.371791302444591,4.41536633561891));
#39757=CARTESIAN_POINT('Ctrl Pts',(4.29423451946808,0.127314547262185,4.54272370785395));
#39758=CARTESIAN_POINT('Ctrl Pts',(4.31809243749951,-0.14829414195428,4.5373703057994));
#39759=CARTESIAN_POINT('Ctrl Pts',(4.34195035553092,-0.387640842632661,
4.40061524972397));
#39760=CARTESIAN_POINT('Ctrl Pts',(4.36580827356235,-0.53219881478122,4.16589884014724));
#39761=CARTESIAN_POINT('Ctrl Pts',(4.38966619159376,-0.546619671109945,
3.89061565172978));
#39762=CARTESIAN_POINT('Ctrl Pts',(4.41352410962518,-0.427377132892538,
3.64207991255526));
#39763=CARTESIAN_POINT('Ctrl Pts',(4.4373820276566,-0.203629241694984,3.48106538615089));
#39764=CARTESIAN_POINT('Ctrl Pts',(4.46123994568802,0.0699115445388116,
3.44694450735191));
#39765=CARTESIAN_POINT('Ctrl Pts',(4.48509786371944,0.326357054473012,3.54806076195131));
#39766=CARTESIAN_POINT('Ctrl Pts',(4.50895578175085,0.502999374434197,3.7596884705576));
#39767=CARTESIAN_POINT('Ctrl Pts',(4.53281369978229,0.556644646112557,4.03007889421215));
#39768=CARTESIAN_POINT('Ctrl Pts',(4.55667161781369,0.474175139017821,4.29311420882242));
#39769=CARTESIAN_POINT('Ctrl Pts',(4.58052953584512,0.275756894216243,4.48447511514554));
#39770=CARTESIAN_POINT('Ctrl Pts',(4.60438745387653,0.00990857728296194,
4.55736865895685));
#39771=CARTESIAN_POINT('Ctrl Pts',(4.62824537190795,-0.258362656684952,
4.49397038324719));
#39772=CARTESIAN_POINT('Ctrl Pts',(4.65210328993938,-0.463457183444019,
4.30978289334447));
#39773=CARTESIAN_POINT('Ctrl Pts',(4.67596120797079,-0.555223804526532,
4.04984504770563));
#39774=CARTESIAN_POINT('Ctrl Pts',(4.69981912600221,-0.511223081411799,
3.77771873014923));
#39775=CARTESIAN_POINT('Ctrl Pts',(4.72367704403363,-0.342214389453536,
3.55994623789246));
#39776=CARTESIAN_POINT('Ctrl Pts',(4.74753496206505,-0.0895249575417115,
3.44977887729433));
#39777=CARTESIAN_POINT('Ctrl Pts',(4.77139288009647,0.185055765100279,3.47415556892044));
#39778=CARTESIAN_POINT('Ctrl Pts',(4.79525079812788,0.414385312357242,3.62711554766008));
#39779=CARTESIAN_POINT('Ctrl Pts',(4.81910871615931,0.542386363113676,3.87125593216545));
#39780=CARTESIAN_POINT('Ctrl Pts',(4.84296663419071,0.537759173780872,4.14687774817434));
#39781=CARTESIAN_POINT('Ctrl Pts',(4.86682455222215,0.401635218192884,4.38658395388507));
#39782=CARTESIAN_POINT('Ctrl Pts',(4.89068247025356,0.167300511433038,4.53175985253543));
#39783=CARTESIAN_POINT('Ctrl Pts',(4.91454038828499,-0.107943727546613,
4.54690598239331));
#39784=CARTESIAN_POINT('Ctrl Pts',(4.9383983063164,-0.356792784813018,4.42831870213619));
#39785=CARTESIAN_POINT('Ctrl Pts',(4.96225622434782,-0.518396287352312,
4.20499583203957));
#39786=CARTESIAN_POINT('Ctrl Pts',(4.98611414237924,-0.553237776802617,
3.93154589703492));
#39787=CARTESIAN_POINT('Ctrl Pts',(5.00997206041066,-0.452797559930213,
3.67483485485756));
#39788=CARTESIAN_POINT('Ctrl Pts',(5.03382997844208,-0.241636005696979,
3.49763554798826));
#39789=CARTESIAN_POINT('Ctrl Pts',(5.05768789647349,0.0286121339618079,
3.44327803376872));
#39790=CARTESIAN_POINT('Ctrl Pts',(5.08154581450492,0.291863827488053,3.52505420509465));
#39791=CARTESIAN_POINT('Ctrl Pts',(5.10540373253633,0.48374686498243,3.72296756053861));
#39792=CARTESIAN_POINT('Ctrl Pts',(5.12926165056775,0.557340616988569,3.98862289364304));
#39793=CARTESIAN_POINT('Ctrl Pts',(5.15311956859917,0.49464940648741,4.25706023915787));
#39794=CARTESIAN_POINT('Ctrl Pts',(5.17697748663059,0.311002942120779,4.46263935401832));
#39795=CARTESIAN_POINT('Ctrl Pts',(5.20083540466201,0.0513077868555636,
4.55509054477827));
#39796=CARTESIAN_POINT('Ctrl Pts',(5.22469332269342,-0.22093351989189,4.5118069769771));
#39797=CARTESIAN_POINT('Ctrl Pts',(5.24855124072485,-0.439150562917527,
4.34337266196288));
#39798=CARTESIAN_POINT('Ctrl Pts',(5.27240915875626,-0.549983331088669,
4.09097437781523));
#39799=CARTESIAN_POINT('Ctrl Pts',(5.29626707678769,-0.526330193563486,
3.81633038019944));
#39800=CARTESIAN_POINT('Ctrl Pts',(5.32012499481911,-0.373974986765411,
3.5865986076849));
#39801=CARTESIAN_POINT('Ctrl Pts',(5.34398291285052,-0.130172708829089,
3.45795473641922));
#39802=CARTESIAN_POINT('Ctrl Pts',(5.36784083088195,0.145460342249349,3.46185569711558));
#39803=CARTESIAN_POINT('Ctrl Pts',(5.39169874891335,0.385524377387638,3.59734759862366));
#39804=CARTESIAN_POINT('Ctrl Pts',(5.41555666694479,0.531317200781484,3.83129898029949));
#39805=CARTESIAN_POINT('Ctrl Pts',(5.4394145849762,0.547188495794237,4.10650235661553));
#39806=CARTESIAN_POINT('Ctrl Pts',(5.46327250300762,0.42925729847004,4.35566300567327));
#39807=CARTESIAN_POINT('Ctrl Pts',(5.48713042103904,0.206360998935678,4.51785436177788));
#39808=CARTESIAN_POINT('Ctrl Pts',(5.51098833907045,-0.0669961859988386,
4.55341622035867));
#39809=CARTESIAN_POINT('Ctrl Pts',(5.53484625710188,-0.323970978517869,
4.45365273830571));
#39810=CARTESIAN_POINT('Ctrl Pts',(5.55870417513329,-0.501726041995696,
4.2429588044862));
#39811=CARTESIAN_POINT('Ctrl Pts',(5.58256209316472,-0.556795421465071,
3.97285482490167));
#39812=CARTESIAN_POINT('Ctrl Pts',(5.60642001119613,-0.475713153578786,
3.70938858005442));
#39813=CARTESIAN_POINT('Ctrl Pts',(5.63027792922756,-0.27830606148521,3.51698474346866));
#39814=CARTESIAN_POINT('Ctrl Pts',(5.65413584725897,-0.0128455564368745,
3.44269129419766));
#39815=CARTESIAN_POINT('Ctrl Pts',(5.67799376529039,0.255756037034639,3.5046750042392));
#39816=CARTESIAN_POINT('Ctrl Pts',(5.70185168332181,0.46181831285622,3.68777916820271));
#39817=CARTESIAN_POINT('Ctrl Pts',(5.72570960135323,0.554953431393631,3.94722983012095));
#39818=CARTESIAN_POINT('Ctrl Pts',(5.74956751938465,0.512387319539865,4.21958423627784));
#39819=CARTESIAN_POINT('Ctrl Pts',(5.77342543741606,0.344528550506956,4.43824431479549));
#39820=CARTESIAN_POINT('Ctrl Pts',(5.79728335544749,0.0924231668635294,
4.54974172178225));
#39821=CARTESIAN_POINT('Ctrl Pts',(5.82114127347891,-0.182282200065281,
4.52681230129395));
#39822=CARTESIAN_POINT('Ctrl Pts',(5.84499919151032,-0.412414601109181,
4.37506292652603));
#39823=CARTESIAN_POINT('Ctrl Pts',(5.86885710954175,-0.541700403334708,
4.13160044316952));
#39824=CARTESIAN_POINT('Ctrl Pts',(5.89271502757316,-0.538525691690445,
3.85595807909033));
#39825=CARTESIAN_POINT('Ctrl Pts',(5.91657294560459,-0.403666797469215,
3.61553786496538));
#39826=CARTESIAN_POINT('Ctrl Pts',(5.94043086363599,-0.170100341263849,
3.46912915944898));
#39827=CARTESIAN_POINT('Ctrl Pts',(5.96428878166742,0.105060216979666,3.45253275189516));
#39828=CARTESIAN_POINT('Ctrl Pts',(5.98814669969884,0.354530812822036,3.5698071562788));
#39829=CARTESIAN_POINT('Ctrl Pts',(6.01200461773026,0.517308736525128,3.79227513259484));
#39830=CARTESIAN_POINT('Ctrl Pts',(6.03586253576167,0.553591019453439,4.06553805729756));
#39831=CARTESIAN_POINT('Ctrl Pts',(6.0597204537931,0.454504394384077,4.32277408438697));
#39832=CARTESIAN_POINT('Ctrl Pts',(6.08357837182452,0.244280620740535,4.50108505220882));
#39833=CARTESIAN_POINT('Ctrl Pts',(6.10743628985593,-0.0256793573627324,
4.55686330558177));
#39834=CARTESIAN_POINT('Ctrl Pts',(6.13129420788736,-0.289354484390735,
4.47648043042773));
#39835=CARTESIAN_POINT('Ctrl Pts',(6.15515212591877,-0.482285035214929,
4.27957167009689));
#39836=CARTESIAN_POINT('Ctrl Pts',(6.17901004395019,-0.557263974895364,
4.01432540012922));
#39837=CARTESIAN_POINT('Ctrl Pts',(6.20286796198161,-0.496014047041978,
3.74552825888183));
#39838=CARTESIAN_POINT('Ctrl Pts',(6.22672588001303,-0.313404643062,3.53904687299508));
#39839=CARTESIAN_POINT('Ctrl Pts',(6.25058379804445,-0.0542924323345977,
3.44511024149985));
#39840=CARTESIAN_POINT('Ctrl Pts',(6.27444171607587,0.218347115212216,3.48718178027374));
#39841=CARTESIAN_POINT('Ctrl Pts',(6.29829963410728,0.437120926894882,3.65404298137615));
#39842=CARTESIAN_POINT('Ctrl Pts',(6.32215755213871,0.549895923261456,3.90664388593688));
#39843=CARTESIAN_POINT('Ctrl Pts',(6.34601547017011,0.526573903738089,4.17995327069166));
#39844=CARTESIAN_POINT('Ctrl Pts',(6.37782602754536,0.327418726170013,4.4906154426808));
#39845=CARTESIAN_POINT('Ctrl Pts',(6.41758922426438,-0.161063729547888,
4.61146011675295));
#39846=CARTESIAN_POINT('Ctrl Pts',(6.46530506032721,-0.60205854017139,4.19446204504257));
#39847=CARTESIAN_POINT('Ctrl Pts',(6.51302089639007,-0.488859252747234,
3.59916283817905));
#39848=CARTESIAN_POINT('Ctrl Pts',(6.56073673245289,0.0725864685289804,
3.37181094029106));
#39849=CARTESIAN_POINT('Ctrl Pts',(6.60845256851574,0.567733426150434,3.72141305678318));
#39850=CARTESIAN_POINT('Ctrl Pts',(6.65616840457857,0.541332409494817,4.32680434473755));
#39851=CARTESIAN_POINT('Ctrl Pts',(6.70388424064141,0.0179179137367747,
4.6321081579338));
#39852=CARTESIAN_POINT('Ctrl Pts',(6.75160007670425,-0.522004047715759,
4.35692568061372));
#39853=CARTESIAN_POINT('Ctrl Pts',(6.79931591276708,-0.582533501572452,
3.75397902491298));
#39854=CARTESIAN_POINT('Ctrl Pts',(6.84703174882993,-0.10812839031349,3.37695395054049));
#39855=CARTESIAN_POINT('Ctrl Pts',(6.89474758489276,0.465580583415614,3.57208337966475));
#39856=CARTESIAN_POINT('Ctrl Pts',(6.9424634209556,0.611735560770294,4.16017430964564));
#39857=CARTESIAN_POINT('Ctrl Pts',(6.99017925701844,0.196126575106773,4.60117519156627));
#39858=CARTESIAN_POINT('Ctrl Pts',(7.03789509308127,-0.399589635450545,
4.49010738789885));
#39859=CARTESIAN_POINT('Ctrl Pts',(7.08561092914412,-0.628355913977057,
3.92896656470948));
#39860=CARTESIAN_POINT('Ctrl Pts',(7.13332676520695,-0.280093617253323,
3.43305676608093));
#39861=CARTESIAN_POINT('Ctrl Pts',(7.1810426012698,0.325383132256395,3.45777970086456));
#39862=CARTESIAN_POINT('Ctrl Pts',(7.22875843733263,0.632055452459012,3.98043185926557));
#39863=CARTESIAN_POINT('Ctrl Pts',(7.27647427339546,0.358301574124045,4.52105375310108));
#39864=CARTESIAN_POINT('Ctrl Pts',(7.32419010945831,-0.244486178793781,
4.58318396235269));
#39865=CARTESIAN_POINT('Ctrl Pts',(7.37190594552114,-0.622758498112341,
4.10976736853928));
#39866=CARTESIAN_POINT('Ctrl Pts',(7.41962178158399,-0.42914211350377,3.53554970961824));
#39867=CARTESIAN_POINT('Ctrl Pts',(7.46733761764681,0.158562080980748,3.38784389968312));
#39868=CARTESIAN_POINT('Ctrl Pts',(7.51505345370967,0.600656274672958,3.80229045545538));
#39869=CARTESIAN_POINT('Ctrl Pts',(7.56276928977248,0.491158570126743,4.3982967283715));
#39870=CARTESIAN_POINT('Ctrl Pts',(7.61048512583535,-0.0693776073840611,
4.62854098691609));
#39871=CARTESIAN_POINT('Ctrl Pts',(7.65820096189817,-0.566203260219877,
4.28158638589565));
#39872=CARTESIAN_POINT('Ctrl Pts',(7.70591679796101,-0.543075747198986,
3.67604667390869));
#39873=CARTESIAN_POINT('Ctrl Pts',(7.75363263402386,-0.0212334191459514,
3.36799828595259));
#39874=CARTESIAN_POINT('Ctrl Pts',(7.80134847008666,0.520107884382028,3.64032679659274));
#39875=CARTESIAN_POINT('Ctrl Pts',(7.84906430614954,0.583826114817312,4.24294874421058));
#39876=CARTESIAN_POINT('Ctrl Pts',(7.89678014221235,0.111407840683781,4.62246712177016));
#39877=CARTESIAN_POINT('Ctrl Pts',(7.94449597827521,-0.463317967772962,
4.43036436352186));
#39878=CARTESIAN_POINT('Ctrl Pts',(7.99221181433803,-0.612571757364041,
3.84305138824375));
#39879=CARTESIAN_POINT('Ctrl Pts',(8.03992765040088,-0.199291476537812,
3.39986673810663));
#39880=CARTESIAN_POINT('Ctrl Pts',(8.08764348646372,0.397001233685627,3.50779369660314));
#39881=CARTESIAN_POINT('Ctrl Pts',(8.13535932252656,0.628721602366905,4.06772127707659));
#39882=CARTESIAN_POINT('Ctrl Pts',(8.18307515858938,0.283077249469033,4.56545936678474));
#39883=CARTESIAN_POINT('Ctrl Pts',(8.23079099465223,-0.32252129731946,4.54392741926377));
#39884=CARTESIAN_POINT('Ctrl Pts',(8.27850683071506,-0.631943574151527,
4.02289855323374));
#39885=CARTESIAN_POINT('Ctrl Pts',(8.32622266677791,-0.361042343138453,
3.48084159342964));
#39886=CARTESIAN_POINT('Ctrl Pts',(8.37393850284074,0.241409626929164,3.41553578665797));
#39887=CARTESIAN_POINT('Ctrl Pts',(8.42165433890358,0.622171422023167,3.88695246013618));
#39888=CARTESIAN_POINT('Ctrl Pts',(8.46937017496642,0.431583626935426,4.46218242893131));
#39889=CARTESIAN_POINT('Ctrl Pts',(8.51708601102927,-0.155334053534803,
4.61298316164806));
#39890=CARTESIAN_POINT('Ctrl Pts',(8.56480184709209,-0.599606082522386,
4.20087202506506));
#39891=CARTESIAN_POINT('Ctrl Pts',(8.61251768315494,-0.493250619804184,
3.60429701705146));
#39892=CARTESIAN_POINT('Ctrl Pts',(8.66023351921777,0.0660644767165412,
3.37110214695249));
#39893=CARTESIAN_POINT('Ctrl Pts',(8.70794935528061,0.564711547735832,3.71543385214437));
#39894=CARTESIAN_POINT('Ctrl Pts',(8.75566519134344,0.544775315265253,4.32108702952508));
#39895=CARTESIAN_POINT('Ctrl Pts',(8.80338102740629,0.0245635283409047,
4.6318810471339));
#39896=CARTESIAN_POINT('Ctrl Pts',(8.85109686346912,-0.518205324617361,
4.36240897642002));
#39897=CARTESIAN_POINT('Ctrl Pts',(8.89881269953197,-0.585098254365674,
3.76013116628075));
#39898=CARTESIAN_POINT('Ctrl Pts',(8.9465285355948,-0.114686454236133,3.3781285970023));
#39899=CARTESIAN_POINT('Ctrl Pts',(8.99424437165764,0.461043681496376,3.56720010581811));
#39900=CARTESIAN_POINT('Ctrl Pts',(9.04196020772047,0.613390310441866,4.15371841694351));
#39901=CARTESIAN_POINT('Ctrl Pts',(9.08967604378332,0.202451179085494,4.59907474052783));
#39902=CARTESIAN_POINT('Ctrl Pts',(9.13739187984615,-0.394401985136886,
4.49429151193569));
#39903=CARTESIAN_POINT('Ctrl Pts',(9.18510771590899,-0.629069737753471,
3.93559278228048));
#39904=CARTESIAN_POINT('Ctrl Pts',(9.23282355197184,-0.28605307070895,3.43604019168954));
#39905=CARTESIAN_POINT('Ctrl Pts',(9.28053938803466,0.319650532659854,3.45438057070715));
#39906=CARTESIAN_POINT('Ctrl Pts',(9.32825522409751,0.631814133431458,3.97377166707843));
#39907=CARTESIAN_POINT('Ctrl Pts',(9.37597106016033,0.363773093762905,4.51724864514637));
#39908=CARTESIAN_POINT('Ctrl Pts',(9.4236868962232,-0.238326375276645,4.58572823348297));
#39909=CARTESIAN_POINT('Ctrl Pts',(9.47140273228601,-0.621567066777005,
4.11632457242483));
#39910=CARTESIAN_POINT('Ctrl Pts',(9.51911856834886,-0.434013156817378,
3.54009826662536));
#39911=CARTESIAN_POINT('Ctrl Pts',(9.5668344044117,0.152101713198456,3.38620679908157));
#39912=CARTESIAN_POINT('Ctrl Pts',(9.61455024047453,0.598539239598464,3.79597107236355));
#39913=CARTESIAN_POINT('Ctrl Pts',(9.66226607653739,0.495328972565208,4.39309824928265));
#39914=CARTESIAN_POINT('Ctrl Pts',(9.7099819126002,-0.0627495115905886,
4.62923725529147));
#39915=CARTESIAN_POINT('Ctrl Pts',(9.75769774866305,-0.563204153727404,
4.28753800770644));
#39916=CARTESIAN_POINT('Ctrl Pts',(9.80541358472588,-0.54645975548653,3.68178818330365));
#39917=CARTESIAN_POINT('Ctrl Pts',(9.85312942078873,-0.027892955418244,
3.36825716649128));
#39918=CARTESIAN_POINT('Ctrl Pts',(9.90084525685157,0.516288374798902,3.63486531430293));
#39919=CARTESIAN_POINT('Ctrl Pts',(9.9485610929144,0.58635414632045,4.2367822623095));
#39920=CARTESIAN_POINT('Ctrl Pts',(9.99627692897723,0.117961883057689,4.62125841547385));
#39921=CARTESIAN_POINT('Ctrl Pts',(10.0439927650401,-0.458756592493822,
4.4352234064191));
#39922=CARTESIAN_POINT('Ctrl Pts',(10.0917086011029,-0.614191830280748,
3.8495160464768));
#39923=CARTESIAN_POINT('Ctrl Pts',(10.1394244371658,-0.205605259764808,
3.40200041654811));
#39924=CARTESIAN_POINT('Ctrl Pts',(10.1871402732286,0.391791784436726,3.5036370055096));
#39925=CARTESIAN_POINT('Ctrl Pts',(10.2348561092915,0.629400404498524,4.06109136983801));
#39926=CARTESIAN_POINT('Ctrl Pts',(10.2825719453542,0.289020948539269,4.56244458923262));
#39927=CARTESIAN_POINT('Ctrl Pts',(10.3302877814171,-0.316770891622519,
4.54729628801251));
#39928=CARTESIAN_POINT('Ctrl Pts',(10.3780036174799,-0.631667147860668,
4.02955738427466));
#39929=CARTESIAN_POINT('Ctrl Pts',(10.4257194535428,-0.366493742769977,
3.48467547975859));
#39930=CARTESIAN_POINT('Ctrl Pts',(10.4734352896056,0.235236505537468,3.41302401146715));
#39931=CARTESIAN_POINT('Ctrl Pts',(10.5211511256685,0.620945451230968,3.88040162523195));
#39932=CARTESIAN_POINT('Ctrl Pts',(10.5688669617313,0.436430634585191,4.45760826680378));
#39933=CARTESIAN_POINT('Ctrl Pts',(10.6165827977941,-0.148865149148659,
4.61458619576145));
#39934=CARTESIAN_POINT('Ctrl Pts',(10.664298633857,-0.597455775834545,4.20718016452724));
#39935=CARTESIAN_POINT('Ctrl Pts',(10.7120144699198,-0.497393570532806,
3.60951740033105));
#39936=CARTESIAN_POINT('Ctrl Pts',(10.7597303059826,0.059432803973042,3.37044081575797));
#39937=CARTESIAN_POINT('Ctrl Pts',(10.8074461420455,0.56168112009921,3.70949811708754));
#39938=CARTESIAN_POINT('Ctrl Pts',(10.8551619781083,0.548129021063343,4.31532776744164));
#39939=CARTESIAN_POINT('Ctrl Pts',(10.9028778141712,0.0312216079359222,
4.63158707701274));
#39940=CARTESIAN_POINT('Ctrl Pts',(10.950593650234,-0.514357088165242,4.36785025554668));
#39941=CARTESIAN_POINT('Ctrl Pts',(10.9983094862968,-0.587593755803164,
3.7663108843084));
#39942=CARTESIAN_POINT('Ctrl Pts',(11.0460253223597,-0.12123403619496,3.37937182377895));
#39943=CARTESIAN_POINT('Ctrl Pts',(11.0937411584225,0.456456764276497,3.56236516706526));
#39944=CARTESIAN_POINT('Ctrl Pts',(11.1414569944854,0.61497629462275,4.14724531131301));
#39945=CARTESIAN_POINT('Ctrl Pts',(11.1891728305482,0.208753630990335,4.59690782052167));
#39946=CARTESIAN_POINT('Ctrl Pts',(11.236888666611,-0.389170704067994,4.49842069353791));
#39947=CARTESIAN_POINT('Ctrl Pts',(11.2846045026739,-0.629713593419695,
3.94222617449013));
#39948=CARTESIAN_POINT('Ctrl Pts',(11.3323203387367,-0.291980800545002,
3.43908624837263));
#39949=CARTESIAN_POINT('Ctrl Pts',(11.3800361747996,0.313882454172263,3.45104205114199));
#39950=CARTESIAN_POINT('Ctrl Pts',(11.4277520108624,0.631502621520784,3.96711438515144));
#39951=CARTESIAN_POINT('Ctrl Pts',(11.4754678469252,0.369204214609944,4.51338608528654));
#39952=CARTESIAN_POINT('Ctrl Pts',(11.5231836829881,-0.232140103514266,
4.58820744384271));
#39953=CARTESIAN_POINT('Ctrl Pts',(11.5708995190509,-0.620306592646703,
4.12286885598323));
#39954=CARTESIAN_POINT('Ctrl Pts',(11.6186153551137,-0.438835993107895,
3.54469790709399));
#39955=CARTESIAN_POINT('Ctrl Pts',(11.6663311911766,0.145624451261577,3.38463787584353));
#39956=CARTESIAN_POINT('Ctrl Pts',(11.7140470272394,0.596355721317347,3.78967435176932));
#39957=CARTESIAN_POINT('Ctrl Pts',(11.7617628633022,0.499444356375145,4.38785610674141));
#39958=CARTESIAN_POINT('Ctrl Pts',(11.8094786993651,-0.0561144459655822,
4.62986363095956));
#39959=CARTESIAN_POINT('Ctrl Pts',(11.8571945354279,-0.560142489144378,
4.29345769116983));
#39960=CARTESIAN_POINT('Ctrl Pts',(11.9049103714908,-0.549783065641843,
3.68756503815187));
#39961=CARTESIAN_POINT('Ctrl Pts',(11.9526262075536,-0.0345493934605723,
3.36858621802886));
#39962=CARTESIAN_POINT('Ctrl Pts',(12.0003420436164,0.512411518346294,3.62944438943981));
#39963=CARTESIAN_POINT('Ctrl Pts',(12.0480578796793,0.588817048391095,4.23058947975914));
#39964=CARTESIAN_POINT('Ctrl Pts',(12.0957737157421,0.1245028227835,4.61998070274044));
#39965=CARTESIAN_POINT('Ctrl Pts',(12.1434895518049,-0.454144260708352,
4.44003410676589));
#39966=CARTESIAN_POINT('Ctrl Pts',(12.1912053878678,-0.615743681684068,
3.85599741975318));
#39967=CARTESIAN_POINT('Ctrl Pts',(12.2389212239306,-0.211896205334937,
3.40420051794564));
#39968=CARTESIAN_POINT('Ctrl Pts',(12.2866370599935,0.386538816815474,3.49953544806202));
#39969=CARTESIAN_POINT('Ctrl Pts',(12.3343528960563,0.63000929582004,4.05445467686));
#39970=CARTESIAN_POINT('Ctrl Pts',(12.3820687321191,0.294932544534008,4.55936733800455));
#39971=CARTESIAN_POINT('Ctrl Pts',(12.429784568182,-0.310985300518122,4.55060436568669));
#39972=CARTESIAN_POINT('Ctrl Pts',(12.4775004042448,-0.631320558980542,
4.0362129322216));
#39973=CARTESIAN_POINT('Ctrl Pts',(12.5252162403077,-0.371904434015698,
3.48856660588983));
#39974=CARTESIAN_POINT('Ctrl Pts',(12.5729320763705,0.229037255191033,3.41057743478371));
#39975=CARTESIAN_POINT('Ctrl Pts',(12.6206479124333,0.619650508764677,3.87386407474765));
#39976=CARTESIAN_POINT('Ctrl Pts',(12.6683637484962,0.44122916559109,4.4529832757215));
#39977=CARTESIAN_POINT('Ctrl Pts',(12.716079584559,-0.142379709528176,4.61612096455669));
#39978=CARTESIAN_POINT('Ctrl Pts',(12.7637954206218,-0.595239106594286,
4.21346529139986));
#39979=CARTESIAN_POINT('Ctrl Pts',(12.8115112566847,-0.501481273143938,
3.61478115656484));
#39980=CARTESIAN_POINT('Ctrl Pts',(12.8592270927475,0.0527945297157079,
3.36984941301012));
#39981=CARTESIAN_POINT('Ctrl Pts',(12.9069429288104,0.558588303589165,3.70359464960132));
#39982=CARTESIAN_POINT('Ctrl Pts',(12.9546587648732,0.551421843290858,4.30953348024615));
#39983=CARTESIAN_POINT('Ctrl Pts',(13.002374600936,0.0378762195828894,4.63122295319618));
#39984=CARTESIAN_POINT('Ctrl Pts',(13.0500904369989,-0.510451719368595,
4.37325067561256));
#39985=CARTESIAN_POINT('Ctrl Pts',(13.0978062730617,-0.590023990114621,
3.77251655941407));
#39986=CARTESIAN_POINT('Ctrl Pts',(13.1455221091246,-0.127768152052348,
3.38068398698829));
#39987=CARTESIAN_POINT('Ctrl Pts',(13.1932379451874,0.451819146005312,3.55757883871291));
#39988=CARTESIAN_POINT('Ctrl Pts',(13.2409537812502,0.616493970155128,4.14075585037205));
#39989=CARTESIAN_POINT('Ctrl Pts',(13.2886696173131,0.215032895532453,4.59467459882739));
#39990=CARTESIAN_POINT('Ctrl Pts',(13.3363854533759,-0.383896195764066,
4.50249451293469));
#39991=CARTESIAN_POINT('Ctrl Pts',(13.3841012894387,-0.630287503488198,
3.94886598394213));
#39992=CARTESIAN_POINT('Ctrl Pts',(13.4318171255016,-0.297876098539286,
3.4421946086935));
#39993=CARTESIAN_POINT('Ctrl Pts',(13.4795329615644,0.308079511111167,3.44776450722078));
#39994=CARTESIAN_POINT('Ctrl Pts',(13.5272487976272,0.631120965295637,3.96046075600252));
#39995=CARTESIAN_POINT('Ctrl Pts',(13.5749646336901,0.374594326004835,4.50946650093658));
#39996=CARTESIAN_POINT('Ctrl Pts',(13.6226804697529,-0.225928046730791,
4.59062131891086));
#39997=CARTESIAN_POINT('Ctrl Pts',(13.6703963058158,-0.618977217803688,
4.12939949185215));
#39998=CARTESIAN_POINT('Ctrl Pts',(13.7181121418786,-0.443610085578744,
3.54934812035851));
#39999=CARTESIAN_POINT('Ctrl Pts',(13.7658279779415,0.139131014051702,3.38313730411011));
#40000=CARTESIAN_POINT('Ctrl Pts',(13.8135438140043,0.594105962672646,3.78340099315002));
#40001=CARTESIAN_POINT('Ctrl Pts',(13.8612596500671,0.503504264276035,4.38257088298437));
#40002=CARTESIAN_POINT('Ctrl Pts',(13.90897548613,-0.0494731474142026,4.63042004436449));
#40003=CARTESIAN_POINT('Ctrl Pts',(13.9566913221928,-0.557018606591754,
4.29934477874546));
#40004=CARTESIAN_POINT('Ctrl Pts',(14.0044071582556,-0.553045308503159,
3.69337659679301));
#40005=CARTESIAN_POINT('Ctrl Pts',(14.0521229943185,-0.0412019939202257,
3.36898540401303));
#40006=CARTESIAN_POINT('Ctrl Pts',(14.0998388303813,0.50847774565382,3.62406462413548));
#40007=CARTESIAN_POINT('Ctrl Pts',(14.1475546664442,0.591214547458171,4.22437108442359));
#40008=CARTESIAN_POINT('Ctrl Pts',(14.195270502507,0.131029933326566,4.61863412549262));
#40009=CARTESIAN_POINT('Ctrl Pts',(14.2429863385698,-0.4494814847335,4.44479593021223));
#40010=CARTESIAN_POINT('Ctrl Pts',(14.2907021746327,-0.617227139201166,
3.86249478815283));
#40011=CARTESIAN_POINT('Ctrl Pts',(14.3384180106955,-0.218163614480107,
3.40646679792233));
#40012=CARTESIAN_POINT('Ctrl Pts',(14.3861338467583,0.381242914296727,3.49548947984197));
#40013=CARTESIAN_POINT('Ctrl Pts',(14.4338496828212,0.630548208698617,4.0478119353149));
#40014=CARTESIAN_POINT('Ctrl Pts',(14.481565518884,0.300811380821271,4.55622795490698));
#40015=CARTESIAN_POINT('Ctrl Pts',(14.5292813549469,-0.305165166642291,
4.55385128484077));
#40016=CARTESIAN_POINT('Ctrl Pts',(14.5769971910097,-0.630903846008588,
4.04286445780787));
#40017=CARTESIAN_POINT('Ctrl Pts',(14.6247130270726,-0.37727381588172,3.49251453961553));
#40018=CARTESIAN_POINT('Ctrl Pts',(14.6724288631354,0.222812564473163,3.40819632836178));
#40019=CARTESIAN_POINT('Ctrl Pts',(14.7201446991982,0.618286738460357,3.86734053484336));
#40020=CARTESIAN_POINT('Ctrl Pts',(14.7678605352611,0.44597868695508,4.44830796940654));
#40021=CARTESIAN_POINT('Ctrl Pts',(14.8155763713239,-0.135878455045208,
4.6175872975589));
#40022=CARTESIAN_POINT('Ctrl Pts',(14.8632922073867,-0.592956321018707,
4.2197267075609));
#40023=CARTESIAN_POINT('Ctrl Pts',(14.9110080434496,-0.505513273594975,
3.62008770107973));
#40024=CARTESIAN_POINT('Ctrl Pts',(14.9587238795124,0.0461503912925444,
3.36932800439917));
#40025=CARTESIAN_POINT('Ctrl Pts',(15.0064397155752,0.555433441741075,3.69772410541485));
#40026=CARTESIAN_POINT('Ctrl Pts',(15.0541555516381,0.554653416196733,4.30370481154056));
#40027=CARTESIAN_POINT('Ctrl Pts',(15.1018713877009,0.0445266241191229,
4.63078871612938));
#40028=CARTESIAN_POINT('Ctrl Pts',(15.1495872237638,-0.506489652017253,
4.37860963676461));
#40029=CARTESIAN_POINT('Ctrl Pts',(15.1973030598266,-0.592388687361149,
3.77874750230084));
#40030=CARTESIAN_POINT('Ctrl Pts',(15.2450188958894,-0.134288076029725,
3.38206494088146));
#40031=CARTESIAN_POINT('Ctrl Pts',(15.2927347319523,0.447131341807447,3.5528416524037));
#40032=CARTESIAN_POINT('Ctrl Pts',(15.3404505680151,0.617943168462805,4.13425075493917));
#40033=CARTESIAN_POINT('Ctrl Pts',(15.3881664040779,0.221288275240951,4.59237532350063));
#40034=CARTESIAN_POINT('Ctrl Pts',(15.4358822401408,-0.378579046092452,
4.50651251762549));
#40035=CARTESIAN_POINT('Ctrl Pts',(15.4835980762036,-0.630791404211772,
3.95551147311801));
#40036=CARTESIAN_POINT('Ctrl Pts',(15.5313139122665,-0.303738309870084,
3.44536492739022));
#40037=CARTESIAN_POINT('Ctrl Pts',(15.5790297483293,0.302242348039936,3.44454830299756));
#40038=CARTESIAN_POINT('Ctrl Pts',(15.6267455843921,0.630669207148581,3.95381151868517));
#40039=CARTESIAN_POINT('Ctrl Pts',(15.674461420455,0.379942829239589,4.50549032746533));
#40040=CARTESIAN_POINT('Ctrl Pts',(15.7221772565178,-0.219690894932002,
4.59296959056563));
#40041=CARTESIAN_POINT('Ctrl Pts',(15.7698930925806,-0.617579089908608,
4.13591575463957));
#40042=CARTESIAN_POINT('Ctrl Pts',(15.8176089286435,-0.448334903946386,
3.5540483898953));
#40043=CARTESIAN_POINT('Ctrl Pts',(15.8653247647063,0.13262212282903,3.3817052505577));
#40044=CARTESIAN_POINT('Ctrl Pts',(15.9130406007692,0.591790213556878,3.77715169332057));
#40045=CARTESIAN_POINT('Ctrl Pts',(15.960756436832,0.507508245312566,4.37724316506909));
#40046=CARTESIAN_POINT('Ctrl Pts',(16.0084722728949,-0.0428263536203826,
4.63090643370248));
#40047=CARTESIAN_POINT('Ctrl Pts',(16.0561881089577,-0.553832853055588,
4.30519861652357));
#40048=CARTESIAN_POINT('Ctrl Pts',(16.1039039450205,-0.556246121716014,
3.69922221370673));
#40049=CARTESIAN_POINT('Ctrl Pts',(16.1516197810833,-0.0478500178579074,
3.36945468010413));
#40050=CARTESIAN_POINT('Ctrl Pts',(16.1993356171462,0.504487493666278,3.61872661594874));
#40051=CARTESIAN_POINT('Ctrl Pts',(16.247051453209,0.593546377218863,4.21812776701271));
#40052=CARTESIAN_POINT('Ctrl Pts',(16.2947672892719,0.137542489686435,4.61721883330181));
#40053=CARTESIAN_POINT('Ctrl Pts',(16.3424831253347,-0.444768782488292,
4.44950834783736));
#40054=CARTESIAN_POINT('Ctrl Pts',(16.3901989613976,-0.618642038056621,
3.86900742997889));
#40055=CARTESIAN_POINT('Ctrl Pts',(16.4379147974604,-0.224406791046256,
3.40879900475058));
#40056=CARTESIAN_POINT('Ctrl Pts',(16.4856306335233,0.375904665124208,3.49149955025639));
#40057=CARTESIAN_POINT('Ctrl Pts',(16.533346469586,0.631017083274371,4.04116388304691));
#40058=CARTESIAN_POINT('Ctrl Pts',(16.5810623056489,0.306656804407812,4.55302678864769));
#40059=CARTESIAN_POINT('Ctrl Pts',(16.6287781417117,-0.29931113646787,4.55703668482238));
#40060=CARTESIAN_POINT('Ctrl Pts',(16.6764939777746,-0.630417055231307,
4.04951122221356));
#40061=CARTESIAN_POINT('Ctrl Pts',(16.7242098138374,-0.382601291962586,
3.49651884241796));
#40062=CARTESIAN_POINT('Ctrl Pts',(16.7719256499003,0.216563124792967,3.40588095668335));
#40063=CARTESIAN_POINT('Ctrl Pts',(16.8196414859631,0.616854291799135,3.86083173012294));
#40064=CARTESIAN_POINT('Ctrl Pts',(16.8673573220259,0.450678671122871,4.44358286716973));
#40065=CARTESIAN_POINT('Ctrl Pts',(16.9150731580887,-0.129362107828251,
4.61898503189482));
#40066=CARTESIAN_POINT('Ctrl Pts',(16.9627889941516,-0.590607672668797,
4.22596371752193));
#40067=CARTESIAN_POINT('Ctrl Pts',(17.0105048302144,-0.509489124030439,
3.62543644444997));
#40068=CARTESIAN_POINT('Ctrl Pts',(17.0582206662773,0.0395011267029154,
3.3688766478407));
#40069=CARTESIAN_POINT('Ctrl Pts',(17.1059365023401,0.552216884982031,3.69188713660034));
#40070=CARTESIAN_POINT('Ctrl Pts',(17.153652338403,0.557823380833178,4.29784240874569));
#40071=CARTESIAN_POINT('Ctrl Pts',(17.2013681744658,0.0511720828492506,
4.63028441404532));
#40072=CARTESIAN_POINT('Ctrl Pts',(17.2490840105287,-0.502471326198846,
4.38392654375487));
#40073=CARTESIAN_POINT('Ctrl Pts',(17.2967998465914,-0.594687584883411,
3.78500302086511));
#40074=CARTESIAN_POINT('Ctrl Pts',(17.3445156826543,-0.140793083924855,
3.38351453206865));
#40075=CARTESIAN_POINT('Ctrl Pts',(17.3922315187171,0.442393872381948,3.5481541343218));
#40076=CARTESIAN_POINT('Ctrl Pts',(17.43994735478,0.61932372857571,4.1277307475695));
#40077=CARTESIAN_POINT('Ctrl Pts',(17.4876631908428,0.227519075297936,4.590010249934));
#40078=CARTESIAN_POINT('Ctrl Pts',(17.5353790269057,-0.373219845656906,
4.51047426130944));
#40079=CARTESIAN_POINT('Ctrl Pts',(17.5830948629685,-0.631225239619516,
3.96216190386831));
#40080=CARTESIAN_POINT('Ctrl Pts',(17.6308106990313,-0.309566783390781,
3.44859685231885));
#40081=CARTESIAN_POINT('Ctrl Pts',(17.6785265350942,0.29637161332294,3.44139379571298));
#40082=CARTESIAN_POINT('Ctrl Pts',(17.726242371157,0.630147397258769,3.94716741176515));
#40083=CARTESIAN_POINT('Ctrl Pts',(17.7739582072198,0.385249130227842,4.50145800652724));
#40084=CARTESIAN_POINT('Ctrl Pts',(17.8216740432827,-0.213429340911116,
4.59525199797214));
#40085=CARTESIAN_POINT('Ctrl Pts',(17.8693898793456,-0.616112364258878,
4.14241692054995));
#40086=CARTESIAN_POINT('Ctrl Pts',(17.9171057154084,-0.453009923400427,
3.55879819362073));
#40087=CARTESIAN_POINT('Ctrl Pts',(17.9648215514712,0.126098500570276,3.38034187425201));
#40088=CARTESIAN_POINT('Ctrl Pts',(18.012537387534,0.589408731192455,3.77092714642348));
#40089=CARTESIAN_POINT('Ctrl Pts',(18.0602532235969,0.511455854741549,4.3718735447732));
#40090=CARTESIAN_POINT('Ctrl Pts',(18.1079690596597,-0.0361748028784226,
4.6313227449477));
#40091=CARTESIAN_POINT('Ctrl Pts',(18.1556848957226,-0.55058558239424,4.31101855428765));
#40092=CARTESIAN_POINT('Ctrl Pts',(18.2034007317854,-0.559385149749292,
3.70510123958967));
#40093=CARTESIAN_POINT('Ctrl Pts',(18.2511165678482,-0.0544927268426965,
3.36999399417717));
#40094=CARTESIAN_POINT('Ctrl Pts',(18.2988324039111,0.500441205601937,3.6134309578002));
#40095=CARTESIAN_POINT('Ctrl Pts',(18.3465482399739,0.595812278664582,4.21186022100458));
#40096=CARTESIAN_POINT('Ctrl Pts',(18.3942640760367,0.144039768479226,4.61573498337195));
#40097=CARTESIAN_POINT('Ctrl Pts',(18.4419799120996,-0.440006677437314,
4.4541708362083));
#40098=CARTESIAN_POINT('Ctrl Pts',(18.4896957481624,-0.619988221090196,
3.87553462183804));
#40099=CARTESIAN_POINT('Ctrl Pts',(18.5374115842252,-0.230625041570952,
3.41119687937986));
#40100=CARTESIAN_POINT('Ctrl Pts',(18.5851274202881,0.370524662245315,3.48756610248778));
#40101=CARTESIAN_POINT('Ctrl Pts',(18.6328432563509,0.631415867466904,4.03451125849008));
#40102=CARTESIAN_POINT('Ctrl Pts',(18.6805590924138,0.31246816601179,4.54976419479712));
#40103=CARTESIAN_POINT('Ctrl Pts',(18.7282749284766,-0.293423860232864,
4.56016021181225));
#40104=CARTESIAN_POINT('Ctrl Pts',(18.7759907645394,-0.629860240718928,
4.05615248714788));
#40105=CARTESIAN_POINT('Ctrl Pts',(18.8237066006023,-0.387886270507855,
3.50057906951772));
#40106=CARTESIAN_POINT('Ctrl Pts',(18.8714224366651,0.210289630309142,3.40363157692976));
#40107=CARTESIAN_POINT('Ctrl Pts',(18.919138272728,0.615353327889266,3.85433838355196));
#40108=CARTESIAN_POINT('Ctrl Pts',(18.9668541087908,0.455328596044662,4.43880849385601));
#40109=CARTESIAN_POINT('Ctrl Pts',(19.0145699448537,-0.122831391686292,
4.62031401230505));
#40110=CARTESIAN_POINT('Ctrl Pts',(19.0622857809165,-0.588193422413584,
4.2321756285162));
#40111=CARTESIAN_POINT('Ctrl Pts',(19.1100016169793,-0.513408382846255,
3.63082679254236));
#40112=CARTESIAN_POINT('Ctrl Pts',(19.1577174530421,0.0328474745430158,
3.36849539350727));
#40113=CARTESIAN_POINT('Ctrl Pts',(19.205433289105,0.548938990540088,3.68608439142882));
#40114=CARTESIAN_POINT('Ctrl Pts',(19.2531491251678,0.560931385193363,4.2919469231649));
#40115=CARTESIAN_POINT('Ctrl Pts',(19.3008649612307,0.0578118574426247,
4.62971010270368));
#40116=CARTESIAN_POINT('Ctrl Pts',(19.3485807972935,-0.498397187901359,
4.38920080648958));
#40117=CARTESIAN_POINT('Ctrl Pts',(19.3962966333563,-0.596920427988996,
3.79128241936144));
#40118=CARTESIAN_POINT('Ctrl Pts',(19.4440124694192,-0.147282451949449,
3.38503260125846));
#40119=CARTESIAN_POINT('Ctrl Pts',(19.491728305482,0.437607261597584,3.54351680188243));
#40120=CARTESIAN_POINT('Ctrl Pts',(19.5394441415449,0.620635501579114,4.12119655861503));
#40121=CARTESIAN_POINT('Ctrl Pts',(19.5871599776077,0.233724595248439,4.58757962923414));
#40122=CARTESIAN_POINT('Ctrl Pts',(19.6348758136705,-0.367819173932889,
4.51437932582758));
#40123=CARTESIAN_POINT('Ctrl Pts',(19.6825916497334,-0.631588991354928,
3.96881649615688));
#40124=CARTESIAN_POINT('Ctrl Pts',(19.7303074857962,-0.315360815373557,
3.4518901025469));
#40125=CARTESIAN_POINT('Ctrl Pts',(19.778023321859,0.290467852693633,3.43830118837221));
#40126=CARTESIAN_POINT('Ctrl Pts',(19.8257391579219,0.629555794415491,3.94052945152661));
#40127=CARTESIAN_POINT('Ctrl Pts',(19.8734549939847,0.390512260364629,4.49736946054851));
#40128=CARTESIAN_POINT('Ctrl Pts',(19.9211708300476,-0.207143364153331,
4.59746927979605));
#40129=CARTESIAN_POINT('Ctrl Pts',(19.9688866661104,-0.61457855576007,4.14890039401813));
#40130=CARTESIAN_POINT('Ctrl Pts',(20.0166025021732,-0.45763207183192,3.5636005413983));
#40131=CARTESIAN_POINT('Ctrl Pts',(20.0643183382361,0.119556051622903,3.37904064719698));
#40132=CARTESIAN_POINT('Ctrl Pts',(20.1120341742989,0.586970881772813,3.7647406560623));
#40133=CARTESIAN_POINT('Ctrl Pts',(20.1597500103618,0.515329468049299,4.36643880344312));
#40134=CARTESIAN_POINT('Ctrl Pts',(20.2074658464246,-0.029486781418557,
4.63171390504007));
#40135=CARTESIAN_POINT('Ctrl Pts',(20.2551816824874,-0.547338447674763,
4.31671898245684));
#40136=CARTESIAN_POINT('Ctrl Pts',(20.3028975185503,-0.562346186529673,
3.71117381387971));
#40137=CARTESIAN_POINT('Ctrl Pts',(20.3506133546131,-0.0613491664957494,
3.37029669484294));
#40138=CARTESIAN_POINT('Ctrl Pts',(20.398329190676,0.496762641213801,3.60878154740643));
#40139=CARTESIAN_POINT('Ctrl Pts',(20.4380923873949,0.580417208789547,4.10498761157686));
#40140=CARTESIAN_POINT('Ctrl Pts',(20.4699029447702,0.374745574175769,4.41137453781958));
#40141=CARTESIAN_POINT('Ctrl Pts',(20.4937608628016,0.13332385162888,4.54159545884303));
#40142=CARTESIAN_POINT('Ctrl Pts',(20.517618780833,-0.143293564288956,4.53872805560682));
#40143=CARTESIAN_POINT('Ctrl Pts',(20.5414766988645,-0.38346854803195,4.40448715909776));
#40144=CARTESIAN_POINT('Ctrl Pts',(20.5653346168959,-0.530621786340447,
4.17114564603877));
#40145=CARTESIAN_POINT('Ctrl Pts',(20.5891925349273,-0.547627617499454,
3.89605651468078));
#40146=CARTESIAN_POINT('Ctrl Pts',(20.6130504529587,-0.430933317123153,
3.64633026976583));
#40147=CARTESIAN_POINT('Ctrl Pts',(20.6369083709901,-0.208752997660079,
3.48311457674551));
#40148=CARTESIAN_POINT('Ctrl Pts',(20.6607662890215,0.0644142843662171,
3.4462762657402));
#40149=CARTESIAN_POINT('Ctrl Pts',(20.684624207053,0.321861676845817,3.54484653226013));
#40150=CARTESIAN_POINT('Ctrl Pts',(20.7084821250844,0.500588620804837,3.75470996102831));
#40151=CARTESIAN_POINT('Ctrl Pts',(20.7323400431158,0.556916750317041,4.02455574134091));
#40152=CARTESIAN_POINT('Ctrl Pts',(20.7561979611472,0.47705893600668,4.28839577951569));
#40153=CARTESIAN_POINT('Ctrl Pts',(20.7800558791787,0.280549668164313,4.48171582646486));
#40154=CARTESIAN_POINT('Ctrl Pts',(20.8039137972101,0.0154370662995263,
4.55724289713534));
#40155=CARTESIAN_POINT('Ctrl Pts',(20.8277717152415,-0.253449631274377,
4.49650907789895));
#40156=CARTESIAN_POINT('Ctrl Pts',(20.8516296332729,-0.460361354274216,
4.31436517051053));
#40157=CARTESIAN_POINT('Ctrl Pts',(20.8754875513043,-0.554701993332711,
4.05535046556385));
#40158=CARTESIAN_POINT('Ctrl Pts',(20.8993454693358,-0.513402987365846,
3.78280103771366));
#40159=CARTESIAN_POINT('Ctrl Pts',(20.9232033873672,-0.346562912086465,
3.56336268648205));
#40160=CARTESIAN_POINT('Ctrl Pts',(20.9470613053986,-0.0949787932613798,
3.45069404477467));
#40161=CARTESIAN_POINT('Ctrl Pts',(20.97091922343,0.179830242856268,3.47234567582879));
#40162=CARTESIAN_POINT('Ctrl Pts',(20.9947771414614,0.410665878084123,3.62302316008453));
#40163=CARTESIAN_POINT('Ctrl Pts',(21.0186350594928,0.541082524061315,3.86588175144064));
#40164=CARTESIAN_POINT('Ctrl Pts',(21.0424929775243,0.539189751860116,4.14153590729571));
#40165=CARTESIAN_POINT('Ctrl Pts',(21.0663508955557,0.405450399288564,4.38258067876424));
#40166=CARTESIAN_POINT('Ctrl Pts',(21.0902088135871,0.172567379211795,4.53007405282339));
#40167=CARTESIAN_POINT('Ctrl Pts',(21.1140667316185,-0.102513065388571,
4.54794988212627));
#40168=CARTESIAN_POINT('Ctrl Pts',(21.1379246496499,-0.352526273278862,
4.43183703934844));
#40169=CARTESIAN_POINT('Ctrl Pts',(21.1617825676814,-0.516337204635697,
4.21012827746935));
#40170=CARTESIAN_POINT('Ctrl Pts',(21.1856404857128,-0.553889624765765,
3.93703742795684));
#40171=CARTESIAN_POINT('Ctrl Pts',(21.2094984037442,-0.456000943963824,
3.67934264238169));
#40172=CARTESIAN_POINT('Ctrl Pts',(21.2333563217756,-0.246607611160355,
3.50005731527167));
#40173=CARTESIAN_POINT('Ctrl Pts',(21.257214239807,0.0230880000356606,3.44302159274494));
#40174=CARTESIAN_POINT('Ctrl Pts',(21.2810721578385,0.287137966314551,3.52218226257825));
#40175=CARTESIAN_POINT('Ctrl Pts',(21.3049300758698,0.480974878350452,3.71818238470557));
#40176=CARTESIAN_POINT('Ctrl Pts',(21.3287879939013,0.557200331135927,3.9830945903298));
#40177=CARTESIAN_POINT('Ctrl Pts',(21.3526459119327,0.497175125126959,4.25214062911267));
#40178=CARTESIAN_POINT('Ctrl Pts',(21.3765038299641,0.31557705824565,4.45953141590455));
#40179=CARTESIAN_POINT('Ctrl Pts',(21.4003617479955,0.0568118044769688,
4.55455425412338));
#40180=CARTESIAN_POINT('Ctrl Pts',(21.424219666027,-0.215845483008899,4.51397347145443));
#40181=CARTESIAN_POINT('Ctrl Pts',(21.4480775840584,-0.435722670386138,
4.34771217465862));
#40182=CARTESIAN_POINT('Ctrl Pts',(21.4719355020898,-0.549053796006754,
4.0964257796693));
#40183=CARTESIAN_POINT('Ctrl Pts',(21.4957934201212,-0.528126312578589,
3.82156065496534));
#40184=CARTESIAN_POINT('Ctrl Pts',(21.5196513381527,-0.378057559853047,
3.59032881071252));
#40185=CARTESIAN_POINT('Ctrl Pts',(21.543509256184,-0.135543435662257,3.45927273145963));
#40186=CARTESIAN_POINT('Ctrl Pts',(21.5673671742155,0.14011475067701,3.46043919847993));
#40187=CARTESIAN_POINT('Ctrl Pts',(21.5912250922469,0.381511063826562,3.59354297881304));
#40188=CARTESIAN_POINT('Ctrl Pts',(21.6150830102783,0.529617529717794,3.8260365724933));
#40189=CARTESIAN_POINT('Ctrl Pts',(21.6389409283097,0.548218083101175,4.10106896286759));
#40190=CARTESIAN_POINT('Ctrl Pts',(21.6627988463412,0.432764382005563,4.35138723875747));
#40191=CARTESIAN_POINT('Ctrl Pts',(21.6866567643726,0.211488001244504,4.51578176317496));
#40192=CARTESIAN_POINT('Ctrl Pts',(21.710514682404,-0.0615029566383307,
4.55405359688301));
#40193=CARTESIAN_POINT('Ctrl Pts',(21.7343726004354,-0.319454766316188,
4.4568442340362));
#40194=CARTESIAN_POINT('Ctrl Pts',(21.7582305184669,-0.499291183856609,
4.24792401178047));
#40195=CARTESIAN_POINT('Ctrl Pts',(21.7820884364982,-0.557037306525311,
3.97837961532992));
#40196=CARTESIAN_POINT('Ctrl Pts',(21.8059463545297,-0.478572634356998,
3.71412199185867));
#40197=CARTESIAN_POINT('Ctrl Pts',(21.8298042725611,-0.283083917031579,
3.51976932853855));
#40198=CARTESIAN_POINT('Ctrl Pts',(21.8536621905926,-0.018373470940863,
3.44284614561161));
#40199=CARTESIAN_POINT('Ctrl Pts',(21.8775201086239,0.250829789278194,3.5021622566489));
#40200=CARTESIAN_POINT('Ctrl Pts',(21.9013780266554,0.458698333552465,3.68321325676341));
#40201=CARTESIAN_POINT('Ctrl Pts',(21.9252359446868,0.55440264058141,3.94172724469688));
#40202=CARTESIAN_POINT('Ctrl Pts',(21.9490938627182,0.514540400363477,4.21449050861997));
#40203=CARTESIAN_POINT('Ctrl Pts',(21.9729517807496,0.348859016457567,4.4348050005813));
#40204=CARTESIAN_POINT('Ctrl Pts',(21.996809698781,0.0978721002989983,4.54879782605011));
#40205=CARTESIAN_POINT('Ctrl Pts',(22.0206676168125,-0.177047210365213,
4.52859463409701));
#40206=CARTESIAN_POINT('Ctrl Pts',(22.0445255348439,-0.408673655425848,
4.3791356554785));
#40207=CARTESIAN_POINT('Ctrl Pts',(22.0683834528753,-0.540368259688198,
4.13696768164748));
#40208=CARTESIAN_POINT('Ctrl Pts',(22.0922413709067,-0.53992810512055,3.86130737872913));
#40209=CARTESIAN_POINT('Ctrl Pts',(22.1160992889381,-0.407460821505317,
3.61956119962225));
#40210=CARTESIAN_POINT('Ctrl Pts',(22.1399572069695,-0.175358268020808,
3.47084267015335));
#40211=CARTESIAN_POINT('Ctrl Pts',(22.163815125001,0.0996241586556461,3.45151752178681));
#40212=CARTESIAN_POINT('Ctrl Pts',(22.1876730430324,0.350245764837839,3.56631127970877));
#40213=CARTESIAN_POINT('Ctrl Pts',(22.2115309610638,0.51522274100534,3.78715374318048));
#40214=CARTESIAN_POINT('Ctrl Pts',(22.2353888790952,0.554213722627899,4.06004291426965));
#40215=CARTESIAN_POINT('Ctrl Pts',(22.2592467971266,0.457684352558003,4.31824995726588));
#40216=CARTESIAN_POINT('Ctrl Pts',(22.2831047151581,0.249238691275201,4.49863621678958));
#40217=CARTESIAN_POINT('Ctrl Pts',(22.3069626331895,-0.0201526192614011,
4.55709233866662));
#40218=CARTESIAN_POINT('Ctrl Pts',(22.3308205512209,-0.284616065231974,
4.47932420896945));
#40219=CARTESIAN_POINT('Ctrl Pts',(22.3546784692523,-0.479483130864429,
4.28434825342259));
#40220=CARTESIAN_POINT('Ctrl Pts',(22.3785363872838,-0.557103509392546,
4.01984140485232));
#40221=CARTESIAN_POINT('Ctrl Pts',(22.4023943053151,-0.498496906094933,
3.75048279151596));
#40222=CARTESIAN_POINT('Ctrl Pts',(22.4262522233466,-0.317994227800984,
3.542137933897));
#40223=CARTESIAN_POINT('Ctrl Pts',(22.450110141378,-0.0597333038680864,
3.44575282046209));
#40224=CARTESIAN_POINT('Ctrl Pts',(22.4739680594094,0.213134049493302,3.48489624527193));
#40225=CARTESIAN_POINT('Ctrl Pts',(22.4978259774408,0.433884304103661,3.6499965589521));
#40226=CARTESIAN_POINT('Ctrl Pts',(22.5216838954723,0.548538061567711,3.90068226732924));
#40227=CARTESIAN_POINT('Ctrl Pts',(22.5455418135037,0.529059256943919,4.17565382996358));
#40228=CARTESIAN_POINT('Ctrl Pts',(22.5693997315351,0.380211173855379,4.40767331583304));
#40229=CARTESIAN_POINT('Ctrl Pts',(22.5932576495665,0.138390873272415,4.54000544018811));
#40230=CARTESIAN_POINT('Ctrl Pts',(22.6171155675979,-0.137269333605106,
4.54029177230974));
#40231=CARTESIAN_POINT('Ctrl Pts',(22.6409734856293,-0.379364264814148,
4.40846158181013));
#40232=CARTESIAN_POINT('Ctrl Pts',(22.6648314036608,-0.528692759685234,
4.17675229015827));
#40233=CARTESIAN_POINT('Ctrl Pts',(22.6886893216921,-0.54874438127821,3.90182058373076));
#40234=CARTESIAN_POINT('Ctrl Pts',(22.7125472397236,-0.434607562942265,
3.65089956353622));
#40235=CARTESIAN_POINT('Ctrl Pts',(22.736405157755,-0.214207731687487,3.48533716867003));
#40236=CARTESIAN_POINT('Ctrl Pts',(22.7602630757864,0.0585913648593265,
3.44563509732658));
#40237=CARTESIAN_POINT('Ctrl Pts',(22.7841209938179,0.31702578011682,3.5414689143437));
#40238=CARTESIAN_POINT('Ctrl Pts',(22.8079789118493,0.498012898707086,3.74946820019106));
#40239=CARTESIAN_POINT('Ctrl Pts',(22.8238841905369,0.537376264140017,3.92891364167179));
#40240=CARTESIAN_POINT('Ctrl Pts',(22.8318368298807,0.534391234777113,4.01792167950194));
#40241=CARTESIAN_POINT('Ctrl Pts',(3.99999999999998,0.254694598474614,4.53673594206822));
#40242=CARTESIAN_POINT('Ctrl Pts',(4.00795263934379,0.165296026927429,4.57915779516171));
#40243=CARTESIAN_POINT('Ctrl Pts',(4.0238579180314,-0.0350146299391769,
4.61842892627033));
#40244=CARTESIAN_POINT('Ctrl Pts',(4.04771583606282,-0.327086058023631,
4.5259865276721));
#40245=CARTESIAN_POINT('Ctrl Pts',(4.07157375409423,-0.539100294705402,
4.30498302442502));
#40246=CARTESIAN_POINT('Ctrl Pts',(4.09543167212566,-0.619328256935644,
4.00937412827253));
#40247=CARTESIAN_POINT('Ctrl Pts',(4.11928959015708,-0.548093442686671,
3.71148804617917));
#40248=CARTESIAN_POINT('Ctrl Pts',(4.1431475081885,-0.342845496867427,3.48414304986991));
#40249=CARTESIAN_POINT('Ctrl Pts',(4.16700542621991,-0.0537568536316998,
3.38294333505492));
#40250=CARTESIAN_POINT('Ctrl Pts',(4.19086334425134,0.248473820944083,3.43262855616194));
#40251=CARTESIAN_POINT('Ctrl Pts',(4.21472126228276,0.489947458130694,3.62105272953394));
#40252=CARTESIAN_POINT('Ctrl Pts',(4.23857918031417,0.611614759069978,3.90213920826301));
#40253=CARTESIAN_POINT('Ctrl Pts',(4.26243709834559,0.583726034554802,4.20715564703007));
#40254=CARTESIAN_POINT('Ctrl Pts',(4.28629501637702,0.413100159498109,4.46151671210738));
#40255=CARTESIAN_POINT('Ctrl Pts',(4.31015293440843,0.141460167127662,4.60302446238992));
#40256=CARTESIAN_POINT('Ctrl Pts',(4.33401085243986,-0.164770755236008,
4.59707625642582));
#40257=CARTESIAN_POINT('Ctrl Pts',(4.35786877047126,-0.430710704813839,
4.44512666775742));
#40258=CARTESIAN_POINT('Ctrl Pts',(4.38172668850269,-0.59133017320549,4.18433147003372));
#40259=CARTESIAN_POINT('Ctrl Pts',(4.40558460653411,-0.607353296958831,
3.87846221409715));
#40260=CARTESIAN_POINT('Ctrl Pts',(4.42944252456553,-0.474862000813124,
3.60231225357117));
#40261=CARTESIAN_POINT('Ctrl Pts',(4.45330044259694,-0.226254007744579,
3.42340778189093));
#40262=CARTESIAN_POINT('Ctrl Pts',(4.47715836062837,0.0776792518003291,
3.38549581251083));
#40263=CARTESIAN_POINT('Ctrl Pts',(4.50101627865978,0.362617819109035,3.49784685630402));
#40264=CARTESIAN_POINT('Ctrl Pts',(4.5248741966912,0.558886451727075,3.73298802180378));
#40265=CARTESIAN_POINT('Ctrl Pts',(4.54873211472262,0.618492123352341,4.03342088939383));
#40266=CARTESIAN_POINT('Ctrl Pts',(4.57259003275404,0.5268596233165,4.32568143907503));
#40267=CARTESIAN_POINT('Ctrl Pts',(4.59644795078546,0.306395594072305,4.5383040055633));
#40268=CARTESIAN_POINT('Ctrl Pts',(4.62030586881688,0.0110094959969652,
4.61929657956068));
#40269=CARTESIAN_POINT('Ctrl Pts',(4.6441637868483,-0.287068723725306,4.54885427056805));
#40270=CARTESIAN_POINT('Ctrl Pts',(4.66802170487971,-0.514950820910697,
4.34420214192463));
#40271=CARTESIAN_POINT('Ctrl Pts',(4.69187962291114,-0.616913415399932,
4.05538321370614));
#40272=CARTESIAN_POINT('Ctrl Pts',(4.71573754094255,-0.568023875442366,
3.75302158112612));
#40273=CARTESIAN_POINT('Ctrl Pts',(4.73959545897398,-0.380237025278099,
3.51105289951885));
#40274=CARTESIAN_POINT('Ctrl Pts',(4.76345337700539,-0.0994718649854296,
3.38864510263028));
#40275=CARTESIAN_POINT('Ctrl Pts',(4.78731129503681,0.205616875855751,3.41573023112194));
#40276=CARTESIAN_POINT('Ctrl Pts',(4.81116921306823,0.460426689658758,3.5856852332931));
#40277=CARTESIAN_POINT('Ctrl Pts',(4.83502713109965,0.60264963606909,3.85695148163183));
#40278=CARTESIAN_POINT('Ctrl Pts',(4.85888504913107,0.597508330613982,4.16319698927494));
#40279=CARTESIAN_POINT('Ctrl Pts',(4.88274296716248,0.446259962523644,4.42953638764361));
#40280=CARTESIAN_POINT('Ctrl Pts',(4.90660088519391,0.185888877718945,4.59084243889714));
#40281=CARTESIAN_POINT('Ctrl Pts',(4.93045880322533,-0.119937101199393,
4.60767141961541));
#40282=CARTESIAN_POINT('Ctrl Pts',(4.95431672125674,-0.396435191853442,
4.47590818560059));
#40283=CARTESIAN_POINT('Ctrl Pts',(4.97817463928816,-0.575994079421511,
4.22777243672773));
#40284=CARTESIAN_POINT('Ctrl Pts',(5.00203255731958,-0.614706724807315,
3.92394012267834));
#40285=CARTESIAN_POINT('Ctrl Pts',(5.025890475351,-0.503106831702736,3.63870652046354));
#40286=CARTESIAN_POINT('Ctrl Pts',(5.04974839338242,-0.268483613891896,
3.44181901543221));
#40287=CARTESIAN_POINT('Ctrl Pts',(5.07360631141384,0.0317911608623165,
3.38142196567243));
#40288=CARTESIAN_POINT('Ctrl Pts',(5.09746422944526,0.32429213081186,3.47228409503311));
#40289=CARTESIAN_POINT('Ctrl Pts',(5.12132214747667,0.537494841237617,3.69218713785082));
#40290=CARTESIAN_POINT('Ctrl Pts',(5.1451800655081,0.619265421915264,3.98735881011802));
#40291=CARTESIAN_POINT('Ctrl Pts',(5.16903798353952,0.549608738483219,4.28562159765047));
#40292=CARTESIAN_POINT('Ctrl Pts',(5.19289590157094,0.34555774745058,4.51404212438126));
#40293=CARTESIAN_POINT('Ctrl Pts',(5.21675381960235,0.0570084743622218,
4.61676534947452));
#40294=CARTESIAN_POINT('Ctrl Pts',(5.24061173763377,-0.245480923587363,
4.56867264627043));
#40295=CARTESIAN_POINT('Ctrl Pts',(5.26446965566519,-0.487943548953736,
4.38152399072137));
#40296=CARTESIAN_POINT('Ctrl Pts',(5.28832757369661,-0.611090685285508,
4.10108232693608));
#40297=CARTESIAN_POINT('Ctrl Pts',(5.31218549172803,-0.584809503288917,
3.79592328078761));
#40298=CARTESIAN_POINT('Ctrl Pts',(5.33604340975945,-0.415526467847156,
3.5406665514248));
#40299=CARTESIAN_POINT('Ctrl Pts',(5.35990132779088,-0.144635892303038,
3.39772936223054));
#40300=CARTESIAN_POINT('Ctrl Pts',(5.38375924582228,0.161622098711782,3.40206374949372));
#40301=CARTESIAN_POINT('Ctrl Pts',(5.40761716385371,0.428359084093981,3.55260983746209));
#40302=CARTESIAN_POINT('Ctrl Pts',(5.43147508188512,0.590350605148055,3.81255500683439));
#40303=CARTESIAN_POINT('Ctrl Pts',(5.45533299991655,0.607985322415754,4.11833558293467));
#40304=CARTESIAN_POINT('Ctrl Pts',(5.47919091794796,0.476951067165249,4.39517988561105));
#40305=CARTESIAN_POINT('Ctrl Pts',(5.50304883597938,0.2292892841064,4.57539194177126));
#40306=CARTESIAN_POINT('Ctrl Pts',(5.5269067540108,-0.0744399746307492,
4.61490499480714));
#40307=CARTESIAN_POINT('Ctrl Pts',(5.55076467204222,-0.359966631867259,
4.5040570269359));
#40308=CARTESIAN_POINT('Ctrl Pts',(5.57462259007364,-0.55747164231658,4.26995338574299));
#40309=CARTESIAN_POINT('Ctrl Pts',(5.59848050810506,-0.618659650999605,
3.96983878834977));
#40310=CARTESIAN_POINT('Ctrl Pts',(5.62233842613648,-0.528568523057477,
3.67709942878664));
#40311=CARTESIAN_POINT('Ctrl Pts',(5.6461963441679,-0.309227993320144,3.46331805450751));
#40312=CARTESIAN_POINT('Ctrl Pts',(5.67005426219932,-0.0142727959960426,
3.38077003484781));
#40313=CARTESIAN_POINT('Ctrl Pts',(5.69391218023074,0.284172488697173,3.4496406091084));
#40314=CARTESIAN_POINT('Ctrl Pts',(5.71777009826216,0.513129859266986,3.65308904601577));
#40315=CARTESIAN_POINT('Ctrl Pts',(5.74162801629357,0.616613001744231,3.94136666067651));
#40316=CARTESIAN_POINT('Ctrl Pts',(5.765485934325,0.569317469330215,4.24398172424487));
#40317=CARTESIAN_POINT('Ctrl Pts',(5.78934385235641,0.382808307322586,4.48693660973462));
#40318=CARTESIAN_POINT('Ctrl Pts',(5.81320177038783,0.102692087527565,4.61082223133738));
#40319=CARTESIAN_POINT('Ctrl Pts',(5.83705968841925,-0.202535146533943,
4.58534517687525));
#40320=CARTESIAN_POINT('Ctrl Pts',(5.86091760645067,-0.458237017319611,
4.41673528603543));
#40321=CARTESIAN_POINT('Ctrl Pts',(5.88477552448209,-0.601887460912657,
4.14622225884759));
#40322=CARTESIAN_POINT('Ctrl Pts',(5.9086334425135,-0.598360014525416,3.83995392008642));
#40323=CARTESIAN_POINT('Ctrl Pts',(5.93249136054493,-0.448517265794504,
3.57282118150817));
#40324=CARTESIAN_POINT('Ctrl Pts',(5.95634927857635,-0.188999790056246,
3.41014534911766));
#40325=CARTESIAN_POINT('Ctrl Pts',(5.98020719660777,0.116733210556207,3.39170495376011));
#40326=CARTESIAN_POINT('Ctrl Pts',(6.00406511463918,0.393921897475357,3.52200944135141));
#40327=CARTESIAN_POINT('Ctrl Pts',(6.02792303267061,0.574785693380153,3.76919531120668));
#40328=CARTESIAN_POINT('Ctrl Pts',(6.05178095070201,0.61509921541814,4.07281983667942));
#40329=CARTESIAN_POINT('Ctrl Pts',(6.07563886873346,0.505003308517799,4.35863675364492));
#40330=CARTESIAN_POINT('Ctrl Pts',(6.09949678676485,0.27142206589204,4.55675943366228));
#40331=CARTESIAN_POINT('Ctrl Pts',(6.12335470479629,-0.0285325303540597,
4.61873507756083));
#40332=CARTESIAN_POINT('Ctrl Pts',(6.14721262282769,-0.321503980505702,
4.52942105023226));
#40333=CARTESIAN_POINT('Ctrl Pts',(6.17107054085913,-0.535870591003297,
4.31063422072759));
#40334=CARTESIAN_POINT('Ctrl Pts',(6.19492845889052,-0.619180264299368,
4.01591706164003));
#40335=CARTESIAN_POINT('Ctrl Pts',(6.21878637692196,-0.551125001039776,
3.71725450231754));
#40336=CARTESIAN_POINT('Ctrl Pts',(6.24264429495337,-0.348226295733882,
3.48783145534908));
#40337=CARTESIAN_POINT('Ctrl Pts',(6.2665022129848,-0.0603247367796791,
3.38345774569467));
#40338=CARTESIAN_POINT('Ctrl Pts',(6.29036013101621,0.242607149567705,3.43020375417728));
#40339=CARTESIAN_POINT('Ctrl Pts',(6.31421804904763,0.485688404846908,3.61560451082823));
#40340=CARTESIAN_POINT('Ctrl Pts',(6.33807596707905,0.61099356578022,3.89627130770405));
#40341=CARTESIAN_POINT('Ctrl Pts',(6.36193388511046,0.585080291527744,4.19994745529594));
#40342=CARTESIAN_POINT('Ctrl Pts',(6.3937444424857,0.363797450650833,4.54512657044717));
#40343=CARTESIAN_POINT('Ctrl Pts',(6.43350763920472,-0.178959141669374,
4.67939801199369));
#40344=CARTESIAN_POINT('Ctrl Pts',(6.48122347526757,-0.668951848353412,
4.21606826543601));
#40345=CARTESIAN_POINT('Ctrl Pts',(6.5289393113304,-0.543175254381078,3.55462676401443));
#40346=CARTESIAN_POINT('Ctrl Pts',(6.57665514739324,0.0806513803028556,
3.30201433154981));
#40347=CARTESIAN_POINT('Ctrl Pts',(6.62437098345608,0.630812951656228,3.69045991683978));
#40348=CARTESIAN_POINT('Ctrl Pts',(6.67208681951892,0.601478580142798,4.36311480674272));
#40349=CARTESIAN_POINT('Ctrl Pts',(6.71980265558175,0.0199087309838695,
4.70234020845997));
#40350=CARTESIAN_POINT('Ctrl Pts',(6.76751849164459,-0.580002689552455,
4.39658285339385));
#40351=CARTESIAN_POINT('Ctrl Pts',(6.81523432770743,-0.64725742864426,3.72664421308375));
#40352=CARTESIAN_POINT('Ctrl Pts',(6.86295016377027,-0.120142281411799,
3.30772876957018));
#40353=CARTESIAN_POINT('Ctrl Pts',(6.91066599983311,0.517310146858294,3.52453857056345));
#40354=CARTESIAN_POINT('Ctrl Pts',(6.95838183589594,0.679704059947864,4.17797090041396));
#40355=CARTESIAN_POINT('Ctrl Pts',(7.00609767195879,0.217917737520193,4.66797035296266));
#40356=CARTESIAN_POINT('Ctrl Pts',(7.05381350802161,-0.443987099894697,
4.54456206689342));
#40357=CARTESIAN_POINT('Ctrl Pts',(7.10152934408447,-0.698171061503544,
3.92107420680554));
#40358=CARTESIAN_POINT('Ctrl Pts',(7.14924518014729,-0.311214160204793,
3.3700650369752));
#40359=CARTESIAN_POINT('Ctrl Pts',(7.19696101621015,0.361535686685884,3.39753487888718));
#40360=CARTESIAN_POINT('Ctrl Pts',(7.24467685227297,0.702281647003851,3.97825768917858));
#40361=CARTESIAN_POINT('Ctrl Pts',(7.29239268833582,0.398111619195611,4.5789468099385));
#40362=CARTESIAN_POINT('Ctrl Pts',(7.34010852439865,-0.271650463017158,
4.64798016059173));
#40363=CARTESIAN_POINT('Ctrl Pts',(7.38782436046149,-0.691951729928866,
4.1219633626529));
#40364=CARTESIAN_POINT('Ctrl Pts',(7.43554019652432,-0.476823084268312,
3.48394573037578));
#40365=CARTESIAN_POINT('Ctrl Pts',(7.48325603258717,0.17617954081454,3.31982867534575));
#40366=CARTESIAN_POINT('Ctrl Pts',(7.53097186865001,0.667393780433987,3.78032341303133));
#40367=CARTESIAN_POINT('Ctrl Pts',(7.57868770471284,0.545730043505963,4.44255054095139));
#40368=CARTESIAN_POINT('Ctrl Pts',(7.62640354077568,-0.077085990144297,
4.69837669746149));
#40369=CARTESIAN_POINT('Ctrl Pts',(7.67411937683852,-0.629112772588521,
4.31287278685955));
#40370=CARTESIAN_POINT('Ctrl Pts',(7.72183521290136,-0.603415615998442,
3.64005298187887));
#40371=CARTESIAN_POINT('Ctrl Pts',(7.76955104896419,-0.0235926144000291,
3.29777806215626));
#40372=CARTESIAN_POINT('Ctrl Pts',(7.81726688502703,0.577895847971041,3.60036435301798));
#40373=CARTESIAN_POINT('Ctrl Pts',(7.86498272108987,0.648693661106154,4.26994220769392));
#40374=CARTESIAN_POINT('Ctrl Pts',(7.9126985571527,0.123786103798515,4.6916279794467));
#40375=CARTESIAN_POINT('Ctrl Pts',(7.96041439321555,-0.514796137313916,
4.47818113561083));
#40376=CARTESIAN_POINT('Ctrl Pts',(8.00813022927838,-0.680633164378164,
3.82561319718015));
#40377=CARTESIAN_POINT('Ctrl Pts',(8.05584606534123,-0.221434283704469,
3.33318734306526));
#40378=CARTESIAN_POINT('Ctrl Pts',(8.10356190140405,0.441111106898351,3.45310581204486));
#40379=CARTESIAN_POINT('Ctrl Pts',(8.1512777374669,0.698577380670183,4.07524562887252));
#40380=CARTESIAN_POINT('Ctrl Pts',(8.19899357352974,0.314529296777622,4.62828622690367));
#40381=CARTESIAN_POINT('Ctrl Pts',(8.24670940959258,-0.358355880000973,
4.60436191534297));
#40382=CARTESIAN_POINT('Ctrl Pts',(8.29442524565541,-0.70215733816079,4.02544275761943));
#40383=CARTESIAN_POINT('Ctrl Pts',(8.34214108171825,-0.401156908608127,
3.42315912408683));
#40384=CARTESIAN_POINT('Ctrl Pts',(8.3898569177811,0.268232082711808,3.35059734274305));
#40385=CARTESIAN_POINT('Ctrl Pts',(8.43757275384392,0.691299425196396,3.8743920139026));
#40386=CARTESIAN_POINT('Ctrl Pts',(8.48528858990677,0.479535868514212,4.51353443142269));
#40387=CARTESIAN_POINT('Ctrl Pts',(8.53300442596961,-0.172592854832336,
4.68109027882443));
#40388=CARTESIAN_POINT('Ctrl Pts',(8.58072026203244,-0.66622690390392,4.22319044326068));
#40389=CARTESIAN_POINT('Ctrl Pts',(8.62843609809529,-0.548054535901959,
3.56033138942427));
#40390=CARTESIAN_POINT('Ctrl Pts',(8.67615193415812,0.0734047453217555,
3.30122678585069));
#40391=CARTESIAN_POINT('Ctrl Pts',(8.72386777022095,0.627455319439314,3.68381637683837));
#40392=CARTESIAN_POINT('Ctrl Pts',(8.7715836062838,0.605304019074675,4.35676225408577));
#40393=CARTESIAN_POINT('Ctrl Pts',(8.81929944234663,0.0272927241942496,
4.70208786391332));
#40394=CARTESIAN_POINT('Ctrl Pts',(8.86701527840948,-0.575781899266294,
4.40267538529889));
#40395=CARTESIAN_POINT('Ctrl Pts',(8.9147311144723,-0.650107145087294,3.73347990440727));
#40396=CARTESIAN_POINT('Ctrl Pts',(8.96244695053515,-0.127428996390418,
3.30903392823725));
#40397=CARTESIAN_POINT('Ctrl Pts',(9.01016278659798,0.512269160438921,3.51911272764658));
#40398=CARTESIAN_POINT('Ctrl Pts',(9.05787862266082,0.681542664962993,4.17079770865984));
#40399=CARTESIAN_POINT('Ctrl Pts',(9.10559445872366,0.224945053369686,4.66563652575022));
#40400=CARTESIAN_POINT('Ctrl Pts',(9.1533102947865,-0.438223061957547,4.54921107910972));
#40401=CARTESIAN_POINT('Ctrl Pts',(9.20102613084934,-0.698964196560635,
3.92843664782408));
#40402=CARTESIAN_POINT('Ctrl Pts',(9.24874196691217,-0.317835754515511,
3.3733799439853));
#40403=CARTESIAN_POINT('Ctrl Pts',(9.29645780297501,0.355166151432911,3.39375807937372));
#40404=CARTESIAN_POINT('Ctrl Pts',(9.34417363903786,0.702013515586798,3.97085749870423));
#40405=CARTESIAN_POINT('Ctrl Pts',(9.39188947510068,0.404191066510942,4.57471892538967));
#40406=CARTESIAN_POINT('Ctrl Pts',(9.43960531116354,-0.264806258220881,
4.65080711970243));
#40407=CARTESIAN_POINT('Ctrl Pts',(9.48732114722635,-0.690627921460452,
4.12924912203773));
#40408=CARTESIAN_POINT('Ctrl Pts',(9.53503698328922,-0.482235337746388,
3.48899966685243));
#40409=CARTESIAN_POINT('Ctrl Pts',(9.58275281935202,0.169001376764621,3.31800968034731));
#40410=CARTESIAN_POINT('Ctrl Pts',(9.63046865541491,0.665041526572246,3.77330189814918));
#40411=CARTESIAN_POINT('Ctrl Pts',(9.6781844914777,0.550363809549371,4.43677447107931));
#40412=CARTESIAN_POINT('Ctrl Pts',(9.72590032754056,-0.0697214622184181,
4.69915032657822));
#40413=CARTESIAN_POINT('Ctrl Pts',(9.7736161636034,-0.625780442428439,4.31948567936979));
#40414=CARTESIAN_POINT('Ctrl Pts',(9.82133199966623,-0.607175613486645,
3.64643241687702));
#40415=CARTESIAN_POINT('Ctrl Pts',(9.86904783572907,-0.030992076082374,
3.29806570630264));
#40416=CARTESIAN_POINT('Ctrl Pts',(9.91676367179191,0.573651961662729,3.59429605827795));
#40417=CARTESIAN_POINT('Ctrl Pts',(9.96447950785474,0.651502576242943,4.26309058249416));
#40418=CARTESIAN_POINT('Ctrl Pts',(10.0121953439176,0.131068350403577,4.69028497663703));
#40419=CARTESIAN_POINT('Ctrl Pts',(10.0599111799804,-0.50972795835719,4.48358005533451));
#40420=CARTESIAN_POINT('Ctrl Pts',(10.1076270160433,-0.682433239785766,
3.83279612838271));
#40421=CARTESIAN_POINT('Ctrl Pts',(10.1553428521061,-0.228449576533966,
3.33555808949935));
#40422=CARTESIAN_POINT('Ctrl Pts',(10.2030586881689,0.435322847997542,3.44848728078164));
#40423=CARTESIAN_POINT('Ctrl Pts',(10.2507745242318,0.699331602909907,4.06787908823615));
#40424=CARTESIAN_POINT('Ctrl Pts',(10.2984903602946,0.321133386270249,4.62493648450936));
#40425=CARTESIAN_POINT('Ctrl Pts',(10.3462061963575,-0.351966560253669,
4.60810509117381));
#40426=CARTESIAN_POINT('Ctrl Pts',(10.3939220324203,-0.701850198794989,
4.03284143571381));
#40427=CARTESIAN_POINT('Ctrl Pts',(10.4416378684831,-0.407214000429435,
3.42741898450738));
#40428=CARTESIAN_POINT('Ctrl Pts',(10.489353704546,0.261373080323254,3.34780649011919));
#40429=CARTESIAN_POINT('Ctrl Pts',(10.5370695406088,0.689937239673316,3.86711333114163));
#40430=CARTESIAN_POINT('Ctrl Pts',(10.5847853766716,0.484921415782374,4.50845204490092));
#40431=CARTESIAN_POINT('Ctrl Pts',(10.6325012127345,-0.165405205696588,
4.68287142228737));
#40432=CARTESIAN_POINT('Ctrl Pts',(10.6802170487973,-0.66383768169814,4.23019946525991));
#40433=CARTESIAN_POINT('Ctrl Pts',(10.7279328848602,-0.552657800140614,
3.5661317972102));
#40434=CARTESIAN_POINT('Ctrl Pts',(10.775648720923,0.0660362430193439,3.30049197570278));
#40435=CARTESIAN_POINT('Ctrl Pts',(10.8233645569858,0.624088188116435,3.67722113622194));
#40436=CARTESIAN_POINT('Ctrl Pts',(10.8710803930487,0.609030347235101,4.3503630939397));
#40437=CARTESIAN_POINT('Ctrl Pts',(10.9187962291115,0.0346905673513346,
4.70176123146349));
#40438=CARTESIAN_POINT('Ctrl Pts',(10.9665120651743,-0.57150609431415,4.40872123214985));
#40439=CARTESIAN_POINT('Ctrl Pts',(11.0142279012372,-0.65287991581936,3.74034623636848));
#40440=CARTESIAN_POINT('Ctrl Pts',(11.0619437373,-0.134704064778877,3.31041528701663));
#40441=CARTESIAN_POINT('Ctrl Pts',(11.1096595733629,0.507172601636502,3.51374059022208));
#40442=CARTESIAN_POINT('Ctrl Pts',(11.1573754094257,0.68330486411552,4.16360539148934));
#40443=CARTESIAN_POINT('Ctrl Pts',(11.2050912454885,0.231947755880478,4.66322884435941));
#40444=CARTESIAN_POINT('Ctrl Pts',(11.2528070815514,-0.432410545554582,
4.55379904436673));
#40445=CARTESIAN_POINT('Ctrl Pts',(11.3005229176142,-0.699679589515398,
3.93580706063847));
#40446=CARTESIAN_POINT('Ctrl Pts',(11.348238753677,-0.324422100469907,3.37676444086124));
#40447=CARTESIAN_POINT('Ctrl Pts',(11.3959545897399,0.348757195312759,3.39004862475285));
#40448=CARTESIAN_POINT('Ctrl Pts',(11.4436704258027,0.701667392320496,3.9634605418422));
#40449=CARTESIAN_POINT('Ctrl Pts',(11.4913862618656,0.410225626419724,4.57042720558968));
#40450=CARTESIAN_POINT('Ctrl Pts',(11.5391020979284,-0.257932644354891,
4.65356178929341));
#40451=CARTESIAN_POINT('Ctrl Pts',(11.5868179339912,-0.689227399014534,
4.13652052554825));
#40452=CARTESIAN_POINT('Ctrl Pts',(11.6345337700541,-0.487594028032435,
3.49411036255383));
#40453=CARTESIAN_POINT('Ctrl Pts',(11.6822496061169,0.161804441490335,3.31626643773886));
#40454=CARTESIAN_POINT('Ctrl Pts',(11.7299654421798,0.662615402711184,3.76630556374144));
#40455=CARTESIAN_POINT('Ctrl Pts',(11.7776812782426,0.554936443973853,4.43094988641136));
#40456=CARTESIAN_POINT('Ctrl Pts',(11.8253971143054,-0.062349190059417,
4.69984629737339));
#40457=CARTESIAN_POINT('Ctrl Pts',(11.8731129503683,-0.622378603495518,
4.32606308493799));
#40458=CARTESIAN_POINT('Ctrl Pts',(11.9208287864311,-0.610868168815925,
3.65285112447858));
#40459=CARTESIAN_POINT('Ctrl Pts',(11.9685446224939,-0.0383880952977111,
3.29843131798253));
#40460=CARTESIAN_POINT('Ctrl Pts',(12.0162604585568,0.569344356809164,3.58827282720487));
#40461=CARTESIAN_POINT('Ctrl Pts',(12.0639762946196,0.654239125569198,4.25620973444184));
#40462=CARTESIAN_POINT('Ctrl Pts',(12.1116921306825,0.138336038556134,4.68886530024737));
#40463=CARTESIAN_POINT('Ctrl Pts',(12.1594079667453,-0.50460316123658,4.48892526128066));
#40464=CARTESIAN_POINT('Ctrl Pts',(12.2071238028081,-0.684157513748105,
3.83999763179777));
#40465=CARTESIAN_POINT('Ctrl Pts',(12.254839638871,-0.235439494268261,3.33800263898788));
#40466=CARTESIAN_POINT('Ctrl Pts',(12.3025554749338,0.429486235500398,3.44393000893412));
#40467=CARTESIAN_POINT('Ctrl Pts',(12.3502713109967,0.700008146713868,4.06050500791278));
#40468=CARTESIAN_POINT('Ctrl Pts',(12.3979871470595,0.327701805790174,4.62151732713591));
#40469=CARTESIAN_POINT('Ctrl Pts',(12.4457029831223,-0.345538145731053,
4.61178072157682));
#40470=CARTESIAN_POINT('Ctrl Pts',(12.4934188191852,-0.701465101239671,
4.04023646593735));
#40471=CARTESIAN_POINT('Ctrl Pts',(12.541134655248,-0.413225860851952,3.43174244451));
#40472=CARTESIAN_POINT('Ctrl Pts',(12.5888504913108,0.254485045853264,3.34508808005552));
#40473=CARTESIAN_POINT('Ctrl Pts',(12.6365663273737,0.688498419195676,3.85984940880123));
#40474=CARTESIAN_POINT('Ctrl Pts',(12.6842821634365,0.490253100280801,4.50331318193882));
#40475=CARTESIAN_POINT('Ctrl Pts',(12.7319979994994,-0.158199184135511,
4.68457671563321));
#40476=CARTESIAN_POINT('Ctrl Pts',(12.7797138355622,-0.661374723552845,
4.23718291779492));
#40477=CARTESIAN_POINT('Ctrl Pts',(12.827429671625,-0.557199677773407,3.57198039701723));
#40478=CARTESIAN_POINT('Ctrl Pts',(12.8751455076879,0.058660405724426,3.29983486358678));
#40479=CARTESIAN_POINT('Ctrl Pts',(12.9228613437507,0.62065173603916,3.67066174834999));
#40480=CARTESIAN_POINT('Ctrl Pts',(12.9705771798135,0.612689027194643,4.34392501712378));
#40481=CARTESIAN_POINT('Ctrl Pts',(13.0182930158764,0.0420845572448178,
4.7013566507062));
#40482=CARTESIAN_POINT('Ctrl Pts',(13.0660088519392,-0.567166809177069,
4.4147216801859));
#40483=CARTESIAN_POINT('Ctrl Pts',(13.1137246880021,-0.655580167748548,
3.74724140943759));
#40484=CARTESIAN_POINT('Ctrl Pts',(13.1614405240649,-0.141964170879043,
3.31187324159358));
#40485=CARTESIAN_POINT('Ctrl Pts',(13.2091563601277,0.502019708508231,3.50842246418533));
#40486=CARTESIAN_POINT('Ctrl Pts',(13.2568721961906,0.684991165006287,4.15639490180834));
#40487=CARTESIAN_POINT('Ctrl Pts',(13.3045880322534,0.238924694735218,4.66074749465585));
#40488=CARTESIAN_POINT('Ctrl Pts',(13.3523038683163,-0.426549999040181,
4.55832549625387));
#40489=CARTESIAN_POINT('Ctrl Pts',(13.4000197043791,-0.700317265381609,
3.94318460369993));
#40490=CARTESIAN_POINT('Ctrl Pts',(13.4477355404419,-0.330972411156884,
3.38021816378559));
#40491=CARTESIAN_POINT('Ctrl Pts',(13.4954513765048,0.342309500898352,3.3864069206363));
#40492=CARTESIAN_POINT('Ctrl Pts',(13.5431672125676,0.70124333116994,3.95606764360979));
#40493=CARTESIAN_POINT('Ctrl Pts',(13.5908830486304,0.416214620412595,4.5660721254426));
#40494=CARTESIAN_POINT('Ctrl Pts',(13.6385988846933,-0.251030380554765,
4.65624386434224));
#40495=CARTESIAN_POINT('Ctrl Pts',(13.6863147207561,-0.687750320459788,
4.14377676500662));
#40496=CARTESIAN_POINT('Ctrl Pts',(13.734030556819,-0.492898558687668,3.49927725007553));
#40497=CARTESIAN_POINT('Ctrl Pts',(13.7817463928818,0.15458953374652,3.31459914100992));
#40498=CARTESIAN_POINT('Ctrl Pts',(13.8294622289446,0.660115678675556,3.75933518700271));
#40499=CARTESIAN_POINT('Ctrl Pts',(13.8771780650075,0.559447438691528,4.42507743387505));
#40500=CARTESIAN_POINT('Ctrl Pts',(13.9248939010703,-0.0549699924482557,
4.7004645325629));
#40501=CARTESIAN_POINT('Ctrl Pts',(13.9726097371331,-0.61890763370075,4.33260427296601));
#40502=CARTESIAN_POINT('Ctrl Pts',(14.020325573196,-0.614492871807821,3.65930839172987));
#40503=CARTESIAN_POINT('Ctrl Pts',(14.0680414092588,-0.0457798505455885,
3.29887485658241));
#40504=CARTESIAN_POINT('Ctrl Pts',(14.1157572453217,0.564973511886205,3.58229532883235));
#40505=CARTESIAN_POINT('Ctrl Pts',(14.1634730813845,0.656903005118004,4.24930042782804));
#40506=CARTESIAN_POINT('Ctrl Pts',(14.2111889174473,0.145588360997982,4.6873691079691));
#40507=CARTESIAN_POINT('Ctrl Pts',(14.2589047535102,-0.499422315191365,
4.49421615972892));
#40508=CARTESIAN_POINT('Ctrl Pts',(14.306620589573,-0.685805794740406,3.8472169075166));
#40509=CARTESIAN_POINT('Ctrl Pts',(14.3543364256359,-0.242403260500786,
3.34052072000184));
#40510=CARTESIAN_POINT('Ctrl Pts',(14.4020522616987,0.423601917710294,3.43943450270243));
#40511=CARTESIAN_POINT('Ctrl Pts',(14.4497680977615,0.700606936934704,4.05312420698026));
#40512=CARTESIAN_POINT('Ctrl Pts',(14.4974839338244,0.334233825748585,4.61802913456711));
#40513=CARTESIAN_POINT('Ctrl Pts',(14.5451997698872,-0.339071350470923,
4.61538839828042));
#40514=CARTESIAN_POINT('Ctrl Pts',(14.59291560595,-0.701002088269634,4.04762702688518));
#40515=CARTESIAN_POINT('Ctrl Pts',(14.6406314420129,-0.419191822106764,
3.43612902386528));
#40516=CARTESIAN_POINT('Ctrl Pts',(14.6883472780757,0.24756874439201,3.34244241450009));
#40517=CARTESIAN_POINT('Ctrl Pts',(14.7360631141386,0.686983123580828,3.85260105372344));
#40518=CARTESIAN_POINT('Ctrl Pts',(14.7837789502014,0.495530329791292,4.49811841333687));
#40519=CARTESIAN_POINT('Ctrl Pts',(14.8314947862642,-0.150975590559777,
4.68620596944608));
#40520=CARTESIAN_POINT('Ctrl Pts',(14.8792106223271,-0.658838303041738,
4.24414002517693));
#40521=CARTESIAN_POINT('Ctrl Pts',(14.9269264583899,-0.561679664310124,
3.57787653921065));
#40522=CARTESIAN_POINT('Ctrl Pts',(14.9746422944528,0.0512780527100071,
3.29925552249156));
#40523=CARTESIAN_POINT('Ctrl Pts',(15.0223581305156,0.617146344912281,3.6641389418082));
#40524=CARTESIAN_POINT('Ctrl Pts',(15.0700739665784,0.616279652564493,4.337448738749));
#40525=CARTESIAN_POINT('Ctrl Pts',(15.1177898026413,0.0494738725853903,
4.70087416658037));
#40526=CARTESIAN_POINT('Ctrl Pts',(15.1655056387041,-0.562764525842253,
4.42067606290572));
#40527=CARTESIAN_POINT('Ctrl Pts',(15.2132214747669,-0.658207600943685,
3.75416465773151));
#40528=CARTESIAN_POINT('Ctrl Pts',(15.2609373108298,-0.14920850827279,3.31340763002542));
#40529=CARTESIAN_POINT('Ctrl Pts',(15.3086531468926,0.496811053413015,3.50315894024854));
#40530=CARTESIAN_POINT('Ctrl Pts',(15.3563689829554,0.686601380328997,4.14916704052379));
#40531=CARTESIAN_POINT('Ctrl Pts',(15.4040848190183,0.245875094968658,4.6581927522561));
#40532=CARTESIAN_POINT('Ctrl Pts',(15.4518006550811,-0.420642073376032,
4.56278993199436));
#40533=CARTESIAN_POINT('Ctrl Pts',(15.499516491144,-0.700877153329261,3.95056845754601));
#40534=CARTESIAN_POINT('Ctrl Pts',(15.5472323272068,-0.337485958999024,
3.3837407291352));
#40535=CARTESIAN_POINT('Ctrl Pts',(15.5949481632696,0.335823784368978,3.38283337152726));
#40536=CARTESIAN_POINT('Ctrl Pts',(15.6426639993325,0.70074137923783,3.94867962517506));
#40537=CARTESIAN_POINT('Ctrl Pts',(15.6903798353953,0.422157383260532,4.56165416869007));
#40538=CARTESIAN_POINT('Ctrl Pts',(15.7380956714582,-0.244100233491204,
4.65885304693675));
#40539=CARTESIAN_POINT('Ctrl Pts',(15.785811507521,-0.686196849863089,4.15101703442422));
#40540=CARTESIAN_POINT('Ctrl Pts',(15.8335273435838,-0.498148340509996,
3.50449975550414));
#40541=CARTESIAN_POINT('Ctrl Pts',(15.8812431796467,0.147357454930898,3.3130079753559));
#40542=CARTESIAN_POINT('Ctrl Pts',(15.9289590157095,0.657542632122849,3.75239154216938));
#40543=CARTESIAN_POINT('Ctrl Pts',(15.9766748517723,0.563896292642505,4.41915776575455));
#40544=CARTESIAN_POINT('Ctrl Pts',(16.0243906878352,-0.0475846890311933,
4.70100496347609));
#40545=CARTESIAN_POINT('Ctrl Pts',(16.072106523898,-0.615367918582998,4.33910851688972));
#40546=CARTESIAN_POINT('Ctrl Pts',(16.1198223599609,-0.618049319847516,
3.66580350138828));
#40547=CARTESIAN_POINT('Ctrl Pts',(16.1675381960237,-0.0531665207849041,
3.29939627283611));
#40548=CARTESIAN_POINT('Ctrl Pts',(16.2152540320865,0.560539912386559,3.57636422711252));
#40549=CARTESIAN_POINT('Ctrl Pts',(16.2629698681494,0.659493918998266,4.24236343010572));
#40550=CARTESIAN_POINT('Ctrl Pts',(16.3106857042122,0.152824512175573,4.68579656599215));
#40551=CARTESIAN_POINT('Ctrl Pts',(16.358401540275,-0.494185995685336,4.49945216299141));
#40552=CARTESIAN_POINT('Ctrl Pts',(16.4061173763379,-0.687377899679438,
3.85445315365633));
#40553=CARTESIAN_POINT('Ctrl Pts',(16.4538332124007,-0.249340101729437,
3.34311205284473));
#40554=CARTESIAN_POINT('Ctrl Pts',(16.5015490484636,0.417670548229327,3.43500126142608));
#40555=CARTESIAN_POINT('Ctrl Pts',(16.5492648845264,0.701127907061643,4.04573750526291));
#40556=CARTESIAN_POINT('Ctrl Pts',(16.5969807205892,0.340728720599694,4.61447229425484));
#40557=CARTESIAN_POINT('Ctrl Pts',(16.6446965566521,-0.3325668927742,4.61892772056098));
#40558=CARTESIAN_POINT('Ctrl Pts',(16.6924123927149,-0.700461211314163,
4.05501229764889));
#40559=CARTESIAN_POINT('Ctrl Pts',(16.7401282287777,-0.425111221523205,
3.4405782353328));
#40560=CARTESIAN_POINT('Ctrl Pts',(16.7878440648406,0.240624944169445,3.3398697873209));
#40561=CARTESIAN_POINT('Ctrl Pts',(16.8355599009034,0.685391521140609,3.84536907102113));
#40562=CARTESIAN_POINT('Ctrl Pts',(16.8832757369663,0.500752518144239,4.49286831610534));
#40563=CARTESIAN_POINT('Ctrl Pts',(16.9309915730291,-0.143735227331884,
4.68775900275617));
#40564=CARTESIAN_POINT('Ctrl Pts',(16.978707409092,-0.656228701898373,4.25107001464348));
#40565=CARTESIAN_POINT('Ctrl Pts',(17.0264232451548,-0.566097262135119,
3.58381956887496));
#40566=CARTESIAN_POINT('Ctrl Pts',(17.0741390812176,0.0438900039728252,
3.29875401676759));
#40567=CARTESIAN_POINT('Ctrl Pts',(17.1218549172805,0.613572404098014,3.65765344111895));
#40568=CARTESIAN_POINT('Ctrl Pts',(17.1695707533433,0.619801824515016,4.33093497816967));
#40569=CARTESIAN_POINT('Ctrl Pts',(17.2172865894061,0.0568576926029748,
4.70031383267802));
#40570=CARTESIAN_POINT('Ctrl Pts',(17.265002425469,-0.558299733294432,4.42658371892475));
#40571=CARTESIAN_POINT('Ctrl Pts',(17.3127182615318,-0.66076192356197,3.76111521224867));
#40572=CARTESIAN_POINT('Ctrl Pts',(17.3604340975947,-0.156436272293483,
3.31501828187956));
#40573=CARTESIAN_POINT('Ctrl Pts',(17.4081499336575,0.491547214903555,3.49795060305896));
#40574=CARTESIAN_POINT('Ctrl Pts',(17.4558657697204,0.688135331228569,4.14192261047223));
#40575=CARTESIAN_POINT('Ctrl Pts',(17.5035816057831,0.252798184563325,4.65556490092881));
#40576=CARTESIAN_POINT('Ctrl Pts',(17.551297441846,-0.414687424786488,4.56719185569987));
#40577=CARTESIAN_POINT('Ctrl Pts',(17.5990132779088,-0.701359191168653,
3.95795780201324));
#40578=CARTESIAN_POINT('Ctrl Pts',(17.6467291139717,-0.343962020502345,
3.38733174564023));
#40579=CARTESIAN_POINT('Ctrl Pts',(17.6944449500345,0.329300766127249,3.37932837435862));
#40580=CARTESIAN_POINT('Ctrl Pts',(17.7421607860974,0.700161592278611,3.94129730716402));
#40581=CARTESIAN_POINT('Ctrl Pts',(17.7898766221602,0.428053254869629,4.55717382605774));
#40582=CARTESIAN_POINT('Ctrl Pts',(17.837592458223,-0.23714297293205,4.66138904726133));
#40583=CARTESIAN_POINT('Ctrl Pts',(17.8853082942859,-0.684567159776581,
4.15824052958626));
#40584=CARTESIAN_POINT('Ctrl Pts',(17.9330241303487,-0.503342790378573,
3.50977729874859));
#40585=CARTESIAN_POINT('Ctrl Pts',(17.9807399664116,0.140109008348428,3.31149311751593));
#40586=CARTESIAN_POINT('Ctrl Pts',(18.0284558024744,0.654896548854854,3.7454754005085));
#40587=CARTESIAN_POINT('Ctrl Pts',(18.0761716385372,0.568282511669218,4.41319153957849));
#40588=CARTESIAN_POINT('Ctrl Pts',(18.1238874746001,-0.040194100132671,
4.70146753008449));
#40589=CARTESIAN_POINT('Ctrl Pts',(18.1716033106629,-0.611759851316993,
4.34557509424858));
#40590=CARTESIAN_POINT('Ctrl Pts',(18.2193191467258,-0.621537117901666,
3.67233573200791));
#40591=CARTESIAN_POINT('Ctrl Pts',(18.2670349827885,-0.0605472855394143,
3.29999550882718));
#40592=CARTESIAN_POINT('Ctrl Pts',(18.3147508188514,0.556044050773433,3.57048018084402));
#40593=CARTESIAN_POINT('Ctrl Pts',(18.3624666549143,0.662011579423562,4.23539951180373));
#40594=CARTESIAN_POINT('Ctrl Pts',(18.4101824909771,0.160043688331546,4.684147848987));
#40595=CARTESIAN_POINT('Ctrl Pts',(18.4578983270399,-0.488894784343999,
4.50463268947774));
#40596=CARTESIAN_POINT('Ctrl Pts',(18.5056141631028,-0.68887365394326,3.86170556644909));
#40597=CARTESIAN_POINT('Ctrl Pts',(18.5533299991656,-0.256249247442801,
3.34577634968359));
#40598=CARTESIAN_POINT('Ctrl Pts',(18.6010458352284,0.41169278588589,3.4306307775285));
#40599=CARTESIAN_POINT('Ctrl Pts',(18.6487616712913,0.701570999227752,4.03834572324048));
#40600=CARTESIAN_POINT('Ctrl Pts',(18.6964775073541,0.347185768921481,4.6108472012761));
#40601=CARTESIAN_POINT('Ctrl Pts',(18.744193343417,-0.326025495125306,4.62239829528727));
#40602=CARTESIAN_POINT('Ctrl Pts',(18.7919091794798,-0.699842530451103,
4.06239145790787));
#40603=CARTESIAN_POINT('Ctrl Pts',(18.8396250155426,-0.430983401602837,
3.44508958471478));
#40604=CARTESIAN_POINT('Ctrl Pts',(18.8873408516055,0.233654416470602,3.33737048427408));
#40605=CARTESIAN_POINT('Ctrl Pts',(18.9350566876683,0.683723788661416,3.83815426398688));
#40606=CARTESIAN_POINT('Ctrl Pts',(18.9827725237312,0.505919085286118,4.48756347340344));
#40607=CARTESIAN_POINT('Ctrl Pts',(19.030488359794,-0.136478898681533,4.68923564305365));
#40608=CARTESIAN_POINT('Ctrl Pts',(19.0782041958568,-0.653546209976322,
4.2579721164561));
#40609=CARTESIAN_POINT('Ctrl Pts',(19.1259200319197,-0.570451980578726,
3.58980882586423));
#40610=CARTESIAN_POINT('Ctrl Pts',(19.1736358679825,0.0364970801727598,
3.29833040216201));
#40611=CARTESIAN_POINT('Ctrl Pts',(19.2213517040453,0.609930310515188,3.65120596658116));
#40612=CARTESIAN_POINT('Ctrl Pts',(19.2690675401082,0.623255151928734,4.32438445905389));
#40613=CARTESIAN_POINT('Ctrl Pts',(19.316783376171,0.0642351969327414,4.69967571095415));
#40614=CARTESIAN_POINT('Ctrl Pts',(19.3644992122339,-0.553772927074266,
4.43244399258532));
#40615=CARTESIAN_POINT('Ctrl Pts',(19.4122150482967,-0.663242852612724,
3.76809229994096));
#40616=CARTESIAN_POINT('Ctrl Pts',(19.4599308843595,-0.163646658734412,
3.3167050201661));
#40617=CARTESIAN_POINT('Ctrl Pts',(19.5076467204224,0.486228775054438,3.49279802752061));
#40618=CARTESIAN_POINT('Ctrl Pts',(19.5553625564852,0.689592852244711,4.13466242315333));
#40619=CARTESIAN_POINT('Ctrl Pts',(19.6030783925481,0.259693185238344,4.65286421968052));
#40620=CARTESIAN_POINT('Ctrl Pts',(19.6507942286109,-0.408686697131164,
4.57153080275077));
#40621=CARTESIAN_POINT('Ctrl Pts',(19.6985100646738,-0.701763358503738,
3.96535177039745));
#40622=CARTESIAN_POINT('Ctrl Pts',(19.7462259007365,-0.350399813749482,
3.39099090115443));
#40623=CARTESIAN_POINT('Ctrl Pts',(19.7939417367994,0.322741052541778,3.37589215469092));
#40624=CARTESIAN_POINT('Ctrl Pts',(19.8416575728622,0.699504257835039,3.93392181877779));
#40625=CARTESIAN_POINT('Ctrl Pts',(19.8893734089251,0.433901159015506,4.55263101135276));
#40626=CARTESIAN_POINT('Ctrl Pts',(19.9370892449879,-0.23015857608315,4.663852686053));
#40627=CARTESIAN_POINT('Ctrl Pts',(19.9848050810507,-0.682862933423436,
4.16544436654047));
#40628=CARTESIAN_POINT('Ctrl Pts',(20.0325209171136,-0.508478494849655,
3.51511322409123));
#40629=CARTESIAN_POINT('Ctrl Pts',(20.0802367531764,0.132839643288252,3.31004731418368));
#40630=CARTESIAN_POINT('Ctrl Pts',(20.1279525892393,0.652187835720725,3.73860154375571));
#40631=CARTESIAN_POINT('Ctrl Pts',(20.1756684253021,0.572586513039731,4.4071529569233));
#40632=CARTESIAN_POINT('Ctrl Pts',(20.2233842613649,-0.0327629883405684,
4.70190215105461));
#40633=CARTESIAN_POINT('Ctrl Pts',(20.2711000974278,-0.608151935097038,
4.35190888358257));
#40634=CARTESIAN_POINT('Ctrl Pts',(20.3188159334906,-0.624827148513498,
3.67908301574286));
#40635=CARTESIAN_POINT('Ctrl Pts',(20.3665317695535,-0.0681655280739813,
3.30033184185188));
#40636=CARTESIAN_POINT('Ctrl Pts',(20.4142476056163,0.551956769749184,3.56531418539817));
#40637=CARTESIAN_POINT('Ctrl Pts',(20.4540108023353,0.644905999548395,4.11665253813788));
#40638=CARTESIAN_POINT('Ctrl Pts',(20.4858213597105,0.416382673412033,4.45708139504444));
#40639=CARTESIAN_POINT('Ctrl Pts',(20.509679277742,0.148137151166912,4.60177085628536));
#40640=CARTESIAN_POINT('Ctrl Pts',(20.5335371957734,-0.159214575149101,
4.59858486262053));
#40641=CARTESIAN_POINT('Ctrl Pts',(20.5573951138048,-0.426074836374489,
4.44942877587387));
#40642=CARTESIAN_POINT('Ctrl Pts',(20.5812530318362,-0.589577924844292,
4.19016123618585));
#40643=CARTESIAN_POINT('Ctrl Pts',(20.6051109498677,-0.608473233900696,
3.88450759853215));
#40644=CARTESIAN_POINT('Ctrl Pts',(20.6289688678991,-0.478813304308425,
3.60703485797333));
#40645=CARTESIAN_POINT('Ctrl Pts',(20.6528267859305,-0.231947052182395,
3.42568465323223));
#40646=CARTESIAN_POINT('Ctrl Pts',(20.6766847039619,0.0715712039811096,
3.38475332414555));
#40647=CARTESIAN_POINT('Ctrl Pts',(20.7005426219933,0.357622970648114,3.49427550111266));
#40648=CARTESIAN_POINT('Ctrl Pts',(20.7244005400248,0.556207844932749,3.72745636179159));
#40649=CARTESIAN_POINT('Ctrl Pts',(20.7482584580561,0.618794460414918,4.02728407199912));
#40650=CARTESIAN_POINT('Ctrl Pts',(20.7721163760876,0.530063832205264,4.32043875618714));
#40651=CARTESIAN_POINT('Ctrl Pts',(20.7959742941189,0.311720881859749,4.53523813880796));
#40652=CARTESIAN_POINT('Ctrl Pts',(20.8198322121505,0.01715224242355,4.619156844639));
#40653=CARTESIAN_POINT('Ctrl Pts',(20.8436901301818,-0.281609823618225,
4.55167503361081));
#40654=CARTESIAN_POINT('Ctrl Pts',(20.8675480482133,-0.511511021444125,
4.34929354512778));
#40655=CARTESIAN_POINT('Ctrl Pts',(20.8914059662447,-0.616333626991818,
4.06150032559224));
#40656=CARTESIAN_POINT('Ctrl Pts',(20.9152638842761,-0.570445985619195,
3.75866857192897));
#40657=CARTESIAN_POINT('Ctrl Pts',(20.9391218023075,-0.385068702031786,
3.51484894167474));
#40658=CARTESIAN_POINT('Ctrl Pts',(20.9629797203389,-0.105531663562905,
3.38966195221662));
#40659=CARTESIAN_POINT('Ctrl Pts',(20.9868376383704,0.199810758127152,3.41371924506628));
#40660=CARTESIAN_POINT('Ctrl Pts',(21.0106955564018,0.456293997792742,3.58113815016051));
#40661=CARTESIAN_POINT('Ctrl Pts',(21.0345534744332,0.60120093052663,3.85098018832832));
#40662=CARTESIAN_POINT('Ctrl Pts',(21.0584113924646,0.599097856858477,4.15726162902184));
#40663=CARTESIAN_POINT('Ctrl Pts',(21.082269310496,0.450499039416452,4.42508831804098));
#40664=CARTESIAN_POINT('Ctrl Pts',(21.1061272285275,0.191740934787398,4.58896933394457));
#40665=CARTESIAN_POINT('Ctrl Pts',(21.1299851465589,-0.113903050943465,
4.60883130459215));
#40666=CARTESIAN_POINT('Ctrl Pts',(21.1538430645903,-0.391694638258801,
4.47981743698434));
#40667=CARTESIAN_POINT('Ctrl Pts',(21.1777009826217,-0.573706216867813,
4.23347513609622));
#40668=CARTESIAN_POINT('Ctrl Pts',(21.2015589006531,-0.615430998064313,
3.9300418046833));
#40669=CARTESIAN_POINT('Ctrl Pts',(21.2254168186846,-0.506666136201032,
3.64371515765586));
#40670=CARTESIAN_POINT('Ctrl Pts',(21.2492747367159,-0.27400760274365,3.44450985958179));
#40671=CARTESIAN_POINT('Ctrl Pts',(21.2731326547474,0.0256532534100022,
3.38113703208972));
#40672=CARTESIAN_POINT('Ctrl Pts',(21.2969905727788,0.319041190319967,3.46909305773936));
#40673=CARTESIAN_POINT('Ctrl Pts',(21.3208484908102,0.534414865691478,3.68687029238709));
#40674=CARTESIAN_POINT('Ctrl Pts',(21.3447064088416,0.619109549231529,3.98121627002784));
#40675=CARTESIAN_POINT('Ctrl Pts',(21.3685643268731,0.552415083779586,4.28015538130547));
#40676=CARTESIAN_POINT('Ctrl Pts',(21.3924222449044,0.350640082858436,4.51058887057447));
#40677=CARTESIAN_POINT('Ctrl Pts',(21.4162801629359,0.0631240304344945,
4.61616947282646));
#40678=CARTESIAN_POINT('Ctrl Pts',(21.4401380809673,-0.239827566894842,
4.57107985485291));
#40679=CARTESIAN_POINT('Ctrl Pts',(21.4639959989987,-0.484134791346583,
4.38634565646493));
#40680=CARTESIAN_POINT('Ctrl Pts',(21.4878539170302,-0.610057871747176,
4.10713942122688));
#40681=CARTESIAN_POINT('Ctrl Pts',(21.5117118350615,-0.586805184862796,
3.80173467907963));
#40682=CARTESIAN_POINT('Ctrl Pts',(21.535569753093,-0.420062646027161,3.5448112085363));
#40683=CARTESIAN_POINT('Ctrl Pts',(21.5594276711244,-0.150603347961132,
3.39919379659958));
#40684=CARTESIAN_POINT('Ctrl Pts',(21.5832855891558,0.155682571034224,3.40048986702667));
#40685=CARTESIAN_POINT('Ctrl Pts',(21.6071435071872,0.423899860703612,3.54838249529388));
#40686=CARTESIAN_POINT('Ctrl Pts',(21.6310014252187,0.588462087630599,3.80670790527556));
#40687=CARTESIAN_POINT('Ctrl Pts',(21.6548593432501,0.609129304746478,4.11229849758833));
#40688=CARTESIAN_POINT('Ctrl Pts',(21.6787172612815,0.480847814502724,4.39042904829107));
#40689=CARTESIAN_POINT('Ctrl Pts',(21.7025751793129,0.234985935581564,4.57308906161293));
#40690=CARTESIAN_POINT('Ctrl Pts',(21.7264330973443,-0.0683364054776661,
4.61561318873779));
#40691=CARTESIAN_POINT('Ctrl Pts',(21.7502910153758,-0.35494863395129,4.5076031222497));
#40692=CARTESIAN_POINT('Ctrl Pts',(21.7741489334072,-0.554766252817153,
4.2754702655401));
#40693=CARTESIAN_POINT('Ctrl Pts',(21.7980068514386,-0.618928411339905,
3.9759774252466));
#40694=CARTESIAN_POINT('Ctrl Pts',(21.82186476947,-0.531745714018629,3.68235875884208));
#40695=CARTESIAN_POINT('Ctrl Pts',(21.8457226875014,-0.314536705157368,
3.46641202827438));
#40696=CARTESIAN_POINT('Ctrl Pts',(21.8695806055329,-0.0204149040773093,
3.3809420914381));
#40697=CARTESIAN_POINT('Ctrl Pts',(21.8934385235643,0.278698897140474,3.44684867604406));
#40698=CARTESIAN_POINT('Ctrl Pts',(21.9172964415957,0.509663226401888,3.6480158268968));
#40699=CARTESIAN_POINT('Ctrl Pts',(21.9411543596271,0.616001013860485,3.93525269592965));
#40700=CARTESIAN_POINT('Ctrl Pts',(21.9650122776585,0.571709773899469,4.23832204448885));
#40701=CARTESIAN_POINT('Ctrl Pts',(21.98887019569,0.387619921158457,4.48311516140836));
#40702=CARTESIAN_POINT('Ctrl Pts',(22.0127281137213,0.108746439139576,4.60977346157076));
#40703=CARTESIAN_POINT('Ctrl Pts',(22.0365860317528,-0.196718509442517,
4.5873255404835));
#40704=CARTESIAN_POINT('Ctrl Pts',(22.0604439497842,-0.454080423961193,
4.42126052632156));
#40705=CARTESIAN_POINT('Ctrl Pts',(22.0843018678156,-0.600407305919173,
4.15218583856754));
#40706=CARTESIAN_POINT('Ctrl Pts',(22.1081597858471,-0.599918246812857,
3.84589756782496));
#40707=CARTESIAN_POINT('Ctrl Pts',(22.1320177038785,-0.452732834916613,
3.57729153941473));
#40708=CARTESIAN_POINT('Ctrl Pts',(22.1558756219099,-0.194841912687001,
3.41204924396571));
#40709=CARTESIAN_POINT('Ctrl Pts',(22.1797335399413,0.110693164578993,3.39057692382254));
#40710=CARTESIAN_POINT('Ctrl Pts',(22.2035914579728,0.389160747889314,3.51812514615901));
#40711=CARTESIAN_POINT('Ctrl Pts',(22.2274493760041,0.572467927805029,3.76350489626149));
#40712=CARTESIAN_POINT('Ctrl Pts',(22.2513072940356,0.615791105677536,4.06671414123586));
#40713=CARTESIAN_POINT('Ctrl Pts',(22.2751652120669,0.508536584364246,4.35360996140145));
#40714=CARTESIAN_POINT('Ctrl Pts',(22.2990231300984,0.276931015980992,4.55403851389998));
#40715=CARTESIAN_POINT('Ctrl Pts',(22.3228810481298,-0.0223917293827815,
4.61898955797298));
#40716=CARTESIAN_POINT('Ctrl Pts',(22.3467389661613,-0.31623908674035,4.53258079431836));
#40717=CARTESIAN_POINT('Ctrl Pts',(22.3705968841927,-0.532757373651304,
4.31594151899069));
#40718=CARTESIAN_POINT('Ctrl Pts',(22.3944548022241,-0.619001969851995,
4.02204593667267));
#40719=CARTESIAN_POINT('Ctrl Pts',(22.4183127202555,-0.553883724721699,
3.72275952141814));
#40720=CARTESIAN_POINT('Ctrl Pts',(22.4421706382869,-0.35332581843718,3.49126595675675));
#40721=CARTESIAN_POINT('Ctrl Pts',(22.4660285563184,-0.0663701307507445,
3.38417172009386));
#40722=CARTESIAN_POINT('Ctrl Pts',(22.4898864743497,0.236814872379406,3.42766427875767));
#40723=CARTESIAN_POINT('Ctrl Pts',(22.5137443923812,0.482092168510832,3.61110849992699));
#40724=CARTESIAN_POINT('Ctrl Pts',(22.5376023104126,0.609484835267769,3.88964730767638));
#40725=CARTESIAN_POINT('Ctrl Pts',(22.561460228444,0.587841786482003,4.19517031382209));
#40726=CARTESIAN_POINT('Ctrl Pts',(22.5853181464754,0.422455543015367,4.45296893898932));
#40727=CARTESIAN_POINT('Ctrl Pts',(22.6091760645069,0.153767157666155,4.60000417439789));
#40728=CARTESIAN_POINT('Ctrl Pts',(22.6330339825383,-0.152521006364708,
4.60032232020799));
#40729=CARTESIAN_POINT('Ctrl Pts',(22.6568919005697,-0.421514535902825,
4.45384478734481));
#40730=CARTESIAN_POINT('Ctrl Pts',(22.6807498186011,-0.587434568575047,
4.19639082134502));
#40731=CARTESIAN_POINT('Ctrl Pts',(22.7046077366325,-0.60971407867596,3.89091209973551));
#40732=CARTESIAN_POINT('Ctrl Pts',(22.728465654664,-0.482895786937606,3.61211183522625));
#40733=CARTESIAN_POINT('Ctrl Pts',(22.7523235726954,-0.23800784887647,3.4281541921173));
#40734=CARTESIAN_POINT('Ctrl Pts',(22.7761814907268,0.0651013135850054,
3.38404091701771));
#40735=CARTESIAN_POINT('Ctrl Pts',(22.8000394087582,0.352249768808992,3.49052260401466));
#40736=CARTESIAN_POINT('Ctrl Pts',(22.8238973267896,0.553345940411564,3.72163220123786));
#40737=CARTESIAN_POINT('Ctrl Pts',(22.8398026054772,0.597082876783669,3.92101540361374));
#40738=CARTESIAN_POINT('Ctrl Pts',(22.847755244821,0.593766187829899,4.01991291515446));
#40739=CARTESIAN_POINT('',(22.8,0.337479661717902,3.51106003648017));
#40740=CARTESIAN_POINT('Ctrl Pts',(22.8,0.337504360408405,3.51101527402275));
#40741=CARTESIAN_POINT('Ctrl Pts',(22.8,0.337610992569967,3.51114843896934));
#40742=CARTESIAN_POINT('Ctrl Pts',(22.8,0.337717562131928,3.51128164981369));
#40743=CARTESIAN_POINT('Ctrl Pts',(22.8,0.337824069051012,3.51141490653789));
#40744=CARTESIAN_POINT('Ctrl Pts',(22.8,0.354145371784291,3.53183539523119));
#40745=CARTESIAN_POINT('Ctrl Pts',(22.8,0.368999739942303,3.55333386321799));
#40746=CARTESIAN_POINT('Ctrl Pts',(22.8,0.382262544471458,3.57576050230915));
#40747=CARTESIAN_POINT('Ctrl Pts',(22.8,0.395177725624396,3.59759933027929));
#40748=CARTESIAN_POINT('Ctrl Pts',(22.8,0.406583379369087,3.62031953557487));
#40749=CARTESIAN_POINT('Ctrl Pts',(22.8,0.416319965152677,3.64376476659274));
#40750=CARTESIAN_POINT('Ctrl Pts',(22.8,0.420499854003763,3.65382973822867));
#40751=CARTESIAN_POINT('Ctrl Pts',(22.8,0.424371599987778,3.66402799385056));
#40752=CARTESIAN_POINT('Ctrl Pts',(22.8,0.42792023461967,3.67434527679585));
#40753=CARTESIAN_POINT('Ctrl Pts',(22.8,0.430015882150509,3.68043815216119));
#40754=CARTESIAN_POINT('Ctrl Pts',(22.8,0.431995626466768,3.68656321156818));
#40755=CARTESIAN_POINT('Ctrl Pts',(22.8,0.433857425300493,3.69271766785326));
#40756=CARTESIAN_POINT('Ctrl Pts',(22.8,0.440667704273582,3.71523007009016));
#40757=CARTESIAN_POINT('Ctrl Pts',(22.8,0.445903532435623,3.73813926926309));
#40758=CARTESIAN_POINT('Ctrl Pts',(22.8,0.449441836754149,3.76130640751661));
#40759=CARTESIAN_POINT('Ctrl Pts',(22.8,0.450038513826676,3.76521316594877));
#40760=CARTESIAN_POINT('Ctrl Pts',(22.8,0.450586822418701,3.76912718643627));
#40761=CARTESIAN_POINT('Ctrl Pts',(22.8,0.451086059471329,3.77304770583064));
#40762=CARTESIAN_POINT('Ctrl Pts',(22.8,0.453684096906641,3.79345015011803));
#40763=CARTESIAN_POINT('Ctrl Pts',(22.8,0.454954433743694,3.81403106227893));
#40764=CARTESIAN_POINT('Ctrl Pts',(22.8,0.45484641916779,3.83463783350426));
#40765=CARTESIAN_POINT('Ctrl Pts',(22.8,0.454808390965019,3.84189276616533));
#40766=CARTESIAN_POINT('Ctrl Pts',(22.8,0.454599381710613,3.84915061719132));
#40767=CARTESIAN_POINT('Ctrl Pts',(22.8,0.454216814112443,3.8564037154462));
#40768=CARTESIAN_POINT('Ctrl Pts',(22.8,0.453866695925276,3.86304160538904));
#40769=CARTESIAN_POINT('Ctrl Pts',(22.8,0.453371644107099,3.86966645154658));
#40770=CARTESIAN_POINT('Ctrl Pts',(22.8,0.452731182295137,3.87626933737115));
#40771=CARTESIAN_POINT('Ctrl Pts',(22.8,0.450713457978438,3.89707120727158));
#40772=CARTESIAN_POINT('Ctrl Pts',(22.8,0.447253508643,3.9176725514372));
#40773=CARTESIAN_POINT('Ctrl Pts',(22.8,0.442312061254715,3.9379035771693));
#40774=CARTESIAN_POINT('Ctrl Pts',(22.8,0.437564183511961,3.95734209977996));
#40775=CARTESIAN_POINT('Ctrl Pts',(22.8,0.431447509288203,3.97643919003209));
#40776=CARTESIAN_POINT('Ctrl Pts',(22.8,0.423915075143768,3.9949978423605));
#40777=CARTESIAN_POINT('Ctrl Pts',(22.8,0.421325190817866,4.00137888225459));
#40778=CARTESIAN_POINT('Ctrl Pts',(22.8,0.418567902041021,4.00769582483512));
#40779=CARTESIAN_POINT('Ctrl Pts',(22.8,0.415641328671541,4.01393920819689));
#40780=CARTESIAN_POINT('Ctrl Pts',(22.6211545887425,-1.51173456864708E-7,
4.59404872180247));
#40781=CARTESIAN_POINT('Ctrl Pts',(22.6251143866744,-0.0492822808754852,
4.59404929162283));
#40782=CARTESIAN_POINT('Ctrl Pts',(22.6290741846063,-0.0985642856931001,
4.58798571459226));
#40783=CARTESIAN_POINT('Ctrl Pts',(22.6330339825383,-0.14630523394925,4.57585637376244));
#40784=CARTESIAN_POINT('Ctrl Pts',(22.6409866218821,-0.242185516210759,
4.55149647592026));
#40785=CARTESIAN_POINT('Ctrl Pts',(22.6489392612259,-0.331850026056775,
4.50267063163255));
#40786=CARTESIAN_POINT('Ctrl Pts',(22.6568919005697,-0.404335619758509,
4.43534871515538));
#40787=CARTESIAN_POINT('Ctrl Pts',(22.6648445399135,-0.476821213460227,
4.36802679867822));
#40788=CARTESIAN_POINT('Ctrl Pts',(22.6727971792573,-0.532127891017642,
4.28220881001161));
#40789=CARTESIAN_POINT('Ctrl Pts',(22.6807498186011,-0.563494481479829,
4.18838669541007));
#40790=CARTESIAN_POINT('Ctrl Pts',(22.6887024579449,-0.594861071942019,
4.09456458080851));
#40791=CARTESIAN_POINT('Ctrl Pts',(22.6966550972887,-0.602287575308989,
3.99273834027202));
#40792=CARTESIAN_POINT('Ctrl Pts',(22.7046077366325,-0.584864445036083,
3.89535850925222));
#40793=CARTESIAN_POINT('Ctrl Pts',(22.7125603759763,-0.567441314763176,
3.79797867823242));
#40794=CARTESIAN_POINT('Ctrl Pts',(22.7205130153201,-0.525168550850394,
3.70504525672934));
#40795=CARTESIAN_POINT('Ctrl Pts',(22.7284656546639,-0.463217512550482,
3.62791893879298));
#40796=CARTESIAN_POINT('Ctrl Pts',(22.7364182940078,-0.401266474250563,
3.5507926208566));
#40797=CARTESIAN_POINT('Ctrl Pts',(22.7443709333516,-0.319637161563486,
3.48947340648693));
#40798=CARTESIAN_POINT('Ctrl Pts',(22.7523235726954,-0.228304311476372,
3.45146158678551));
#40799=CARTESIAN_POINT('Ctrl Pts',(22.7602762120392,-0.136971461389268,
3.41344976708409));
#40800=CARTESIAN_POINT('Ctrl Pts',(22.768228851383,-0.0359350739021178,
3.3987453420509));
#40801=CARTESIAN_POINT('Ctrl Pts',(22.7761814907268,0.062441195712126,3.40914007736714));
#40802=CARTESIAN_POINT('Ctrl Pts',(22.7841209938178,0.160654966376612,3.41951764255099));
#40803=CARTESIAN_POINT('Ctrl Pts',(22.7920604969089,0.256217399931083,3.45491151845628));
#40804=CARTESIAN_POINT('Ctrl Pts',(22.8,0.337504360408238,3.51101527402264));
#40805=CARTESIAN_POINT('Ctrl Pts',(4.,-0.219914231356244,4.35301468169996));
#40806=CARTESIAN_POINT('Ctrl Pts',(4.00793950309107,-0.278596966840389,
4.31645650682028));
#40807=CARTESIAN_POINT('Ctrl Pts',(4.02383164552594,-0.377405665439666,
4.21337674819164));
#40808=CARTESIAN_POINT('Ctrl Pts',(4.04767642730463,-0.433534992178268,
4.00656196868444));
#40809=CARTESIAN_POINT('Ctrl Pts',(4.07153434533603,-0.383670022685343,
3.79803920418254));
#40810=CARTESIAN_POINT('Ctrl Pts',(4.09539226336747,-0.239994733226421,
3.63889579340969));
#40811=CARTESIAN_POINT('Ctrl Pts',(4.11925018139887,-0.0376302499649443,
3.56805514133307));
#40812=CARTESIAN_POINT('Ctrl Pts',(4.1431080994303,0.173933765839147,3.60283521426327));
#40813=CARTESIAN_POINT('Ctrl Pts',(4.16696601746172,0.342967344134064,3.73473372141871));
#40814=CARTESIAN_POINT('Ctrl Pts',(4.19082393549313,0.428135478754777,3.93149662217858));
#40815=CARTESIAN_POINT('Ctrl Pts',(4.21468185352456,0.40861313688017,4.1450106963618));
#40816=CARTESIAN_POINT('Ctrl Pts',(4.23853977155597,0.289173588337559,4.32306558264197));
#40817=CARTESIAN_POINT('Ctrl Pts',(4.25811226835493,0.13317859508208,4.40432939198872));
#40818=CARTESIAN_POINT('Ctrl Pts',(4.26973212581007,0.0319512750557707,
4.41584666103033));
#40819=CARTESIAN_POINT('Ctrl Pts',(4.2733993439214,2.51014653359152E-6,
4.41583996132385));
#40820=CARTESIAN_POINT('Origin',(3.42660065607856,0.,4.));
#40821=CARTESIAN_POINT('Ctrl Pts',(4.,-0.219892372743211,3.64701365460636));
#40822=CARTESIAN_POINT('Ctrl Pts',(4.00795263934381,-0.161099076858729,
3.61038844940468));
#40823=CARTESIAN_POINT('Ctrl Pts',(4.02385791803142,-0.0249198690254346,
3.56711791692558));
#40824=CARTESIAN_POINT('Ctrl Pts',(4.04771583606284,0.185569069288609,3.60813812632505));
#40825=CARTESIAN_POINT('Ctrl Pts',(4.07157375409426,0.350624105231944,3.74494568050885));
#40826=CARTESIAN_POINT('Ctrl Pts',(4.09543167212568,0.429971014252744,3.94413788601839));
#40827=CARTESIAN_POINT('Ctrl Pts',(4.1192895901571,0.40416308778273,4.15698104289539));
#40828=CARTESIAN_POINT('Ctrl Pts',(4.14314750818851,0.279534313346206,4.3314427366163));
#40829=CARTESIAN_POINT('Ctrl Pts',(4.16225119682902,0.125004509401131,4.40624063703925));
#40830=CARTESIAN_POINT('Ctrl Pts',(4.1734022461257,0.0278694809177792,4.41585864517498));
#40831=CARTESIAN_POINT('Ctrl Pts',(4.17660065607858,5.88453344126799E-6,
4.41584444980552));
#40832=CARTESIAN_POINT('Ctrl Pts',(3.95224475517896,-0.314128184302177,
3.49573985500833));
#40833=CARTESIAN_POINT('Ctrl Pts',(3.96019739452277,-0.230138771413741,
3.44341876234755));
#40834=CARTESIAN_POINT('Ctrl Pts',(3.97610267321038,-0.0355993848822847,
3.38160445914153));
#40835=CARTESIAN_POINT('Ctrl Pts',(3.9999605912418,0.265095483172694,3.44020405374152));
#40836=CARTESIAN_POINT('Ctrl Pts',(4.02381850927322,0.500885556761892,3.63564106712445));
#40837=CARTESIAN_POINT('Ctrl Pts',(4.04767642730465,0.614236921112272,3.92019793948569));
#40838=CARTESIAN_POINT('Ctrl Pts',(4.07153434533605,0.577368897990231,4.22425593648149));
#40839=CARTESIAN_POINT('Ctrl Pts',(4.09539226336749,0.399329932212592,4.47348393104611));
#40840=CARTESIAN_POINT('Ctrl Pts',(4.11925018139889,0.123637843932736,4.60692867011962));
#40841=CARTESIAN_POINT('Ctrl Pts',(4.14310809943032,-0.182283847264271,
4.59196468982869));
#40842=CARTESIAN_POINT('Ctrl Pts',(4.16696601746173,-0.443633876576525,
4.43224822622665));
#40843=CARTESIAN_POINT('Ctrl Pts',(4.19082393549315,-0.596502436238336,
4.16683582239239));
#40844=CARTESIAN_POINT('Ctrl Pts',(4.21468185352458,-0.603510379797736,
3.86062723727387));
#40845=CARTESIAN_POINT('Ctrl Pts',(4.23853977155598,-0.462943343075553,
3.58849923641164));
#40846=CARTESIAN_POINT('Ctrl Pts',(4.26239768958742,-0.209174182705692,
3.41699430327496));
#40847=CARTESIAN_POINT('Ctrl Pts',(4.28625560761882,0.0957438341235747,
3.38805018506757));
#40848=CARTESIAN_POINT('Ctrl Pts',(4.31011352565025,0.377249837899377,3.50874444390425));
#40849=CARTESIAN_POINT('Ctrl Pts',(4.33397144368167,0.566508000142931,3.7495640793295));
#40850=CARTESIAN_POINT('Ctrl Pts',(4.35782936171309,0.617239514437223,4.05162211295782));
#40851=CARTESIAN_POINT('Ctrl Pts',(4.3816872797445,0.517039159770137,4.34105713706075));
#40852=CARTESIAN_POINT('Ctrl Pts',(4.40554519777592,0.290408643717306,4.54709439922074));
#40853=CARTESIAN_POINT('Ctrl Pts',(4.42940311580735,-0.00723469473045889,
4.61935217913086));
#40854=CARTESIAN_POINT('Ctrl Pts',(4.45326103383876,-0.303108954077165,
4.54016147994594));
#40855=CARTESIAN_POINT('Ctrl Pts',(4.47711895187019,-0.524864817190473,
4.3288865854667));
#40856=CARTESIAN_POINT('Ctrl Pts',(4.5009768699016,-0.618276935702851,4.03718996201469));
#40857=CARTESIAN_POINT('Ctrl Pts',(4.52483478793302,-0.560503501787052,
3.7363993798876));
#40858=CARTESIAN_POINT('Ctrl Pts',(4.54869270596444,-0.365671693940747,
3.50006632967672));
#40859=CARTESIAN_POINT('Ctrl Pts',(4.57255062399586,-0.0814231961944085,
3.38598067979976));
#40860=CARTESIAN_POINT('Ctrl Pts',(4.59640854202727,0.222735490926488,3.42203947925158));
#40861=CARTESIAN_POINT('Ctrl Pts',(4.6202664600587,0.472429283332598,3.59942536936051));
#40862=CARTESIAN_POINT('Ctrl Pts',(4.64412437809011,0.606601247243452,3.87476266809168));
#40863=CARTESIAN_POINT('Ctrl Pts',(4.66798229612153,0.592442682719785,4.18072390587243));
#40864=CARTESIAN_POINT('Ctrl Pts',(4.69184021415295,0.433415744455024,4.44249322584619));
#40865=CARTESIAN_POINT('Ctrl Pts',(4.71569813218437,0.168406850663934,4.59606089882753));
#40866=CARTESIAN_POINT('Ctrl Pts',(4.7395560502158,-0.1377821054254,4.60387544567241));
#40867=CARTESIAN_POINT('Ctrl Pts',(4.7634139682472,-0.410279583628813,4.46402599681362));
#40868=CARTESIAN_POINT('Ctrl Pts',(4.78727188627863,-0.582452527843622,
4.21070955191949));
#40869=CARTESIAN_POINT('Ctrl Pts',(4.81112980431005,-0.612199963312297,
3.9058688819681));
#40870=CARTESIAN_POINT('Ctrl Pts',(4.83498772234147,-0.492247831758966,
3.62404583445569));
#40871=CARTESIAN_POINT('Ctrl Pts',(4.85884564037289,-0.251927696778831,
3.4341538212047));
#40872=CARTESIAN_POINT('Ctrl Pts',(4.88270355840431,0.0499956224363984,
3.38262661200963));
#40873=CARTESIAN_POINT('Ctrl Pts',(4.90656147643572,0.339693650112522,3.48206401309162));
#40874=CARTESIAN_POINT('Ctrl Pts',(4.93041939446714,0.546327327266884,3.70815087126575));
#40875=CARTESIAN_POINT('Ctrl Pts',(4.95427731249857,0.619369091246891,4.00560279122603));
#40876=CARTESIAN_POINT('Ctrl Pts',(4.97813523052998,0.540958241141728,4.3016846761146));
#40877=CARTESIAN_POINT('Ctrl Pts',(5.00199314856141,0.330268365670778,4.52399643996756));
#40878=CARTESIAN_POINT('Ctrl Pts',(5.02585106659282,0.0388188784636707,
4.61817680087201));
#40879=CARTESIAN_POINT('Ctrl Pts',(5.04970898462424,-0.262122881932824,
4.56119609516527));
#40880=CARTESIAN_POINT('Ctrl Pts',(5.07356690265566,-0.498968457612796,
4.36698765751594));
#40881=CARTESIAN_POINT('Ctrl Pts',(5.09742482068708,-0.613802653778546,
4.08304074106085));
#40882=CARTESIAN_POINT('Ctrl Pts',(5.12128273871849,-0.578545381446849,
3.77878810143205));
#40883=CARTESIAN_POINT('Ctrl Pts',(5.14514065674992,-0.40181800409162,3.52862779669421));
#40884=CARTESIAN_POINT('Ctrl Pts',(5.16899857478133,-0.126835179433317,
3.39373083558568));
#40885=CARTESIAN_POINT('Ctrl Pts',(5.19285649281276,0.179162301517353,3.4070831996169));
#40886=CARTESIAN_POINT('Ctrl Pts',(5.21671441084417,0.441349719463922,3.56541987207117));
#40887=CARTESIAN_POINT('Ctrl Pts',(5.24057232887559,0.595615108876583,3.83002322352904));
#40888=CARTESIAN_POINT('Ctrl Pts',(5.26443024690701,0.604236379939102,4.13619052690848));
#40889=CARTESIAN_POINT('Ctrl Pts',(5.28828816493843,0.465105397037983,4.40905553670335));
#40890=CARTESIAN_POINT('Ctrl Pts',(5.31214608296985,0.21224347534444,4.58189532532512));
#40891=CARTESIAN_POINT('Ctrl Pts',(5.33600400100126,-0.0925177574670201,
4.61244585639451));
#40892=CARTESIAN_POINT('Ctrl Pts',(5.35986191903269,-0.37465587844466,4.49323669288525));
#40893=CARTESIAN_POINT('Ctrl Pts',(5.3837198370641,-0.565180431721392,4.25341772246777));
#40894=CARTESIAN_POINT('Ctrl Pts',(5.40757775509553,-0.617502974236318,
3.95163121594683));
#40895=CARTESIAN_POINT('Ctrl Pts',(5.43143567312694,-0.518829219107294,
3.66167219466597));
#40896=CARTESIAN_POINT('Ctrl Pts',(5.45529359115837,-0.293287587282116,
3.45444353765392));
#40897=CARTESIAN_POINT('Ctrl Pts',(5.47915150918978,0.00397084862654925,
3.38061829634467));
#40898=CARTESIAN_POINT('Ctrl Pts',(5.50300942722121,0.300258303883157,3.45824875319892));
#40899=CARTESIAN_POINT('Ctrl Pts',(5.52686734525262,0.523124424966688,3.66835214690199));
#40900=CARTESIAN_POINT('Ctrl Pts',(5.55072526328404,0.618072374525773,3.95955247459688));
#40901=CARTESIAN_POINT('Ctrl Pts',(5.57458318131546,0.561884792553919,4.26064332401524));
#40902=CARTESIAN_POINT('Ctrl Pts',(5.59844109934688,0.368301073379394,4.49799978094171));
#40903=CARTESIAN_POINT('Ctrl Pts',(5.62229901737829,0.0846577094226282,
4.61358172616469));
#40904=CARTESIAN_POINT('Ctrl Pts',(5.64615693540972,-0.219686770477705,
4.57912622575047));
#40905=CARTESIAN_POINT('Ctrl Pts',(5.67001485344113,-0.470311850924231,
4.40305858798173));
#40906=CARTESIAN_POINT('Ctrl Pts',(5.69387277147256,-0.605932872639677,
4.12843214650112));
#40907=CARTESIAN_POINT('Ctrl Pts',(5.71773068950397,-0.593386801983745,
3.82240054650545));
#40908=CARTESIAN_POINT('Ctrl Pts',(5.74158860753539,-0.435741494202748,
3.55979685111874));
#40909=CARTESIAN_POINT('Ctrl Pts',(5.76544652556682,-0.171545522688555,
3.40483481554927));
#40910=CARTESIAN_POINT('Ctrl Pts',(5.78930444359822,0.134598003740687,3.39540688139736));
#40911=CARTESIAN_POINT('Ctrl Pts',(5.81316236162965,0.407828648458881,3.53381843004554));
#40912=CARTESIAN_POINT('Ctrl Pts',(5.83702027966106,0.58133408605803,3.78622407765735));
#40913=CARTESIAN_POINT('Ctrl Pts',(5.86087819769249,0.612687492198482,4.09090374899912));
#40914=CARTESIAN_POINT('Ctrl Pts',(5.8847361157239,0.494222140250734,4.3733550009975));
#40915=CARTESIAN_POINT('Ctrl Pts',(5.90859403375532,0.254905969192102,4.56451074097759));
#40916=CARTESIAN_POINT('Ctrl Pts',(5.93245195178675,-0.0467415727364197,
4.61762831145024));
#40917=CARTESIAN_POINT('Ctrl Pts',(5.95630986981815,-0.336959681931401,
4.51971877801409));
#40918=CARTESIAN_POINT('Ctrl Pts',(5.98016778784959,-0.544781677596122,
4.29472414464893));
#40919=CARTESIAN_POINT('Ctrl Pts',(6.00402570588099,-0.61939026621187,3.99766086682344));
#40920=CARTESIAN_POINT('Ctrl Pts',(6.02788362391242,-0.542540019317823,
3.70117063377655));
#40921=CARTESIAN_POINT('Ctrl Pts',(6.05174154194384,-0.333025929677459,
3.47775031355921));
#40922=CARTESIAN_POINT('Ctrl Pts',(6.07559945997526,-0.042074208138152,
3.38203805739984));
#40923=CARTESIAN_POINT('Ctrl Pts',(6.09945737800668,0.259158778028439,3.43742717299816));
#40924=CARTESIAN_POINT('Ctrl Pts',(6.12331529603809,0.497033648893269,3.63039418124561));
#40925=CARTESIAN_POINT('Ctrl Pts',(6.14717321406952,0.613345206175343,3.91371436613889));
#40926=CARTESIAN_POINT('Ctrl Pts',(6.17103113210093,0.579724447951105,4.21818191418763));
#40927=CARTESIAN_POINT('Ctrl Pts',(6.19488905013236,0.40425597056565,4.46920707734689));
#40928=CARTESIAN_POINT('Ctrl Pts',(6.21874696816377,0.13010450107023,4.60567007851858));
#40929=CARTESIAN_POINT('Ctrl Pts',(6.24260488619519,-0.176179318911185,
4.59370602015056));
#40930=CARTESIAN_POINT('Ctrl Pts',(6.26646280422661,-0.438782409775579,
4.43717629804221));
#40931=CARTESIAN_POINT('Ctrl Pts',(6.29032072225803,-0.595217424383659,
4.17259489198797));
#40932=CARTESIAN_POINT('Ctrl Pts',(6.31417864028945,-0.604035436411749,
3.86794272465182));
#40933=CARTESIAN_POINT('Ctrl Pts',(6.34598919766468,-0.423477061217623,
3.4998212904071));
#40934=CARTESIAN_POINT('Ctrl Pts',(6.3857523943837,0.100470573235224,3.30464850830547));
#40935=CARTESIAN_POINT('Ctrl Pts',(6.43346823044655,0.640013163212275,3.70919899990029));
#40936=CARTESIAN_POINT('Ctrl Pts',(6.48118406650937,0.590335835129396,4.3806576914582));
#40937=CARTESIAN_POINT('Ctrl Pts',(6.52889990257223,-0.000686065451295705,
4.70262946694599));
#40938=CARTESIAN_POINT('Ctrl Pts',(6.57661573863505,-0.591483599613884,
4.37932465573422));
#40939=CARTESIAN_POINT('Ctrl Pts',(6.6243315746979,-0.638898060441451,3.70770201230499));
#40940=CARTESIAN_POINT('Ctrl Pts',(6.67204741076074,-0.0997162142428727,
3.30448953810453));
#40941=CARTESIAN_POINT('Ctrl Pts',(6.71976324682356,0.531096731682035,3.53998115137447));
#40942=CARTESIAN_POINT('Ctrl Pts',(6.76747908288643,0.674163513320998,4.19791190586338));
#40943=CARTESIAN_POINT('Ctrl Pts',(6.81519491894923,0.19815244237474,4.67409883091767));
#40944=CARTESIAN_POINT('Ctrl Pts',(6.86291075501209,-0.459834002450772,
4.53124951681343));
#40945=CARTESIAN_POINT('Ctrl Pts',(6.91062659107492,-0.695543074258338,
3.90054607923755));
#40946=CARTESIAN_POINT('Ctrl Pts',(6.95834242713776,-0.292526745343327,
3.36117245204842));
#40947=CARTESIAN_POINT('Ctrl Pts',(7.00605826320061,0.379122722467859,3.40844412700009));
#40948=CARTESIAN_POINT('Ctrl Pts',(7.05377409926343,0.702617257610868,3.99895059076549));
#40949=CARTESIAN_POINT('Ctrl Pts',(7.10148993532628,0.380887926283931,4.59042078110798));
#40950=CARTESIAN_POINT('Ctrl Pts',(7.14920577138911,-0.290616845661789,
4.63969846327979));
#40951=CARTESIAN_POINT('Ctrl Pts',(7.19692160745196,-0.695243592084394,
4.10153121423426));
#40952=CARTESIAN_POINT('Ctrl Pts',(7.24463744351478,-0.461417505508394,
3.47012628326466));
#40953=CARTESIAN_POINT('Ctrl Pts',(7.29235327957764,0.196135405489393,3.32531254251214));
#40954=CARTESIAN_POINT('Ctrl Pts',(7.34006911564046,0.673574140181709,3.80007467379138));
#40955=CARTESIAN_POINT('Ctrl Pts',(7.38778495170331,0.532459385890787,4.45843130921146));
#40956=CARTESIAN_POINT('Ctrl Pts',(7.43550078776614,-0.0976210197556089,
4.69580341906706));
#40957=CARTESIAN_POINT('Ctrl Pts',(7.48321662382899,-0.638054538563543,
4.29420854311633));
#40958=CARTESIAN_POINT('Ctrl Pts',(7.53093245989182,-0.592552758097988,
3.62243743491725));
#40959=CARTESIAN_POINT('Ctrl Pts',(7.57864829595465,-0.00290066162856385,
3.29738783984629));
#40960=CARTESIAN_POINT('Ctrl Pts',(7.6263641320175,0.589415156704478,3.61755780248734));
#40961=CARTESIAN_POINT('Ctrl Pts',(7.67407996808033,0.64046196749915,4.28893031975233));
#40962=CARTESIAN_POINT('Ctrl Pts',(7.72179580414318,0.103362698669259,4.69497367861456));
#40963=CARTESIAN_POINT('Ctrl Pts',(7.769511640206,-0.528656126737314,4.46281201486565));
#40964=CARTESIAN_POINT('Ctrl Pts',(7.81722747626886,-0.675201896567852,
3.80564295658466));
#40965=CARTESIAN_POINT('Ctrl Pts',(7.86494331233168,-0.201699375449268,
3.32695496184095));
#40966=CARTESIAN_POINT('Ctrl Pts',(7.91265914839452,0.457026785680635,3.46633458176699));
#40967=CARTESIAN_POINT('Ctrl Pts',(7.96037498445737,0.696058217263005,4.09578736675475));
#40968=CARTESIAN_POINT('Ctrl Pts',(8.0080908205202,0.295888677698302,4.63727713897333));
#40969=CARTESIAN_POINT('Ctrl Pts',(8.05580665658303,-0.375999987428149,
4.59354550870361));
#40970=CARTESIAN_POINT('Ctrl Pts',(8.10352249264589,-0.702602078596463,
4.00475190491975));
#40971=CARTESIAN_POINT('Ctrl Pts',(8.1512383287087,-0.383993870066737,3.41159455373064));
#40972=CARTESIAN_POINT('Ctrl Pts',(8.19895416477156,0.287241817850264,3.35877897763223));
#40973=CARTESIAN_POINT('Ctrl Pts',(8.24667000083438,0.694698924651979,3.89480653282778));
#40974=CARTESIAN_POINT('Ctrl Pts',(8.29438583689724,0.464203319628796,4.52743486753713));
#40975=CARTESIAN_POINT('Ctrl Pts',(8.34210167296006,-0.192577336495663,
4.67571164775853));
#40976=CARTESIAN_POINT('Ctrl Pts',(8.3898175090229,-0.672511261332963,4.20347202468314));
#40977=CARTESIAN_POINT('Ctrl Pts',(8.43753334508575,-0.534867746972347,
3.54438091052171));
#40978=CARTESIAN_POINT('Ctrl Pts',(8.48524918114857,0.0939530494311211,
3.303691816829));
#40979=CARTESIAN_POINT('Ctrl Pts',(8.53296501721143,0.636495314888509,3.70243324182078));
#40980=CARTESIAN_POINT('Ctrl Pts',(8.58068085327425,0.594534138944492,4.37443479950165));
#40981=CARTESIAN_POINT('Ctrl Pts',(8.6283966893371,0.00660311512414562,
4.7025871193802));
#40982=CARTESIAN_POINT('Ctrl Pts',(8.67611252539993,-0.58739165091669,4.3855428768395));
#40983=CARTESIAN_POINT('Ctrl Pts',(8.72382836146277,-0.64197562573843,3.71444867815739));
#40984=CARTESIAN_POINT('Ctrl Pts',(8.77154419752561,-0.107023505379864,
3.30558065209521));
#40985=CARTESIAN_POINT('Ctrl Pts',(8.81926003358845,0.526209946737336,3.53440859822909));
#40986=CARTESIAN_POINT('Ctrl Pts',(8.86697586965128,0.676216707984864,4.19079629265377));
#40987=CARTESIAN_POINT('Ctrl Pts',(8.91469170571413,0.20524326135842,4.67197281575615));
#40988=CARTESIAN_POINT('Ctrl Pts',(8.96240754177695,-0.45420823024697,4.53606636251889));
#40989=CARTESIAN_POINT('Ctrl Pts',(9.0101233778398,-0.69655331512461,3.90788192013928));
#40990=CARTESIAN_POINT('Ctrl Pts',(9.05783921390263,-0.299242772872918,
3.36429092791464));
#40991=CARTESIAN_POINT('Ctrl Pts',(9.10555504996548,0.37286701214988,3.40448135822736));
#40992=CARTESIAN_POINT('Ctrl Pts',(9.15327088602831,0.702567282619003,3.99154572051203));
#40993=CARTESIAN_POINT('Ctrl Pts',(9.20098672209116,0.387089207071907,4.58637377773631));
#40994=CARTESIAN_POINT('Ctrl Pts',(9.24870255815397,-0.28385884346236,4.64272577234503));
#40995=CARTESIAN_POINT('Ctrl Pts',(9.29641839421684,-0.694134950315416,
4.10885280060212));
#40996=CARTESIAN_POINT('Ctrl Pts',(9.34413423027966,-0.46697625165475,3.47501862715065));
#40997=CARTESIAN_POINT('Ctrl Pts',(9.39185006634251,0.189013924253689,3.32328292626348));
#40998=CARTESIAN_POINT('Ctrl Pts',(9.43956590240535,0.671429705166911,3.79298692681914));
#40999=CARTESIAN_POINT('Ctrl Pts',(9.48728173846818,0.537261256551386,4.45279421778236));
#41000=CARTESIAN_POINT('Ctrl Pts',(9.53499757453101,-0.090282470782305,
4.69679361142145));
#41001=CARTESIAN_POINT('Ctrl Pts',(9.58271341059386,-0.634918416022234,
4.30091671014441));
#41002=CARTESIAN_POINT('Ctrl Pts',(9.63042924665669,-0.596499010353368,
3.62870336374299));
#41003=CARTESIAN_POINT('Ctrl Pts',(9.67814508271953,-0.0103053851599677,
3.29745743154951));
#41004=CARTESIAN_POINT('Ctrl Pts',(9.72586091878236,0.585351833794561,3.61136714997101));
#41005=CARTESIAN_POINT('Ctrl Pts',(9.77357675484522,0.643471456979869,4.28216439445919));
#41006=CARTESIAN_POINT('Ctrl Pts',(9.82129259090803,0.110681340139534,4.69384573385819));
#41007=CARTESIAN_POINT('Ctrl Pts',(9.8690084269709,-0.523749154402255,4.46835785966634));
#41008=CARTESIAN_POINT('Ctrl Pts',(9.91672426303372,-0.677212741539845,
3.81276975633088));
#41009=CARTESIAN_POINT('Ctrl Pts',(9.96444009909655,-0.208781447863971,
3.32911806666439));
#41010=CARTESIAN_POINT('Ctrl Pts',(10.0121559351594,0.451377061900895,3.4615475792254));
#41011=CARTESIAN_POINT('Ctrl Pts',(10.0598717712222,0.697029070393332,4.08844623493918));
#41012=CARTESIAN_POINT('Ctrl Pts',(10.1075876072851,0.302588558372737,4.63412335218805));
#41013=CARTESIAN_POINT('Ctrl Pts',(10.1553034433479,-0.369723682724971,
4.5974752378807));
#41014=CARTESIAN_POINT('Ctrl Pts',(10.2030192794108,-0.702512977046242,
4.01215641928927));
#41015=CARTESIAN_POINT('Ctrl Pts',(10.2507351154736,-0.390173794994359,
3.41567417381395));
#41016=CARTESIAN_POINT('Ctrl Pts',(10.2984509515364,0.280467986596366,3.3557873255338));
#41017=CARTESIAN_POINT('Ctrl Pts',(10.3461667875993,0.693551700540965,3.8874908887021));
#41018=CARTESIAN_POINT('Ctrl Pts',(10.3938826236621,0.469736216214169,4.52251329995044));
#41019=CARTESIAN_POINT('Ctrl Pts',(10.441598459725,-0.185445263282835,4.67770370795377));
#41020=CARTESIAN_POINT('Ctrl Pts',(10.4893142957878,-0.670329504065059,
4.21054837313121));
#41021=CARTESIAN_POINT('Ctrl Pts',(10.5370301318506,-0.539639846919137,
3.55004322755915));
#41022=CARTESIAN_POINT('Ctrl Pts',(10.5847459679134,0.0866093850789692,
3.30274030959437));
#41023=CARTESIAN_POINT('Ctrl Pts',(10.6324618039763,0.633323886102378,3.69574169404847));
#41024=CARTESIAN_POINT('Ctrl Pts',(10.6801776400391,0.598447317577389,4.36814816247366));
#41025=CARTESIAN_POINT('Ctrl Pts',(10.727893476102,0.0140073690254923,4.70247850861168));
#41026=CARTESIAN_POINT('Ctrl Pts',(10.7756093121648,-0.583295762033595,
4.39171203127037));
#41027=CARTESIAN_POINT('Ctrl Pts',(10.8233251482277,-0.644949419658282,
3.72123036834915));
#41028=CARTESIAN_POINT('Ctrl Pts',(10.8710409842905,-0.114336101388361,
3.30674714759503));
#41029=CARTESIAN_POINT('Ctrl Pts',(10.9187568203533,0.521273818073547,3.52888868827067));
#41030=CARTESIAN_POINT('Ctrl Pts',(10.9664726564162,0.678189969569843,4.18365899548663));
#41031=CARTESIAN_POINT('Ctrl Pts',(11.014188492479,0.212313836716152,4.66977242119035));
#41032=CARTESIAN_POINT('Ctrl Pts',(11.0619043285418,-0.44853335926228,4.54082352674158));
#41033=CARTESIAN_POINT('Ctrl Pts',(11.1096201646047,-0.697485469857315,
3.91522806604643));
#41034=CARTESIAN_POINT('Ctrl Pts',(11.1573360006675,-0.305925941288932,
3.36747997668469));
#41035=CARTESIAN_POINT('Ctrl Pts',(11.2050518367303,0.36657008644075,3.40058475730499));
#41036=CARTESIAN_POINT('Ctrl Pts',(11.2527676727932,0.702439163386103,3.98414177848112));
#41037=CARTESIAN_POINT('Ctrl Pts',(11.300483508856,0.393247548178179,4.58226164848818));
#41038=CARTESIAN_POINT('Ctrl Pts',(11.3481993449189,-0.277069341413063,
4.64568168744144));
#41039=CARTESIAN_POINT('Ctrl Pts',(11.3959151809817,-0.692949191524882,
4.11616229772746));
#41040=CARTESIAN_POINT('Ctrl Pts',(11.4436310170446,-0.47248313666557,3.47996928262364));
#41041=CARTESIAN_POINT('Ctrl Pts',(11.4913468531074,0.181871452681271,3.32132847698764));
#41042=CARTESIAN_POINT('Ctrl Pts',(11.5390626891702,0.669210688578896,3.78592217363756));
#41043=CARTESIAN_POINT('Ctrl Pts',(11.586778525233,0.54200345202451,4.44710683224685));
#41044=CARTESIAN_POINT('Ctrl Pts',(11.6344943612959,-0.082933894319074,
4.69770640718098));
#41045=CARTESIAN_POINT('Ctrl Pts',(11.6822101973587,-0.631711769407458,
4.30759145280778));
#41046=CARTESIAN_POINT('Ctrl Pts',(11.7299260334216,-0.600379006513997,
3.63501053441836));
#41047=CARTESIAN_POINT('Ctrl Pts',(11.7776418694844,-0.0177089639202829,
3.29760505835735));
#41048=CARTESIAN_POINT('Ctrl Pts',(11.8253577055473,0.581223492728864,3.60521966494218));
#41049=CARTESIAN_POINT('Ctrl Pts',(11.8730735416101,0.646409472732109,4.27536712768685));
#41050=CARTESIAN_POINT('Ctrl Pts',(11.9207893776729,0.11798768763725,4.69264072000881));
#41051=CARTESIAN_POINT('Ctrl Pts',(11.9685052137358,-0.518784006488825,
4.4738516814993));
#41052=CARTESIAN_POINT('Ctrl Pts',(12.0162210497986,-0.679148364938221,
3.81991735272367));
#41053=CARTESIAN_POINT('Ctrl Pts',(12.0639368858614,-0.215840329824027,
3.33135568986959));
#41054=CARTESIAN_POINT('Ctrl Pts',(12.1116527219243,0.445677201297934,3.45682038542343));
#41055=CARTESIAN_POINT('Ctrl Pts',(12.1593685579871,0.697922500842799,4.08109527893561));
#41056=CARTESIAN_POINT('Ctrl Pts',(12.2070843940499,0.309254828945687,4.63089912998995));
#41057=CARTESIAN_POINT('Ctrl Pts',(12.2548002301128,-0.36340631086944,4.60133860234362));
#41058=CARTESIAN_POINT('Ctrl Pts',(12.3025160661756,-0.702345843688318,
4.0195595833814));
#41059=CARTESIAN_POINT('Ctrl Pts',(12.3502319022385,-0.396310381268302,
3.41981869803717));
#41060=CARTESIAN_POINT('Ctrl Pts',(12.3979477383013,0.273663002289436,3.35286722952223));
#41061=CARTESIAN_POINT('Ctrl Pts',(12.4456635743641,0.69232743999824,3.88018774155459));
#41062=CARTESIAN_POINT('Ctrl Pts',(12.493379410427,0.475216936729713,4.51753369406595));
#41063=CARTESIAN_POINT('Ctrl Pts',(12.5410952464898,-0.178292591690169,
4.67962049203707));
#41064=CARTESIAN_POINT('Ctrl Pts',(12.5888110825527,-0.66807328977682,4.21760133486514));
#41065=CARTESIAN_POINT('Ctrl Pts',(12.6365269186155,-0.544352006232531,
3.55575552365962));
#41066=CARTESIAN_POINT('Ctrl Pts',(12.6842427546784,0.0792561005673328,
3.3018662506574));
#41067=CARTESIAN_POINT('Ctrl Pts',(12.7319585907411,0.630082110704352,3.68908394184497));
#41068=CARTESIAN_POINT('Ctrl Pts',(12.779674426804,0.60229402352211,4.36182063329482));
#41069=CARTESIAN_POINT('Ctrl Pts',(12.8273902628668,0.0214100670547408,
4.70229186986395));
#41070=CARTESIAN_POINT('Ctrl Pts',(12.8751060989297,-0.579135083425219,
4.39783767618763));
#41071=CARTESIAN_POINT('Ctrl Pts',(12.9228219349925,-0.647851575657132,
3.7280430229487));
#41072=CARTESIAN_POINT('Ctrl Pts',(12.9705377710554,-0.121635997485283,
3.30799064633195));
#41073=CARTESIAN_POINT('Ctrl Pts',(13.0182536071182,0.516279788787698,3.52342110712114));
#41074=CARTESIAN_POINT('Ctrl Pts',(13.065969443181,0.68008790103128,4.17650129834983));
#41075=CARTESIAN_POINT('Ctrl Pts',(13.1136852792439,0.219360829260397,4.66749763148232));
#41076=CARTESIAN_POINT('Ctrl Pts',(13.1614011153067,-0.44280866732052,4.54552061885334));
#41077=CARTESIAN_POINT('Ctrl Pts',(13.2091169513696,-0.698340151213866,
3.92258362801769));
#41078=CARTESIAN_POINT('Ctrl Pts',(13.2568327874324,-0.31257512890311,3.37073928277739));
#41079=CARTESIAN_POINT('Ctrl Pts',(13.3045486234952,0.36023244386594,3.39675473658331));
#41080=CARTESIAN_POINT('Ctrl Pts',(13.3522644595581,0.702233020544282,3.97673959790624));
#41081=CARTESIAN_POINT('Ctrl Pts',(13.3999802956209,0.39936220921291,4.57808484437918));
#41082=CARTESIAN_POINT('Ctrl Pts',(13.4476961316837,-0.270249063816132,
4.64856588328003));
#41083=CARTESIAN_POINT('Ctrl Pts',(13.4954119677466,-0.691686463226468,
4.123458892096));
#41084=CARTESIAN_POINT('Ctrl Pts',(13.5431278038094,-0.47793754049168,3.48497770064095));
#41085=CARTESIAN_POINT('Ctrl Pts',(13.5908436398723,0.174708779690948,3.31944941132403));
#41086=CARTESIAN_POINT('Ctrl Pts',(13.6385594759351,0.666917339243262,3.77888119920505));
#41087=CARTESIAN_POINT('Ctrl Pts',(13.6862753119979,0.54668544432619,4.44136978420615));
#41088=CARTESIAN_POINT('Ctrl Pts',(13.7339911480608,-0.075576105952426,
4.69854170502367));
#41089=CARTESIAN_POINT('Ctrl Pts',(13.7817069841236,-0.62843495524706,4.31423202967224));
#41090=CARTESIAN_POINT('Ctrl Pts',(13.8294228201864,-0.604192315423611,
3.64135824639153));
#41091=CARTESIAN_POINT('Ctrl Pts',(13.8771386562493,-0.025110575652917,
3.29783070386218));
#41092=CARTESIAN_POINT('Ctrl Pts',(13.9248544923121,0.577030592115723,3.59911603023956));
#41093=CARTESIAN_POINT('Ctrl Pts',(13.972570328375,0.649275688387581,4.26853927444071));
#41094=CARTESIAN_POINT('Ctrl Pts',(14.0202861644378,0.125280929622514,4.69135877091509));
#41095=CARTESIAN_POINT('Ctrl Pts',(14.0680020005006,-0.513761234509794,
4.47929287013608));
#41096=CARTESIAN_POINT('Ctrl Pts',(14.1157178365635,-0.681008551759042,
3.82708495184235));
#41097=CARTESIAN_POINT('Ctrl Pts',(14.1634336726263,-0.222875237264486,
3.33366758291179));
#41098=CARTESIAN_POINT('Ctrl Pts',(14.2111495086891,0.439927836986373,3.45215352543546));
#41099=CARTESIAN_POINT('Ctrl Pts',(14.258865344752,0.698738409372782,4.07373531525328));
#41100=CARTESIAN_POINT('Ctrl Pts',(14.3065811808148,0.315886748959774,4.62760483051036));
#41101=CARTESIAN_POINT('Ctrl Pts',(14.3542970168777,-0.357048573565392,
4.60513517296818));
#41102=CARTESIAN_POINT('Ctrl Pts',(14.4020128529405,-0.702100697086982,
4.02696057488784));
#41103=CARTESIAN_POINT('Ctrl Pts',(14.4497286890033,-0.402402947265751,
3.42402766604624));
#41104=CARTESIAN_POINT('Ctrl Pts',(14.4974445250662,0.266827620794843,3.35001901394789));
#41105=CARTESIAN_POINT('Ctrl Pts',(14.545160361129,0.691026279008849,3.87289790258421));
#41106=CARTESIAN_POINT('Ctrl Pts',(14.5928761971919,0.480644872403009,4.51249660299459));
#41107=CARTESIAN_POINT('Ctrl Pts',(14.6405920332547,-0.171120116202498,
4.6814617871012));
#41108=CARTESIAN_POINT('Ctrl Pts',(14.6883078693176,-0.665742869077823,
4.22463012647536));
#41109=CARTESIAN_POINT('Ctrl Pts',(14.7360237053803,-0.549003701508229,
3.56151716432844));
#41110=CARTESIAN_POINT('Ctrl Pts',(14.7837395414432,0.0718940126641393,
3.30106973710437));
#41111=CARTESIAN_POINT('Ctrl Pts',(14.831455377506,0.626770348775451,3.68246072472179));
#41112=CARTESIAN_POINT('Ctrl Pts',(14.8791712135689,0.606073829504824,4.35545291479698));
#41113=CARTESIAN_POINT('Ctrl Pts',(14.9268870496317,0.0288103869553486,
4.70202722386799));
#41114=CARTESIAN_POINT('Ctrl Pts',(14.9746028856946,-0.574910077240004,
4.4039191311837));
#41115=CARTESIAN_POINT('Ctrl Pts',(15.0223187217574,-0.650681771377263,
3.73488588523872));
#41116=CARTESIAN_POINT('Ctrl Pts',(15.0700345578202,-0.128922382832804,
3.30931101018402));
#41117=CARTESIAN_POINT('Ctrl Pts',(15.1177503938831,0.511228413592865,3.51800646209349));
#41118=CARTESIAN_POINT('Ctrl Pts',(15.1654662299459,0.681910291555949,4.16932399628639));
#41119=CARTESIAN_POINT('Ctrl Pts',(15.2131820660088,0.226383456244684,4.6651486993049));
#41120=CARTESIAN_POINT('Ctrl Pts',(15.2608979020716,-0.437034790293287,
4.55015711712348));
#41121=CARTESIAN_POINT('Ctrl Pts',(15.3086137381344,-0.699117264260319,
3.92994778903219));
#41122=CARTESIAN_POINT('Ctrl Pts',(15.3563295741972,-0.319189597155267,
3.37406848416447));
#41123=CARTESIAN_POINT('Ctrl Pts',(15.4040454102601,0.353854788380711,3.39299172148285));
#41124=CARTESIAN_POINT('Ctrl Pts',(15.4517612463229,0.70194887699091,3.96934000098645));
#41125=CARTESIAN_POINT('Ctrl Pts',(15.4994770823858,0.40543251098856,4.57384382934891));
#41126=CARTESIAN_POINT('Ctrl Pts',(15.5471929184486,-0.263398768235635,
4.65137803949801));
#41127=CARTESIAN_POINT('Ctrl Pts',(15.5949087545115,-0.690346905678043,
4.13074177323664));
#41128=CARTESIAN_POINT('Ctrl Pts',(15.6426245905743,-0.483338857283784,
3.4900433248913));
#41129=CARTESIAN_POINT('Ctrl Pts',(15.6903404266371,0.167526700878456,3.31764593799033));
#41130=CARTESIAN_POINT('Ctrl Pts',(15.7380562627,0.664549911894371,3.77186478559966));
#41131=CARTESIAN_POINT('Ctrl Pts',(15.7857720987628,0.551306713402943,4.43558371090429));
#41132=CARTESIAN_POINT('Ctrl Pts',(15.8334879348256,-0.0682099229505586,
4.69929941216862));
#41133=CARTESIAN_POINT('Ctrl Pts',(15.8812037708885,-0.625088337514006,
4.32083770313399));
#41134=CARTESIAN_POINT('Ctrl Pts',(15.9289196069513,-0.607938513517956,
3.64774579458877));
#41135=CARTESIAN_POINT('Ctrl Pts',(15.9766354430142,-0.0325093982219456,
3.29813434300035));
#41136=CARTESIAN_POINT('Ctrl Pts',(16.024351279077,0.572773597682653,3.59305692382598));
#41137=CARTESIAN_POINT('Ctrl Pts',(16.0720671151399,0.652069785580651,4.2616815931263));
#41138=CARTESIAN_POINT('Ctrl Pts',(16.1197829512026,0.132560255996602,4.69000002896988));
#41139=CARTESIAN_POINT('Ctrl Pts',(16.1674987872655,-0.508681396370837,
4.48468082119526));
#41140=CARTESIAN_POINT('Ctrl Pts',(16.2152146233283,-0.682793095381579,
3.83427175754402));
#41141=CARTESIAN_POINT('Ctrl Pts',(16.2629304593912,-0.229885388781225,
3.33605348899688));
#41142=CARTESIAN_POINT('Ctrl Pts',(16.310646295454,0.434129607578297,3.44754751763412));
#41143=CARTESIAN_POINT('Ctrl Pts',(16.3583621315168,0.699476705356048,4.06636716140204));
#41144=CARTESIAN_POINT('Ctrl Pts',(16.4060779675797,0.322483581772784,4.62424081966442));
#41145=CARTESIAN_POINT('Ctrl Pts',(16.4537938036425,-0.350651177000141,
4.60886452804932));
#41146=CARTESIAN_POINT('Ctrl Pts',(16.5015096397054,-0.701777564471952,
4.03435857174156));
#41147=CARTESIAN_POINT('Ctrl Pts',(16.5492254757682,-0.408450816253369,
3.42830061032894));
#41148=CARTESIAN_POINT('Ctrl Pts',(16.596941311831,0.259962601354342,3.34724299517707));
#41149=CARTESIAN_POINT('Ctrl Pts',(16.6446571478939,0.689648362099571,3.86562218151166));
#41150=CARTESIAN_POINT('Ctrl Pts',(16.6923729839567,0.486019420324727,4.50740258623259));
#41151=CARTESIAN_POINT('Ctrl Pts',(16.7400888200196,-0.163928633504336,
4.6832273886238));
#41152=CARTESIAN_POINT('Ctrl Pts',(16.7878046560824,-0.663338500820136,
4.23163396723712));
#41153=CARTESIAN_POINT('Ctrl Pts',(16.8355204921452,-0.553594416058007,
3.56732750958986));
#41154=CARTESIAN_POINT('Ctrl Pts',(16.8832363282081,0.064523939115192,3.30035085740826));
#41155=CARTESIAN_POINT('Ctrl Pts',(16.9309521642709,0.623388968170475,3.67587277835446));
#41156=CARTESIAN_POINT('Ctrl Pts',(16.9786680003338,0.609786315682611,4.34904571427615));
#41157=CARTESIAN_POINT('Ctrl Pts',(17.0263838363966,0.0362075067348799,
4.70168460001938));
#41158=CARTESIAN_POINT('Ctrl Pts',(17.0740996724594,-0.570621212771584,
4.40995572075944));
#41159=CARTESIAN_POINT('Ctrl Pts',(17.1218155085223,-0.653439692453966,
3.74175819514654));
#41160=CARTESIAN_POINT('Ctrl Pts',(17.1695313445851,-0.136194448093839,
3.31070809249149));
#41161=CARTESIAN_POINT('Ctrl Pts',(17.2172471806479,0.50612025357182,3.51264535462077));
#41162=CARTESIAN_POINT('Ctrl Pts',(17.2649630167108,0.683656938721366,4.16212788651693));
#41163=CARTESIAN_POINT('Ctrl Pts',(17.3126788527736,0.233380937628925,4.66272588556639));
#41164=CARTESIAN_POINT('Ctrl Pts',(17.3603946888365,-0.431212369515449,
4.55473250655174));
#41165=CARTESIAN_POINT('Ctrl Pts',(17.4081105248993,-0.699816722678643,
3.93731973111387));
#41166=CARTESIAN_POINT('Ctrl Pts',(17.4558263609621,-0.325768611341644,
3.37746721105403));
#41167=CARTESIAN_POINT('Ctrl Pts',(17.503542197025,0.347437828384778,3.38929612998149));
#41168=CARTESIAN_POINT('Ctrl Pts',(17.5512580330878,0.701586764287296,3.96194380963385));
#41169=CARTESIAN_POINT('Ctrl Pts',(17.5989738691507,0.411457779244836,4.56953907446917));
#41170=CARTESIAN_POINT('Ctrl Pts',(17.6466897052135,-0.256519215569882,
4.65411784373439));
#41171=CARTESIAN_POINT('Ctrl Pts',(17.6944055412764,-0.688930667671302,
4.13801013220155));
#41172=CARTESIAN_POINT('Ctrl Pts',(17.7421213773391,-0.488686487089258,
3.49516559270919));
#41173=CARTESIAN_POINT('Ctrl Pts',(17.789837213402,0.160326013994967,3.3159182573078));
#41174=CARTESIAN_POINT('Ctrl Pts',(17.8375530494648,0.662108669494809,3.76487371217125));
#41175=CARTESIAN_POINT('Ctrl Pts',(17.8852688855277,0.555866745946156,4.42974925503083));
#41176=CARTESIAN_POINT('Ctrl Pts',(17.9329847215905,-0.060836163514142,
4.69997944445332));
#41177=CARTESIAN_POINT('Ctrl Pts',(17.9807005576534,-0.621672287934692,
4.32740773946617));
#41178=CARTESIAN_POINT('Ctrl Pts',(18.0284163937162,-0.611617184687133,
3.65417246951162));
#41179=CARTESIAN_POINT('Ctrl Pts',(18.0761322297791,-0.0399046098013318,
3.29851594204507));
#41180=CARTESIAN_POINT('Ctrl Pts',(18.1238480658419,0.568452982276385,3.58704301871817));
#41181=CARTESIAN_POINT('Ctrl Pts',(18.1715639019047,0.65479145395626,4.25479484546229));
#41182=CARTESIAN_POINT('Ctrl Pts',(18.2192797379675,0.139824858206545,4.68856464509573));
#41183=CARTESIAN_POINT('Ctrl Pts',(18.2669955740304,-0.503545056316242,
4.49001493620888));
#41184=CARTESIAN_POINT('Ctrl Pts',(18.3147114100932,-0.684501797587214,
3.84147697155243));
#41185=CARTESIAN_POINT('Ctrl Pts',(18.3624272461561,-0.236870005719869,
3.33851314310973));
#41186=CARTESIAN_POINT('Ctrl Pts',(18.4101430822189,0.42828315711354,3.44300287363294));
#41187=CARTESIAN_POINT('Ctrl Pts',(18.4578589182817,0.70013730678616,4.05899163580144));
#41188=CARTESIAN_POINT('Ctrl Pts',(18.5055747543446,0.32904459463985,4.62080747111051));
#41189=CARTESIAN_POINT('Ctrl Pts',(18.5532905904074,-0.34421483176614,4.61252625334797));
#41190=CARTESIAN_POINT('Ctrl Pts',(18.6010064264702,-0.701376481735239,
4.0417527522082));
#41191=CARTESIAN_POINT('Ctrl Pts',(18.6487222625331,-0.414453316462639,
3.43263705626685));
#41192=CARTESIAN_POINT('Ctrl Pts',(18.6964380985959,0.253068706501803,3.34453948155689));
#41193=CARTESIAN_POINT('Ctrl Pts',(18.7441539346588,0.68819384232267,3.85836138648927));
#41194=CARTESIAN_POINT('Ctrl Pts',(18.7918697707216,0.491339983515996,4.50225220959958));
#41195=CARTESIAN_POINT('Ctrl Pts',(18.8395856067844,-0.156718942392259,
4.68491710048942));
#41196=CARTESIAN_POINT('Ctrl Pts',(18.8873014428473,-0.660860452068119,
4.23861207919858));
#41197=CARTESIAN_POINT('Ctrl Pts',(18.9350172789101,-0.558123639969822,
3.57318591405529));
#41198=CARTESIAN_POINT('Ctrl Pts',(18.9827331149729,0.0571466985584877,
3.29970969142451));
#41199=CARTESIAN_POINT('Ctrl Pts',(19.0304489510358,0.619938344467307,3.66932083449001));
#41200=CARTESIAN_POINT('Ctrl Pts',(19.0781647870986,0.613431069708698,4.3425997434341));
#41201=CARTESIAN_POINT('Ctrl Pts',(19.1258806231615,0.0436006047213211,
4.70126403633668));
#41202=CARTESIAN_POINT('Ctrl Pts',(19.1735964592243,-0.566268966340429,
4.41594677447179));
#41203=CARTESIAN_POINT('Ctrl Pts',(19.2213122952871,-0.656125032675529,
3.74865918919138));
#41204=CARTESIAN_POINT('Ctrl Pts',(19.26902813135,-0.143451385285705,3.31218173833215));
#41205=CARTESIAN_POINT('Ctrl Pts',(19.3167439674128,0.500955875668841,3.50733837970023));
#41206=CARTESIAN_POINT('Ctrl Pts',(19.3644598034757,0.68532764936022,4.15491376927485));
#41207=CARTESIAN_POINT('Ctrl Pts',(19.4121756395385,0.240352494576274,4.66022945763735));
#41208=CARTESIAN_POINT('Ctrl Pts',(19.4598914756013,-0.425342048711971,
4.55924628221868));
#41209=CARTESIAN_POINT('Ctrl Pts',(19.5076073116642,-0.700438454444525,
3.94469862920436));
#41210=CARTESIAN_POINT('Ctrl Pts',(19.555323147727,-0.332311429993836,3.3809350976725));
#41211=CARTESIAN_POINT('Ctrl Pts',(19.6030389837899,0.340982256434611,3.38566835039883));
#41212=CARTESIAN_POINT('Ctrl Pts',(19.6507548198527,0.701146760813864,3.95455188724214));
#41213=CARTESIAN_POINT('Ctrl Pts',(19.6984706559155,0.417437272672218,4.56517097885182));
#41214=CARTESIAN_POINT('Ctrl Pts',(19.7461864919784,-0.249611033919464,
4.6567851409082));
#41215=CARTESIAN_POINT('Ctrl Pts',(19.7939023280412,-0.687438163400574,
4.14526287985386));
#41216=CARTESIAN_POINT('Ctrl Pts',(19.841618164104,-0.493979350866992,3.5003444672369));
#41217=CARTESIAN_POINT('Ctrl Pts',(19.8893340001669,0.153106602982307,3.31426555646693));
#41218=CARTESIAN_POINT('Ctrl Pts',(19.9370498362297,0.659595612567133,3.75791065255607));
#41219=CARTESIAN_POINT('Ctrl Pts',(19.9847656722925,0.560361770063263,4.42386348253578));
#41220=CARTESIAN_POINT('Ctrl Pts',(20.0324815083554,-0.0534494809679074,
4.70058849011268));
#41221=CARTESIAN_POINT('Ctrl Pts',(20.0801973444182,-0.618198828117398,
4.33392863744107));
#41222=CARTESIAN_POINT('Ctrl Pts',(20.1279131804811,-0.615205937201001,
3.66066167313574));
#41223=CARTESIAN_POINT('Ctrl Pts',(20.1756290165439,-0.0473369003220797,
3.29892991724937));
#41224=CARTESIAN_POINT('Ctrl Pts',(20.2233448526068,0.564147630203746,3.58116102158214));
#41225=CARTESIAN_POINT('Ctrl Pts',(20.2710606886696,0.657292163719816,4.24771695100806));
#41226=CARTESIAN_POINT('Ctrl Pts',(20.3187765247324,0.147355317357748,4.68736342730055));
#41227=CARTESIAN_POINT('Ctrl Pts',(20.3664923607953,-0.498896366832293,
4.49468216892218));
#41228=CARTESIAN_POINT('Ctrl Pts',(20.4062555575143,-0.653992183610565,
3.9575054511282));
#41229=CARTESIAN_POINT('Ctrl Pts',(20.4380661148895,-0.465699721472375,
3.59327933193152));
#41230=CARTESIAN_POINT('Ctrl Pts',(20.461924032921,-0.215665100260693,3.41899970433759));
#41231=CARTESIAN_POINT('Ctrl Pts',(20.4857819509523,0.0900520562992202,
3.38718375849312));
#41232=CARTESIAN_POINT('Ctrl Pts',(20.5096398689838,0.372154449079436,3.50499792242313));
#41233=CARTESIAN_POINT('Ctrl Pts',(20.5334977870152,0.564103623124681,3.74397162737493));
#41234=CARTESIAN_POINT('Ctrl Pts',(20.5573557050466,0.61766411855396,4.04548854604559));
#41235=CARTESIAN_POINT('Ctrl Pts',(20.581213623078,0.520427284318709,4.33591550271974));
#41236=CARTESIAN_POINT('Ctrl Pts',(20.6050715411094,0.295805552416038,4.5441843692251));
#41237=CARTESIAN_POINT('Ctrl Pts',(20.6289294591409,-0.00108183093298003,
4.61939465531364));
#41238=CARTESIAN_POINT('Ctrl Pts',(20.6527873771723,-0.297740088546312,
4.543141139652));
#41239=CARTESIAN_POINT('Ctrl Pts',(20.6766452952037,-0.521574030203058,
4.33407743490148));
#41240=CARTESIAN_POINT('Ctrl Pts',(20.7005032132351,-0.617878846294169,
4.04332131262121));
#41241=CARTESIAN_POINT('Ctrl Pts',(20.7243611312665,-0.563090193646282,
3.74197268265107));
#41242=CARTESIAN_POINT('Ctrl Pts',(20.748219049298,-0.370613436173077,3.50371837193987));
#41243=CARTESIAN_POINT('Ctrl Pts',(20.7720769673294,-0.0875101228827464,
3.38681864340431));
#41244=CARTESIAN_POINT('Ctrl Pts',(20.7959348853608,0.216991017820888,3.41985835035499));
#41245=CARTESIAN_POINT('Ctrl Pts',(20.8197928033922,0.468432357761717,3.59475855107288));
#41246=CARTESIAN_POINT('Ctrl Pts',(20.8436507214236,0.605329007232586,3.86875129405724));
#41247=CARTESIAN_POINT('Ctrl Pts',(20.8675086394551,0.594206341669864,4.17483793696784));
#41248=CARTESIAN_POINT('Ctrl Pts',(20.8913665574864,0.437783978244149,4.43817193323088));
#41249=CARTESIAN_POINT('Ctrl Pts',(20.9152244755179,0.174311539695801,4.5943609607934));
#41250=CARTESIAN_POINT('Ctrl Pts',(20.9390823935493,-0.13178483570001,4.60521254097096));
#41251=CARTESIAN_POINT('Ctrl Pts',(20.9629403115808,-0.405656219889506,
4.46807317049539));
#41252=CARTESIAN_POINT('Ctrl Pts',(20.9867982296121,-0.580333613298163,
4.21647715910241));
#41253=CARTESIAN_POINT('Ctrl Pts',(21.0106561476436,-0.613103627724174,
3.91194658594648));
#41254=CARTESIAN_POINT('Ctrl Pts',(21.034514065675,-0.495953105920446,3.62894747086441));
#41255=CARTESIAN_POINT('Ctrl Pts',(21.0583719837064,-0.257528539509485,
3.43668080652407));
#41256=CARTESIAN_POINT('Ctrl Pts',(21.0822299017379,0.0438687693677006,
3.38216102944232));
#41257=CARTESIAN_POINT('Ctrl Pts',(21.1060878197692,0.334538969374667,3.47871971028568));
#41258=CARTESIAN_POINT('Ctrl Pts',(21.1299457378007,0.543405278604256,3.7027456213393));
#41259=CARTESIAN_POINT('Ctrl Pts',(21.153803655832,0.619394195209021,3.99945832503004));
#41260=CARTESIAN_POINT('Ctrl Pts',(21.1776615738635,0.543924359096133,4.29630348300169));
#41261=CARTESIAN_POINT('Ctrl Pts',(21.2015194918949,0.33545020099803,4.52069436823682));
#41262=CARTESIAN_POINT('Ctrl Pts',(21.2253774099264,0.0449493312674926,
4.61776129700707));
#41263=CARTESIAN_POINT('Ctrl Pts',(21.2492353279577,-0.256542874348706,
4.56376876117982));
#41264=CARTESIAN_POINT('Ctrl Pts',(21.2730932459892,-0.495303359101402,
4.37191940649105));
#41265=CARTESIAN_POINT('Ctrl Pts',(21.2969511640206,-0.612948680759938,
4.08912562603418));
#41266=CARTESIAN_POINT('Ctrl Pts',(21.320809082052,-0.580711353586496,3.78453820227854));
#41267=CARTESIAN_POINT('Ctrl Pts',(21.3446670000834,-0.406474282201139,
3.53263705712739));
#41268=CARTESIAN_POINT('Ctrl Pts',(21.3685249181149,-0.132843176680646,
3.39501888221951));
#41269=CARTESIAN_POINT('Ctrl Pts',(21.3923828361463,0.17327170411384,3.40533506996376));
#41270=CARTESIAN_POINT('Ctrl Pts',(21.4162407541777,0.437016933425986,3.56106303144932));
#41271=CARTESIAN_POINT('Ctrl Pts',(21.4400986722091,0.593899618413251,3.82412303814848));
#41272=CARTESIAN_POINT('Ctrl Pts',(21.4639565902405,0.605557669197671,4.13018975281259));
#41273=CARTESIAN_POINT('Ctrl Pts',(21.4878145082719,0.469140374803543,4.40442152661638));
#41274=CARTESIAN_POINT('Ctrl Pts',(21.5116724263034,0.218005479642704,4.57976122094124));
#41275=CARTESIAN_POINT('Ctrl Pts',(21.5355303443348,-0.0864376936408111,
4.61333350436739));
#41276=CARTESIAN_POINT('Ctrl Pts',(21.5593882623662,-0.369744496313637,
4.49692903910649));
#41277=CARTESIAN_POINT('Ctrl Pts',(21.5832461803976,-0.562638697999917,
4.2590118877088));
#41278=CARTESIAN_POINT('Ctrl Pts',(21.607104098429,-0.617952412054802,3.95775927442416));
#41279=CARTESIAN_POINT('Ctrl Pts',(21.6309620164605,-0.522159928676552,
3.66683566915707));
#41280=CARTESIAN_POINT('Ctrl Pts',(21.6548199344919,-0.298685119385998,
3.45737981799522));
#41281=CARTESIAN_POINT('Ctrl Pts',(21.6786778525233,-0.00217366238626178,
3.38060938201055));
#41282=CARTESIAN_POINT('Ctrl Pts',(21.7025357705547,0.294869314276287,3.45529682398599));
#41283=CARTESIAN_POINT('Ctrl Pts',(21.7263936885862,0.519808711519421,3.66317902991346));
#41284=CARTESIAN_POINT('Ctrl Pts',(21.7502516066175,0.617640719491047,3.95342313784609));
#41285=CARTESIAN_POINT('Ctrl Pts',(21.774109524649,0.564442747351711,4.25505655730362));
#41286=CARTESIAN_POINT('Ctrl Pts',(21.7979674426804,0.373223148373148,4.49432170089927));
#41287=CARTESIAN_POINT('Ctrl Pts',(21.8218253607118,0.0907403232229101,
4.61271172357229));
#41288=CARTESIAN_POINT('Ctrl Pts',(21.8456832787432,-0.213930982672105,
4.58127703989962));
#41289=CARTESIAN_POINT('Ctrl Pts',(21.8695411967746,-0.466290335940828,
4.40770428630285));
#41290=CARTESIAN_POINT('Ctrl Pts',(21.8933991148061,-0.604629000578284,
4.13443672906324));
#41291=CARTESIAN_POINT('Ctrl Pts',(21.9172570328375,-0.595119404811066,
3.82829572958469));
#41292=CARTESIAN_POINT('Ctrl Pts',(21.9411149508689,-0.440086903840403,
3.56414110135311));
#41293=CARTESIAN_POINT('Ctrl Pts',(21.9649728689003,-0.177441167154219,
3.40656584639871));
#41294=CARTESIAN_POINT('Ctrl Pts',(21.9888307869318,0.128593768301574,3.39410140682164));
#41295=CARTESIAN_POINT('Ctrl Pts',(22.0126887049631,0.403184024583593,3.52979567762293));
#41296=CARTESIAN_POINT('Ctrl Pts',(22.0365466229946,0.579184804342829,3.7804677133541));
#41297=CARTESIAN_POINT('Ctrl Pts',(22.060404541026,0.613559122762511,4.08482137310942));
#41298=CARTESIAN_POINT('Ctrl Pts',(22.0842624590574,0.497901522652627,4.36843389665204));
#41299=CARTESIAN_POINT('Ctrl Pts',(22.1081203770888,0.260493437687466,4.56195429652472));
#41300=CARTESIAN_POINT('Ctrl Pts',(22.1319782951203,-0.0406123884881684,
4.61806156357065));
#41301=CARTESIAN_POINT('Ctrl Pts',(22.1558362131517,-0.33178737942464,4.52303594266224));
#41302=CARTESIAN_POINT('Ctrl Pts',(22.1796941311831,-0.541831318374727,
4.30011378656432));
#41303=CARTESIAN_POINT('Ctrl Pts',(22.2035520492145,-0.619382740812877,
4.00380563470766));
#41304=CARTESIAN_POINT('Ctrl Pts',(22.2274099672459,-0.545478211438426,
3.70656690151735));
#41305=CARTESIAN_POINT('Ctrl Pts',(22.2512678852774,-0.338189400908512,
3.48108055383335));
#41306=CARTESIAN_POINT('Ctrl Pts',(22.2751258033088,-0.0482040696311437,
3.38248414587532));
#41307=CARTESIAN_POINT('Ctrl Pts',(22.2989837213402,0.253568469476171,3.43488718493857));
#41308=CARTESIAN_POINT('Ctrl Pts',(22.3228416393716,0.493336611197201,3.62547570084914));
#41309=CARTESIAN_POINT('Ctrl Pts',(22.346699557403,0.612470512379129,3.90764560936005));
#41310=CARTESIAN_POINT('Ctrl Pts',(22.3705574754344,0.581838691587799,4.21239868278141));
#41311=CARTESIAN_POINT('Ctrl Pts',(22.3944153934659,0.408931458591185,4.46521449128699));
#41312=CARTESIAN_POINT('Ctrl Pts',(22.4182733114973,0.13602935083686,4.60427268703701));
#41313=CARTESIAN_POINT('Ctrl Pts',(22.4421312295287,-0.170135649772668,
4.59556974592947));
#41314=CARTESIAN_POINT('Ctrl Pts',(22.4659891475601,-0.434697828443077,
4.44123378804823));
#41315=CARTESIAN_POINT('Ctrl Pts',(22.4898470655916,-0.592964587096883,
4.17900413283907));
#41316=CARTESIAN_POINT('Ctrl Pts',(22.513704983623,-0.606235276705168,3.87300312362118));
#41317=CARTESIAN_POINT('Ctrl Pts',(22.5375629016543,-0.471265070143009,
3.59805624874041));
#41318=CARTESIAN_POINT('Ctrl Pts',(22.5614208196858,-0.22105744785653,3.4213956854475));
#41319=CARTESIAN_POINT('Ctrl Pts',(22.5852787377172,0.0832042338527798,
3.38621941950615));
#41320=CARTESIAN_POINT('Ctrl Pts',(22.6091366557487,0.36712117327337,3.50112963696785));
#41321=CARTESIAN_POINT('Ctrl Pts',(22.63299457378,0.561265174232679,3.7380264683998));
#41322=CARTESIAN_POINT('Ctrl Pts',(22.6568524918115,0.618167971965146,4.03898443479498));
#41323=CARTESIAN_POINT('Ctrl Pts',(22.6807104098429,0.523905402647805,4.33040686810369));
#41324=CARTESIAN_POINT('Ctrl Pts',(22.7045683278744,0.301545895245711,4.54104106792393));
#41325=CARTESIAN_POINT('Ctrl Pts',(22.7284262459057,0.00542710047790416,
4.61936606261506));
#41326=CARTESIAN_POINT('Ctrl Pts',(22.7522841639372,-0.291974666000346,
4.54625809930836));
#41327=CARTESIAN_POINT('Ctrl Pts',(22.7761420819686,-0.518067845615496,
4.33953802216683));
#41328=CARTESIAN_POINT('Ctrl Pts',(22.7920473606562,-0.584213376873476,
4.14642833911731));
#41329=CARTESIAN_POINT('Ctrl Pts',(22.8,-0.592174260192535,4.04779597854866));
#41330=CARTESIAN_POINT('Ctrl Pts',(3.96816317011931,-0.282716247115855,
3.54616445487434));
#41331=CARTESIAN_POINT('Ctrl Pts',(3.97611580946312,-0.207125539895404,
3.49907532469992));
#41332=CARTESIAN_POINT('Ctrl Pts',(3.99202108815073,-0.0320395462633344,
3.44344227840288));
#41333=CARTESIAN_POINT('Ctrl Pts',(4.01587900618214,0.238586678544665,3.49618207793602));
#41334=CARTESIAN_POINT('Ctrl Pts',(4.03973692421357,0.450798406251909,3.67207593825259));
#41335=CARTESIAN_POINT('Ctrl Pts',(4.06359484224498,0.552814952159096,3.92817792166325));
#41336=CARTESIAN_POINT('Ctrl Pts',(4.0874527602764,0.519633627921064,4.20183097195279));
#41337=CARTESIAN_POINT('Ctrl Pts',(4.11131067830782,0.359398059257131,4.42613686623617));
#41338=CARTESIAN_POINT('Ctrl Pts',(4.13516859633924,0.11127440638865,4.54623750576341));
#41339=CARTESIAN_POINT('Ctrl Pts',(4.15902651437066,-0.164055973910312,
4.53276988152218));
#41340=CARTESIAN_POINT('Ctrl Pts',(4.18288443240208,-0.399271733473279,
4.38902461621758));
#41341=CARTESIAN_POINT('Ctrl Pts',(4.2067423504335,-0.536853866020863,4.15015270818839));
#41342=CARTESIAN_POINT('Ctrl Pts',(4.23060026846491,-0.543161034884179,
3.87456412255522));
#41343=CARTESIAN_POINT('Ctrl Pts',(4.25445818649634,-0.416650307492554,
3.62964815836115));
#41344=CARTESIAN_POINT('Ctrl Pts',(4.27831610452775,-0.188257351244862,
3.47529323740438));
#41345=CARTESIAN_POINT('Ctrl Pts',(4.30217402255918,0.0861697193074588,
3.44924344981891));
#41346=CARTESIAN_POINT('Ctrl Pts',(4.32603194059059,0.339525912432458,3.55786862136322));
#41347=CARTESIAN_POINT('Ctrl Pts',(4.34988985862202,0.509858789389686,3.77460696883261));
#41348=CARTESIAN_POINT('Ctrl Pts',(4.37374777665342,0.555517294574929,4.0464600464808));
#41349=CARTESIAN_POINT('Ctrl Pts',(4.39760569468486,0.465336694276122,4.30695238014399));
#41350=CARTESIAN_POINT('Ctrl Pts',(4.42146361271626,0.261368594047533,4.4923864940975));
#41351=CARTESIAN_POINT('Ctrl Pts',(4.4453215307477,-0.00651124555331369,
4.55741869872598));
#41352=CARTESIAN_POINT('Ctrl Pts',(4.4691794487791,-0.272798909000308,4.48614684730087));
#41353=CARTESIAN_POINT('Ctrl Pts',(4.49303736681053,-0.472379807908186,
4.29599884956661));
#41354=CARTESIAN_POINT('Ctrl Pts',(4.51689528484195,-0.55645097662433,4.03347107014466));
#41355=CARTESIAN_POINT('Ctrl Pts',(4.54075320287336,-0.504454724024634,
3.76275870240323));
#41356=CARTESIAN_POINT('Ctrl Pts',(4.56461112090479,-0.329105550388866,
3.55005829421323));
#41357=CARTESIAN_POINT('Ctrl Pts',(4.5884690389362,-0.0732811049967102,
3.44738088927219));
#41358=CARTESIAN_POINT('Ctrl Pts',(4.61232695696762,0.200462566687888,3.47983390993684));
#41359=CARTESIAN_POINT('Ctrl Pts',(4.63618487499904,0.425187680335341,3.63948170866684));
#41360=CARTESIAN_POINT('Ctrl Pts',(4.66004279303046,0.54594282425631,3.88728604994618));
#41361=CARTESIAN_POINT('Ctrl Pts',(4.68390071106188,0.533200076465109,4.16265202228146));
#41362=CARTESIAN_POINT('Ctrl Pts',(4.7077586290933,0.390075385898422,4.39824514461603));
#41363=CARTESIAN_POINT('Ctrl Pts',(4.73161654712472,0.151566638040082,4.53645648111246));
#41364=CARTESIAN_POINT('Ctrl Pts',(4.75547446515614,-0.124004281411749,
4.54348959519552));
#41365=CARTESIAN_POINT('Ctrl Pts',(4.77933238318755,-0.369252776249408,
4.41762469889406));
#41366=CARTESIAN_POINT('Ctrl Pts',(4.80319030121898,-0.524208909050512,
4.18963918784455));
#41367=CARTESIAN_POINT('Ctrl Pts',(4.82704821925039,-0.550981684424725,
3.91528172969931));
#41368=CARTESIAN_POINT('Ctrl Pts',(4.85090613728181,-0.443024429517375,
3.66164019632193));
#41369=CARTESIAN_POINT('Ctrl Pts',(4.87476405531323,-0.226735633849849,
3.49073685167984));
#41370=CARTESIAN_POINT('Ctrl Pts',(4.89862197334465,0.0449962004486201,
3.44436221885167));
#41371=CARTESIAN_POINT('Ctrl Pts',(4.92247989137607,0.305725238065515,3.53385615878353));
#41372=CARTESIAN_POINT('Ctrl Pts',(4.94633780940749,0.491696127187109,3.73733496539613));
#41373=CARTESIAN_POINT('Ctrl Pts',(4.9701957274389,0.557433919677865,4.00504252782125));
#41374=CARTESIAN_POINT('Ctrl Pts',(4.99405364547033,0.486863934612277,4.27151705483839));
#41375=CARTESIAN_POINT('Ctrl Pts',(5.01791156350174,0.297242455626679,4.47159826597145));
#41376=CARTESIAN_POINT('Ctrl Pts',(5.04176948153317,0.0349370995184326,
4.55636085499566));
#41377=CARTESIAN_POINT('Ctrl Pts',(5.06562739956458,-0.235911329089554,
4.505078060008));
#41378=CARTESIAN_POINT('Ctrl Pts',(5.08948531759601,-0.449073011639563,
4.33028992129829));
#41379=CARTESIAN_POINT('Ctrl Pts',(5.11334323562741,-0.552424110340463,
4.07473689991432));
#41380=CARTESIAN_POINT('Ctrl Pts',(5.13720115365885,-0.520692466332485,
3.80090867070902));
#41381=CARTESIAN_POINT('Ctrl Pts',(5.16105907169026,-0.361637330928202,
3.57576369465428));
#41382=CARTESIAN_POINT('Ctrl Pts',(5.18491698972168,-0.114152017308863,
3.45435605122152));
#41383=CARTESIAN_POINT('Ctrl Pts',(5.2087749077531,0.161246573981014,3.46637321630784));
#41384=CARTESIAN_POINT('Ctrl Pts',(5.23263282578452,0.397215985664045,3.60887666570863));
#41385=CARTESIAN_POINT('Ctrl Pts',(5.25649074381594,0.536055268906009,3.84702042432939));
#41386=CARTESIAN_POINT('Ctrl Pts',(5.28034866184735,0.543814437048104,4.12257185628156));
#41387=CARTESIAN_POINT('Ctrl Pts',(5.30420657987878,0.418596162124088,4.3681511305826));
#41388=CARTESIAN_POINT('Ctrl Pts',(5.32806449791019,0.191019723230217,4.5237074252207));
#41389=CARTESIAN_POINT('Ctrl Pts',(5.35192241594161,-0.0832662412662402,
4.55120298888854));
#41390=CARTESIAN_POINT('Ctrl Pts',(5.37578033397303,-0.337191341646214,
4.44391440730515));
#41391=CARTESIAN_POINT('Ctrl Pts',(5.39963825200445,-0.508663974085987,
4.22807666114996));
#41392=CARTESIAN_POINT('Ctrl Pts',(5.42349617003587,-0.555754409133215,
3.95646795866016));
#41393=CARTESIAN_POINT('Ctrl Pts',(5.4473540880673,-0.466947752701331,3.69550402606682));
#41394=CARTESIAN_POINT('Ctrl Pts',(5.47121200609871,-0.263959651332346,
3.50899765340418));
#41395=CARTESIAN_POINT('Ctrl Pts',(5.49506992413013,0.00357377490351851,
3.44255472911916));
#41396=CARTESIAN_POINT('Ctrl Pts',(5.51892784216155,0.270233315828591,3.51242235806964));
#41397=CARTESIAN_POINT('Ctrl Pts',(5.54278576019296,0.470813450024345,3.70151600181885));
#41398=CARTESIAN_POINT('Ctrl Pts',(5.56664367822439,0.556266870991092,3.96359711366712));
#41399=CARTESIAN_POINT('Ctrl Pts',(5.5905015962558,0.505697889589837,4.23457972281303));
#41400=CARTESIAN_POINT('Ctrl Pts',(5.61435951428722,0.331471999260015,4.4482011999181));
#41401=CARTESIAN_POINT('Ctrl Pts',(5.63821743231864,0.0761921759760934,
4.55222527486821));
#41402=CARTESIAN_POINT('Ctrl Pts',(5.66207535035006,-0.197718709731212,
4.52121522783523));
#41403=CARTESIAN_POINT('Ctrl Pts',(5.68593326838148,-0.423281985227643,
4.3627538599096));
#41404=CARTESIAN_POINT('Ctrl Pts',(5.70979118641289,-0.545341285237878,
4.11558929214995));
#41405=CARTESIAN_POINT('Ctrl Pts',(5.73364910444432,-0.534049786451273,
3.84015999362387));
#41406=CARTESIAN_POINT('Ctrl Pts',(5.75750702247573,-0.392168567195948,
3.6038159310769));
#41407=CARTESIAN_POINT('Ctrl Pts',(5.78136494050716,-0.154391451667357,
3.46434966433946));
#41408=CARTESIAN_POINT('Ctrl Pts',(5.80522285853857,0.121138580962943,3.45586449715393));
#41409=CARTESIAN_POINT('Ctrl Pts',(5.82908077656999,0.367046927720705,3.58043527923202));
#41410=CARTESIAN_POINT('Ctrl Pts',(5.85293869460141,0.523202308305842,3.80760107017232));
#41411=CARTESIAN_POINT('Ctrl Pts',(5.87679661263283,0.551420461789987,4.08181362911724));
#41412=CARTESIAN_POINT('Ctrl Pts',(5.90065453066425,0.44480131269862,4.33602054829434));
#41413=CARTESIAN_POINT('Ctrl Pts',(5.92451244869567,0.229416087376931,4.50806125053784));
#41414=CARTESIAN_POINT('Ctrl Pts',(5.94837036672709,-0.042067546589846,
4.55586721297736));
#41415=CARTESIAN_POINT('Ctrl Pts',(5.97222828475851,-0.30326465903273,4.46774835821298));
#41416=CARTESIAN_POINT('Ctrl Pts',(5.99608620278993,-0.490305038147314,
4.26525255699254));
#41417=CARTESIAN_POINT('Ctrl Pts',(6.01994412082133,-0.557452977205748,
3.99789477357902));
#41418=CARTESIAN_POINT('Ctrl Pts',(6.04380203885278,-0.488287539408226,
3.73105273207384));
#41419=CARTESIAN_POINT('Ctrl Pts',(6.06765995688417,-0.299724270968661,
3.52997381710292));
#41420=CARTESIAN_POINT('Ctrl Pts',(6.09151787491561,-0.0378669053578504,
3.44383251805177));
#41421=CARTESIAN_POINT('Ctrl Pts',(6.11537579294702,0.233243627260218,3.49368287747685));
#41422=CARTESIAN_POINT('Ctrl Pts',(6.13923371097844,0.447331678364145,3.6673537262422));
#41423=CARTESIAN_POINT('Ctrl Pts',(6.16309162900986,0.552012406214274,3.92234268746235));
#41424=CARTESIAN_POINT('Ctrl Pts',(6.18694954704127,0.521753629494025,4.19636433484848));
#41425=CARTESIAN_POINT('Ctrl Pts',(6.2108074650727,0.363831507594212,4.42228768590875));
#41426=CARTESIAN_POINT('Ctrl Pts',(6.23466538310411,0.117094415953721,4.54510476979165));
#41427=CARTESIAN_POINT('Ctrl Pts',(6.25852330113554,-0.158561881267111,
4.53433708369694));
#41428=CARTESIAN_POINT('Ctrl Pts',(6.28238121916695,-0.394905399742298,
4.39345989467659));
#41429=CARTESIAN_POINT('Ctrl Pts',(6.30623913719837,-0.535697351746728,
4.1553358869807));
#41430=CARTESIAN_POINT('Ctrl Pts',(6.33009705522979,-0.543633587309765,
3.88114808171798));
#41431=CARTESIAN_POINT('Ctrl Pts',(6.36190761260502,-0.381130543103143,
3.54983775818315));
#41432=CARTESIAN_POINT('Ctrl Pts',(6.40167080932404,0.0904237977681596,
3.37418170676098));
#41433=CARTESIAN_POINT('Ctrl Pts',(6.4493866453869,0.576013642360818,3.73827828410759));
#41434=CARTESIAN_POINT('Ctrl Pts',(6.49710248144972,0.531303907723303,4.34259299019566));
#41435=CARTESIAN_POINT('Ctrl Pts',(6.54481831751257,-0.000617460830772086,
4.63236849138271));
#41436=CARTESIAN_POINT('Ctrl Pts',(6.5925341535754,-0.532336898979176,4.34139325430452));
#41437=CARTESIAN_POINT('Ctrl Pts',(6.64024998963824,-0.575010046738857,
3.73693099107234));
#41438=CARTESIAN_POINT('Ctrl Pts',(6.68796582570108,-0.0897448725589052,
3.37403863313417));
#41439=CARTESIAN_POINT('Ctrl Pts',(6.73568166176391,0.477988548433368,3.58598174571673));
#41440=CARTESIAN_POINT('Ctrl Pts',(6.78339749782676,0.606749053262868,4.17812127049189));
#41441=CARTESIAN_POINT('Ctrl Pts',(6.83111333388958,0.178337754027021,4.60669083891839));
#41442=CARTESIAN_POINT('Ctrl Pts',(6.87882916995244,-0.413851892207341,
4.47812605548031));
#41443=CARTESIAN_POINT('Ctrl Pts',(6.92654500601527,-0.625990718083913,
3.91049119230943));
#41444=CARTESIAN_POINT('Ctrl Pts',(6.97426084207811,-0.263274891453005,
3.42505341469988));
#41445=CARTESIAN_POINT('Ctrl Pts',(7.02197667814094,0.341211513798207,3.46759805477058));
#41446=CARTESIAN_POINT('Ctrl Pts',(7.06969251420378,0.63235750294684,3.99905552874491));
#41447=CARTESIAN_POINT('Ctrl Pts',(7.11740835026662,0.342800202184808,4.53138035934227));
#41448=CARTESIAN_POINT('Ctrl Pts',(7.16512418632946,-0.261555976381552,
4.57573041153878));
#41449=CARTESIAN_POINT('Ctrl Pts',(7.2128400223923,-0.625721183287191,4.0913783776429));
#41450=CARTESIAN_POINT('Ctrl Pts',(7.26055585845514,-0.41527704940159,3.52311216844965));
#41451=CARTESIAN_POINT('Ctrl Pts',(7.30827169451797,0.176522415171576,3.39277939551711));
#41452=CARTESIAN_POINT('Ctrl Pts',(7.35598753058081,0.606218615784068,3.8200666455489));
#41453=CARTESIAN_POINT('Ctrl Pts',(7.40370336664364,0.479214941044062,4.4125894643569));
#41454=CARTESIAN_POINT('Ctrl Pts',(7.4514192027065,-0.0878591916424711,
4.62622502914213));
#41455=CARTESIAN_POINT('Ctrl Pts',(7.49913503876932,-0.574250874682306,
4.26478851416677));
#41456=CARTESIAN_POINT('Ctrl Pts',(7.54685087483217,-0.53329914461431,3.6601926322252));
#41457=CARTESIAN_POINT('Ctrl Pts',(7.594566710895,-0.00261060360317682,
3.36764708477891));
#41458=CARTESIAN_POINT('Ctrl Pts',(7.64228254695784,0.530475294557976,3.65580094934904));
#41459=CARTESIAN_POINT('Ctrl Pts',(7.68999838302067,0.576417567478113,4.26003809833172));
#41460=CARTESIAN_POINT('Ctrl Pts',(7.73771421908353,0.093026718772369,4.62547826040714));
#41461=CARTESIAN_POINT('Ctrl Pts',(7.78543005514634,-0.475791997136335,
4.41653211173522));
#41462=CARTESIAN_POINT('Ctrl Pts',(7.8331458912092,-0.607683601098078,3.82507811568403));
#41463=CARTESIAN_POINT('Ctrl Pts',(7.88086172727203,-0.181530003744534,
3.39425757752065));
#41464=CARTESIAN_POINT('Ctrl Pts',(7.92857756333487,0.411325389238953,3.51969962646458));
#41465=CARTESIAN_POINT('Ctrl Pts',(7.97629339939771,0.626454348233276,4.08620889879763));
#41466=CARTESIAN_POINT('Ctrl Pts',(8.02400923546054,0.266300640003926,4.57355121287022));
#41467=CARTESIAN_POINT('Ctrl Pts',(8.07172507152339,-0.338401043502061,
4.5341926229444));
#41468=CARTESIAN_POINT('Ctrl Pts',(8.11944090758622,-0.632343841791292,
4.00427672775865));
#41469=CARTESIAN_POINT('Ctrl Pts',(8.16715674364906,-0.345595560302635,
3.47043344766624));
#41470=CARTESIAN_POINT('Ctrl Pts',(8.2148725797119,0.258518441882999,3.42289928101069));
#41471=CARTESIAN_POINT('Ctrl Pts',(8.26258841577473,0.625230981070026,3.90532558443901));
#41472=CARTESIAN_POINT('Ctrl Pts',(8.31030425183758,0.417784289925175,4.47469286043008));
#41473=CARTESIAN_POINT('Ctrl Pts',(8.35802008790041,-0.173320143095541,
4.60814237859973));
#41474=CARTESIAN_POINT('Ctrl Pts',(8.40573592396325,-0.605262021838435,
4.18312539302794));
#41475=CARTESIAN_POINT('Ctrl Pts',(8.45345176002609,-0.481382472773795,
3.58994154129225));
#41476=CARTESIAN_POINT('Ctrl Pts',(8.50116759608892,0.0845580080604409,
3.37332068174828));
#41477=CARTESIAN_POINT('Ctrl Pts',(8.54888343215178,0.572847569000584,3.73218908285563));
#41478=CARTESIAN_POINT('Ctrl Pts',(8.59659926821459,0.535082392934658,4.33699236997728));
#41479=CARTESIAN_POINT('Ctrl Pts',(8.64431510427745,0.00594282213592907,
4.6323303784547));
#41480=CARTESIAN_POINT('Ctrl Pts',(8.69203094034027,-0.528654133672296,
4.34698967074364));
#41481=CARTESIAN_POINT('Ctrl Pts',(8.73974677640312,-0.577779864139828,
3.74300300926635));
#41482=CARTESIAN_POINT('Ctrl Pts',(8.78746261246595,-0.0963214550818077,
3.37502063878676));
#41483=CARTESIAN_POINT('Ctrl Pts',(8.8351784485288,0.473590428273928,3.58096643225285));
#41484=CARTESIAN_POINT('Ctrl Pts',(8.88289428459164,0.608596934220305,4.17171719864135));
#41485=CARTESIAN_POINT('Ctrl Pts',(8.93061012065447,0.184719511004659,4.60477741930878));
#41486=CARTESIAN_POINT('Ctrl Pts',(8.97832595671731,-0.408788681441581,
4.48246123012823));
#41487=CARTESIAN_POINT('Ctrl Pts',(9.02604179278014,-0.626899937697651,
3.91709346970068));
#41488=CARTESIAN_POINT('Ctrl Pts',(9.07375762884299,-0.269319335070538,
3.42786005172794));
#41489=CARTESIAN_POINT('Ctrl Pts',(9.12147346490582,0.335581356962483,3.46403155175812));
#41490=CARTESIAN_POINT('Ctrl Pts',(9.16918930096866,0.632312525313962,3.99239112474344));
#41491=CARTESIAN_POINT('Ctrl Pts',(9.21690513703149,0.348381372290835,4.52773804495445));
#41492=CARTESIAN_POINT('Ctrl Pts',(9.26462097309434,-0.255473755443411,
4.5784549981902));
#41493=CARTESIAN_POINT('Ctrl Pts',(9.31233680915717,-0.624723402584967,
4.09796782591368));
#41494=CARTESIAN_POINT('Ctrl Pts',(9.36005264522002,-0.420279936527615,
3.52751529167185));
#41495=CARTESIAN_POINT('Ctrl Pts',(9.40776848128285,0.170113062081096,3.39095273519949));
#41496=CARTESIAN_POINT('Ctrl Pts',(9.45548431734569,0.604288618254829,3.81368765339017));
#41497=CARTESIAN_POINT('Ctrl Pts',(9.50320015340853,0.483536638109595,4.40751606625661));
#41498=CARTESIAN_POINT('Ctrl Pts',(9.55091598947137,-0.0812544769791981,
4.62711620503893));
#41499=CARTESIAN_POINT('Ctrl Pts',(9.5986318255342,-0.571428355597161,4.27082588331087));
#41500=CARTESIAN_POINT('Ctrl Pts',(9.64634766159704,-0.536850782714826,
3.66583198574659));
#41501=CARTESIAN_POINT('Ctrl Pts',(9.69406349765987,-0.0092748755543832,
3.36770971750703));
#41502=CARTESIAN_POINT('Ctrl Pts',(9.74177933372272,0.52681829253995,3.65022934471732));
#41503=CARTESIAN_POINT('Ctrl Pts',(9.78949516978555,0.579126116453474,4.253948746587));
#41504=CARTESIAN_POINT('Ctrl Pts',(9.83721100584839,0.099613516627068,4.62446310696212));
#41505=CARTESIAN_POINT('Ctrl Pts',(9.88492684191123,-0.471375708268938,
4.42152338761395));
#41506=CARTESIAN_POINT('Ctrl Pts',(9.93264267797408,-0.609493367214024,
3.83149225544889));
#41507=CARTESIAN_POINT('Ctrl Pts',(9.9803585140369,-0.187903888785556,3.39620437793004));
#41508=CARTESIAN_POINT('Ctrl Pts',(10.0280743500997,0.406240621987656,3.51539131074786));
#41509=CARTESIAN_POINT('Ctrl Pts',(10.0757901861626,0.627328118774167,4.07960185956908));
#41510=CARTESIAN_POINT('Ctrl Pts',(10.1235060222254,0.27233055140652,4.57071279591595));
#41511=CARTESIAN_POINT('Ctrl Pts',(10.1712218582883,-0.332752351661881,
4.5377293902281));
#41512=CARTESIAN_POINT('Ctrl Pts',(10.2189376943511,-0.632263650146131,
4.01094081146358));
#41513=CARTESIAN_POINT('Ctrl Pts',(10.2666535304139,-0.351157510074434,
3.47410511718603));
#41514=CARTESIAN_POINT('Ctrl Pts',(10.3143693664768,0.252421974751429,3.42020678572945));
#41515=CARTESIAN_POINT('Ctrl Pts',(10.3620852025396,0.624198476151732,3.89874148420283));
#41516=CARTESIAN_POINT('Ctrl Pts',(10.4098010386024,0.422763912373798,4.47026343579529));
#41517=CARTESIAN_POINT('Ctrl Pts',(10.4575168746653,-0.166901257195935,
4.60993523836389));
#41518=CARTESIAN_POINT('Ctrl Pts',(10.5052327107281,-0.603298434176698,
4.18949412648294));
#41519=CARTESIAN_POINT('Ctrl Pts',(10.552948546791,-0.485677376113382,3.5950376425108));
#41520=CARTESIAN_POINT('Ctrl Pts',(10.6006643828538,0.0779486895418537,
3.3724643225678));
#41521=CARTESIAN_POINT('Ctrl Pts',(10.6483802189166,0.569993274196054,3.72616667108832));
#41522=CARTESIAN_POINT('Ctrl Pts',(10.6960960549795,0.538604264682155,4.3313343790158));
#41523=CARTESIAN_POINT('Ctrl Pts',(10.7438118910423,0.0126066714187673,
4.63223262845832));
#41524=CARTESIAN_POINT('Ctrl Pts',(10.7915277271052,-0.524967822187051,
4.35254192703816));
#41525=CARTESIAN_POINT('Ctrl Pts',(10.839243563168,-0.580456287010268,3.74910654946403));
#41526=CARTESIAN_POINT('Ctrl Pts',(10.8869593992308,-0.102902812003948,
3.37607048800905));
#41527=CARTESIAN_POINT('Ctrl Pts',(10.9346752352937,0.469147898628881,3.5759984978049));
#41528=CARTESIAN_POINT('Ctrl Pts',(10.9823910713565,0.610372875182502,4.16529361116822));
#41529=CARTESIAN_POINT('Ctrl Pts',(11.0301069074193,0.191083048662156,4.60279705802663));
#41530=CARTESIAN_POINT('Ctrl Pts',(11.0778227434822,-0.403681281635282,
4.48674269127424));
#41531=CARTESIAN_POINT('Ctrl Pts',(11.125538579545,-0.627738879572117,3.92370502162571));
#41532=CARTESIAN_POINT('Ctrl Pts',(11.1732544156079,-0.275334205393669,
3.43073020456744));
#41533=CARTESIAN_POINT('Ctrl Pts',(11.2209702516707,0.329914106159097,3.46052459999659));
#41534=CARTESIAN_POINT('Ctrl Pts',(11.2686860877335,0.632197217644931,3.98572755614488));
#41535=CARTESIAN_POINT('Ctrl Pts',(11.3164019237964,0.353923896562866,4.52403711709511));
#41536=CARTESIAN_POINT('Ctrl Pts',(11.3641177598592,-0.24936318455202,4.58111533006939));
#41537=CARTESIAN_POINT('Ctrl Pts',(11.411833595922,-0.623656216347001,4.10454639383227));
#41538=CARTESIAN_POINT('Ctrl Pts',(11.4595494319849,-0.425236148486169,
3.53197089548594));
#41539=CARTESIAN_POINT('Ctrl Pts',(11.5072652680477,0.163684817628688,3.3891937253683));
#41540=CARTESIAN_POINT('Ctrl Pts',(11.5549811041106,0.602291497100466,3.80732935570755));
#41541=CARTESIAN_POINT('Ctrl Pts',(11.6026969401734,0.487804627338989,4.40239740331947));
#41542=CARTESIAN_POINT('Ctrl Pts',(11.6504127762363,-0.0746407375468588,
4.62793772378323));
#41543=CARTESIAN_POINT('Ctrl Pts',(11.6981286122991,-0.568542364648052,
4.276833170433));
#41544=CARTESIAN_POINT('Ctrl Pts',(11.7458444483619,-0.540342790144192,
3.67150845704832));
#41545=CARTESIAN_POINT('Ctrl Pts',(11.7935602844247,-0.0159381172083995,
3.36784258204823));
#41546=CARTESIAN_POINT('Ctrl Pts',(11.8412761204876,0.523102773999324,3.64469659094542));
#41547=CARTESIAN_POINT('Ctrl Pts',(11.8889919565504,0.581770338872691,4.24783118742311));
#41548=CARTESIAN_POINT('Ctrl Pts',(11.9367077926133,0.106189249871976,4.62337859111715));
#41549=CARTESIAN_POINT('Ctrl Pts',(11.9844236286761,-0.466907061217805,
4.4264678426758));
#41550=CARTESIAN_POINT('Ctrl Pts',(12.0321394647389,-0.611235433702689,
3.83792511225401));
#41551=CARTESIAN_POINT('Ctrl Pts',(12.0798553008018,-0.19425690235234,3.39821824509208));
#41552=CARTESIAN_POINT('Ctrl Pts',(12.1275711368646,0.401110731454808,3.51113682306459));
#41553=CARTESIAN_POINT('Ctrl Pts',(12.1752869729275,0.628132208685083,4.07298597854376));
#41554=CARTESIAN_POINT('Ctrl Pts',(12.2230028089903,0.27833021362349,4.56781098689255));
#41555=CARTESIAN_POINT('Ctrl Pts',(12.2707186450531,-0.327066699269377,
4.54120642908287));
#41556=CARTESIAN_POINT('Ctrl Pts',(12.3184344811159,-0.632113229655128,
4.01760367991507));
#41557=CARTESIAN_POINT('Ctrl Pts',(12.3661503171788,-0.356680454936339,
3.47783520061383));
#41558=CARTESIAN_POINT('Ctrl Pts',(12.4138661532416,0.246297469784735,3.4175786911271));
#41559=CARTESIAN_POINT('Ctrl Pts',(12.4615819893045,0.623096638228782,3.89216863128209));
#41560=CARTESIAN_POINT('Ctrl Pts',(12.5092978253673,0.427696576213203,4.46578177652963));
#41561=CARTESIAN_POINT('Ctrl Pts',(12.5570136614302,-0.16046383269669,4.61166034941614));
#41562=CARTESIAN_POINT('Ctrl Pts',(12.604729497493,-0.601267834987779,4.1958418118296));
#41563=CARTESIAN_POINT('Ctrl Pts',(12.6524453335558,-0.489918332714758,
3.60017872502631));
#41564=CARTESIAN_POINT('Ctrl Pts',(12.7001611696187,0.0713307128527425,
3.37167766707246));
#41565=CARTESIAN_POINT('Ctrl Pts',(12.7478770056815,0.56707566724347,3.72017467542775));
#41566=CARTESIAN_POINT('Ctrl Pts',(12.7955928417444,0.542066310823814,4.32563958500381));
#41567=CARTESIAN_POINT('Ctrl Pts',(12.8433086778072,0.0192691204123526,
4.63206465306178));
#41568=CARTESIAN_POINT('Ctrl Pts',(12.89102451387,-0.521223199767296,4.35805502464836));
#41569=CARTESIAN_POINT('Ctrl Pts',(12.9387403499329,-0.583068235550835,
3.7552379577156));
#41570=CARTESIAN_POINT('Ctrl Pts',(12.9864561859957,-0.109472738970043,
3.37718964036075));
#41571=CARTESIAN_POINT('Ctrl Pts',(13.0341720220585,0.464653258261548,3.57107765943178));
#41572=CARTESIAN_POINT('Ctrl Pts',(13.0818878581214,0.612081018822183,4.15885166366515));
#41573=CARTESIAN_POINT('Ctrl Pts',(13.1296036941842,0.197425361721354,4.6007497409078));
#41574=CARTESIAN_POINT('Ctrl Pts',(13.177319530247,-0.398529042827853,4.49097008735187));
#41575=CARTESIAN_POINT('Ctrl Pts',(13.2250353663099,-0.628508095190705,
3.93032504803489));
#41576=CARTESIAN_POINT('Ctrl Pts',(13.2727512023727,-0.281318492899819,
3.4336635891944));
#41577=CARTESIAN_POINT('Ctrl Pts',(13.3204670384356,0.324210210062374,3.45707757060249));
#41578=CARTESIAN_POINT('Ctrl Pts',(13.3681828744984,0.632011688508986,3.97906557286167));
#41579=CARTESIAN_POINT('Ctrl Pts',(13.4158987105612,0.359427108647973,4.52027798167956));
#41580=CARTESIAN_POINT('Ctrl Pts',(13.4636145466241,-0.243224915581421,
4.58371111441534));
#41581=CARTESIAN_POINT('Ctrl Pts',(13.5113303826869,-0.622519757336015,
4.11111334923356));
#41582=CARTESIAN_POINT('Ctrl Pts',(13.5590462187498,-0.430145127231255,
3.53647848575196));
#41583=CARTESIAN_POINT('Ctrl Pts',(13.6067620548126,0.157238391843492,3.38750256099959));
#41584=CARTESIAN_POINT('Ctrl Pts',(13.6544778908755,0.600227476264717,3.8009924589658));
#41585=CARTESIAN_POINT('Ctrl Pts',(13.7021937269383,0.492018433545193,4.39723404398833));
#41586=CARTESIAN_POINT('Ctrl Pts',(13.7499095630011,-0.0680187073756014,
4.62868949418496));
#41587=CARTESIAN_POINT('Ctrl Pts',(13.797625399064,-0.565593222711038,4.28280970824024));
#41588=CARTESIAN_POINT('Ctrl Pts',(13.8453412351268,-0.543774778860562,
3.67722141563181));
#41589=CARTESIAN_POINT('Ctrl Pts',(13.8930570711896,-0.0225995885319848,
3.36804566363559));
#41590=CARTESIAN_POINT('Ctrl Pts',(13.9407729072525,0.519329151684885,3.63920330259016));
#41591=CARTESIAN_POINT('Ctrl Pts',(13.9884887433153,0.584349941003394,4.24168610034696));
#41592=CARTESIAN_POINT('Ctrl Pts',(14.0362045793781,0.112753188118911,4.62222483333648));
#41593=CARTESIAN_POINT('Ctrl Pts',(14.083920415441,-0.462386552345973,4.43136492771341));
#41594=CARTESIAN_POINT('Ctrl Pts',(14.1316362515038,-0.612909607059929,
3.84437597156854));
#41595=CARTESIAN_POINT('Ctrl Pts',(14.1793520875667,-0.200588338784227,
3.40029895531576));
#41596=CARTESIAN_POINT('Ctrl Pts',(14.2270679236295,0.395936287445344,3.50693663598317));
#41597=CARTESIAN_POINT('Ctrl Pts',(14.2747837596923,0.628866528650988,4.06636199058228));
#41598=CARTESIAN_POINT('Ctrl Pts',(14.3224995957552,0.284298960241116,4.5648461081192));
#41599=CARTESIAN_POINT('Ctrl Pts',(14.370215431818,-0.321344717859966,4.54462335329573));
#41600=CARTESIAN_POINT('Ctrl Pts',(14.4179312678809,-0.631892597026201,
4.02426459303334));
#41601=CARTESIAN_POINT('Ctrl Pts',(14.4656471039437,-0.362163781425906,
3.48162328362967));
#41602=CARTESIAN_POINT('Ctrl Pts',(14.5133629400065,0.240145607263868,3.41501528911991));
#41603=CARTESIAN_POINT('Ctrl Pts',(14.5610787760693,0.6219255896881,3.8856077557581));
#41604=CARTESIAN_POINT('Ctrl Pts',(14.6087946121322,0.432581733546503,4.46124838043455));
#41605=CARTESIAN_POINT('Ctrl Pts',(14.656510448195,-0.154008584636381,4.61331752013935));
#41606=CARTESIAN_POINT('Ctrl Pts',(14.7042262842579,-0.599170449821005,
4.20216774399712));
#41607=CARTESIAN_POINT('Ctrl Pts',(14.7519421203207,-0.494104871512583,
3.60536421779174));
#41608=CARTESIAN_POINT('Ctrl Pts',(14.7996579563836,0.0647048130865326,
3.37096080264023));
#41609=CARTESIAN_POINT('Ctrl Pts',(14.8473737924464,0.564095072216763,3.71421376143635));
#41610=CARTESIAN_POINT('Ctrl Pts',(14.8950896285093,0.545468146811986,4.319908620492));
#41611=CARTESIAN_POINT('Ctrl Pts',(14.942805464572,0.0259294290834894,4.63182647092298));
#41612=CARTESIAN_POINT('Ctrl Pts',(14.9905213006349,-0.517420682347921,
4.36352835120552));
#41613=CARTESIAN_POINT('Ctrl Pts',(15.0382371366977,-0.585615419638682,
3.76139655297334));
#41614=CARTESIAN_POINT('Ctrl Pts',(15.0859529727606,-0.116030506223773,
3.3783779715317));
#41615=CARTESIAN_POINT('Ctrl Pts',(15.1336688088234,0.460107006415252,3.56620446371685));
#41616=CARTESIAN_POINT('Ctrl Pts',(15.1813846448862,0.613721175406852,4.15239207167311));
#41617=CARTESIAN_POINT('Ctrl Pts',(15.2291004809491,0.203745745708236,4.59863569535852));
#41618=CARTESIAN_POINT('Ctrl Pts',(15.2768163170119,-0.393332537305518,
4.49514294880206));
#41619=CARTESIAN_POINT('Ctrl Pts',(15.3245321530748,-0.629207499112597,
3.93695281360709));
#41620=CARTESIAN_POINT('Ctrl Pts',(15.3722479891376,-0.287271532882751,
3.43665987978239));
#41621=CARTESIAN_POINT('Ctrl Pts',(15.4199638252004,0.318470302234025,3.45369084645546));
#41622=CARTESIAN_POINT('Ctrl Pts',(15.4676796612633,0.631755958513824,3.97240591487529));
#41623=CARTESIAN_POINT('Ctrl Pts',(15.5153954973261,0.364890397275464,4.51646105625472));
#41624=CARTESIAN_POINT('Ctrl Pts',(15.563111333389,-0.237059630341402,4.58624206290064));
#41625=CARTESIAN_POINT('Ctrl Pts',(15.6108271694518,-0.621314151784485,
4.11766796269128));
#41626=CARTESIAN_POINT('Ctrl Pts',(15.6585430055147,-0.435006327496808,
3.54103756178819));
#41627=CARTESIAN_POINT('Ctrl Pts',(15.7062588415774,0.150774500763906,3.38587942993986));
#41628=CARTESIAN_POINT('Ctrl Pts',(15.7539746776403,0.598096785009218,3.79467766703735));
#41629=CARTESIAN_POINT('Ctrl Pts',(15.8016905137032,0.496177588678611,4.39202656178461));
#41630=CARTESIAN_POINT('Ctrl Pts',(15.849406349766,-0.0613891220090978,
4.62937143274106));
#41631=CARTESIAN_POINT('Ctrl Pts',(15.8971221858288,-0.562581257362808,
4.28875483288714));
#41632=CARTESIAN_POINT('Ctrl Pts',(15.9448380218917,-0.547146367654922,
3.68297022692873));
#41633=CARTESIAN_POINT('Ctrl Pts',(15.9925538579545,-0.0292585496004989,
3.36831893971177));
#41634=CARTESIAN_POINT('Ctrl Pts',(16.0402696940173,0.515497844752703,3.63375008981994));
#41635=CARTESIAN_POINT('Ctrl Pts',(16.0879855300802,0.586864636315616,4.23551416792571));
#41636=CARTESIAN_POINT('Ctrl Pts',(16.135701366143,0.119304602276749,4.62100196177401));
#41637=CARTESIAN_POINT('Ctrl Pts',(16.1834172022059,-0.457814683770117,
4.43621409878185));
#41638=CARTESIAN_POINT('Ctrl Pts',(16.2311330382687,-0.614515701326505,
3.85084411686165));
#41639=CARTESIAN_POINT('Ctrl Pts',(16.2788488743316,-0.206897494815317,
3.40244627748567));
#41640=CARTESIAN_POINT('Ctrl Pts',(16.3265647103943,0.390717864711932,3.50279121604045));
#41641=CARTESIAN_POINT('Ctrl Pts',(16.3742805464572,0.629530997107116,4.05973063144581));
#41642=CARTESIAN_POINT('Ctrl Pts',(16.42199638252,0.290236128279341,4.56181848892059));
#41643=CARTESIAN_POINT('Ctrl Pts',(16.4697122185829,-0.315587043004215,
4.54797978333095));
#41644=CARTESIAN_POINT('Ctrl Pts',(16.5174280546457,-0.631601776766168,
4.03092281095576));
#41645=CARTESIAN_POINT('Ctrl Pts',(16.5651438907086,-0.367606880481235,
3.48546894547127));
#41646=CARTESIAN_POINT('Ctrl Pts',(16.6128597267714,0.233967070508539,3.41251686443844));
#41647=CARTESIAN_POINT('Ctrl Pts',(16.6605755628343,0.620685460604191,3.87905958638177));
#41648=CARTESIAN_POINT('Ctrl Pts',(16.7082913988971,0.437418841753611,4.45666375105816));
#41649=CARTESIAN_POINT('Ctrl Pts',(16.7560072349599,-0.147536230033309,
4.61490656646286));
#41650=CARTESIAN_POINT('Ctrl Pts',(16.8037230710227,-0.597006511643959,
4.20847122033102));
#41651=CARTESIAN_POINT('Ctrl Pts',(16.8514389070856,-0.498236527486006,
3.61059354482716));
#41652=CARTESIAN_POINT('Ctrl Pts',(16.8991547431484,0.058071726216741,3.37031380889701));
#41653=CARTESIAN_POINT('Ctrl Pts',(16.9468705792113,0.561051820186282,3.70828459122417));
#41654=CARTESIAN_POINT('Ctrl Pts',(16.9945864152741,0.548809394786867,4.31414212204871));
#41655=CARTESIAN_POINT('Ctrl Pts',(17.0423022513369,0.0325868576366809,
4.63151810849805));
#41656=CARTESIAN_POINT('Ctrl Pts',(17.0900180873998,-0.513560692294518,
4.3689612987585));
#41657=CARTESIAN_POINT('Ctrl Pts',(17.1377339234626,-0.588097556344686,
3.76758165116972));
#41658=CARTESIAN_POINT('Ctrl Pts',(17.1854497595255,-0.122575385359494,
3.37963534952775));
#41659=CARTESIAN_POINT('Ctrl Pts',(17.2331655955883,0.455509648066065,3.56137945195155));
#41660=CARTESIAN_POINT('Ctrl Pts',(17.2808814316511,0.615293162755707,4.14591555269289));
#41661=CARTESIAN_POINT('Ctrl Pts',(17.328597267714,0.210043498584534,4.59645515619697));
#41662=CARTESIAN_POINT('Ctrl Pts',(17.3763131037768,-0.388092342271454,
4.49926081212312));
#41663=CARTESIAN_POINT('Ctrl Pts',(17.4240289398397,-0.629837013651323,
3.94358758216158));
#41664=CARTESIAN_POINT('Ctrl Pts',(17.4717447759025,-0.293192664107019,
3.43971874351766));
#41665=CARTESIAN_POINT('Ctrl Pts',(17.5194606119653,0.312695020235776,3.45036480373676));
#41666=CARTESIAN_POINT('Ctrl Pts',(17.5671764480282,0.631430056064715,3.96574932190893));
#41667=CARTESIAN_POINT('Ctrl Pts',(17.614892284091,0.370313155609181,4.51258676478657));
#41668=CARTESIAN_POINT('Ctrl Pts',(17.6626081201539,-0.230868013642575,
4.58870789439952));
#41669=CARTESIAN_POINT('Ctrl Pts',(17.7103239562166,-0.620039533605355,
4.12420950615009));
#41670=CARTESIAN_POINT('Ctrl Pts',(17.7580397922796,-0.43981920932378,3.54564761719411));
#41671=CARTESIAN_POINT('Ctrl Pts',(17.8057556283423,0.144293862368219,3.38432451247882));
#41672=CARTESIAN_POINT('Ctrl Pts',(17.8534714644052,0.595899660001039,3.78838568133928));
#41673=CARTESIAN_POINT('Ctrl Pts',(17.901187300468,0.500281630760053,4.38677553513073));
#41674=CARTESIAN_POINT('Ctrl Pts',(17.9489031365309,-0.0547527178302441,
4.62998346370502));
#41675=CARTESIAN_POINT('Ctrl Pts',(17.9966189725937,-0.559506803158163,
4.29466788401745));
#41676=CARTESIAN_POINT('Ctrl Pts',(18.0443348086565,-0.550457182027191,
3.68875425238845));
#41677=CARTESIAN_POINT('Ctrl Pts',(18.0920506447194,-0.0359142607682062,
3.36866237992255));
#41678=CARTESIAN_POINT('Ctrl Pts',(18.1397664807822,0.511609278766163,3.62833755835171));
#41679=CARTESIAN_POINT('Ctrl Pts',(18.187482316845,0.589314145488933,4.22931607570827));
#41680=CARTESIAN_POINT('Ctrl Pts',(18.2351981529079,0.12584276464555,4.61971011226051));
#41681=CARTESIAN_POINT('Ctrl Pts',(18.2829139889707,-0.453191963311679,
4.44101481725822));
#41682=CARTESIAN_POINT('Ctrl Pts',(18.3306298250336,-0.616053538105107,
3.85732882968247));
#41683=CARTESIAN_POINT('Ctrl Pts',(18.3783456610964,-0.213183669654489,
3.40465997308746));
#41684=CARTESIAN_POINT('Ctrl Pts',(18.4260614971592,0.385456042892229,3.49870102369));
#41685=CARTESIAN_POINT('Ctrl Pts',(18.4737773332221,0.630125540247444,4.05309263771424));
#41686=CARTESIAN_POINT('Ctrl Pts',(18.5214931692849,0.296141058265729,4.55872846559028));
#41687=CARTESIAN_POINT('Ctrl Pts',(18.5692090053478,-0.309794314237323,
4.55127534637221));
#41688=CARTESIAN_POINT('Ctrl Pts',(18.6169248414106,-0.631240801177943,
4.0375775941191));
#41689=CARTESIAN_POINT('Ctrl Pts',(18.6646406774734,-0.373009147508776,
3.4893717589807));
#41690=CARTESIAN_POINT('Ctrl Pts',(18.7123565135363,0.227762545801372,3.41008369459593));
#41691=CARTESIAN_POINT('Ctrl Pts',(18.7600723495991,0.619376388724522,3.87252485049244));
#41692=CARTESIAN_POINT('Ctrl Pts',(18.8077881856619,0.442207363551868,4.45202839763978));
#41693=CARTESIAN_POINT('Ctrl Pts',(18.8555040217248,-0.141047487806633,
4.61642731188217));
#41694=CARTESIAN_POINT('Ctrl Pts',(18.9032198577876,-0.594776260815313,
4.21475154067248));
#41695=CARTESIAN_POINT('Ctrl Pts',(18.9509356938505,-0.502312841712761,
3.615866125281));
#41696=CARTESIAN_POINT('Ctrl Pts',(18.9986515299133,0.0514321890198641,
3.36973675771293));
#41697=CARTESIAN_POINT('Ctrl Pts',(19.0463673659762,0.557946249173174,3.70238782336559));
#41698=CARTESIAN_POINT('Ctrl Pts',(19.0940832020389,0.552089683635207,4.30834073020757));
#41699=CARTESIAN_POINT('Ctrl Pts',(19.1417990381018,0.0392406665648073,
4.63113960000379));
#41700=CARTESIAN_POINT('Ctrl Pts',(19.1895148741646,-0.509643658296843,
4.3743532639067));
#41701=CARTESIAN_POINT('Ctrl Pts',(19.2372307102275,-0.590514370077448,
3.77379256516987));
#41702=CARTESIAN_POINT('Ctrl Pts',(19.2849465462903,-0.129106649190522,
3.38096163491845));
#41703=CARTESIAN_POINT('Ctrl Pts',(19.3326623823532,0.450861693465423,3.55660315963506));
#41704=CARTESIAN_POINT('Ctrl Pts',(19.380378218416,0.616796807017627,4.1394228269368));
#41705=CARTESIAN_POINT('Ctrl Pts',(19.4280940544789,0.216317919394901,4.59420836405745));
#41706=CARTESIAN_POINT('Ctrl Pts',(19.4758098905416,-0.382809037079938,
4.50332322288615));
#41707=CARTESIAN_POINT('Ctrl Pts',(19.5235257266046,-0.630396573984801,
3.95022861114352));
#41708=CARTESIAN_POINT('Ctrl Pts',(19.5712415626673,-0.299081219248977,
3.44283985120298));
#41709=CARTESIAN_POINT('Ctrl Pts',(19.6189573987302,0.306884987370396,3.44709979193512));
#41710=CARTESIAN_POINT('Ctrl Pts',(19.666673234793,0.631034051704256,3.95909657101937));
#41711=CARTESIAN_POINT('Ctrl Pts',(19.7143890708559,0.375694716468479,4.50865546647685));
#41712=CARTESIAN_POINT('Ctrl Pts',(19.7621049069187,-0.224650630777236,
4.59110846933868));
#41713=CARTESIAN_POINT('Ctrl Pts',(19.8098207429815,-0.618696275574682,
4.13073699938377));
#41714=CARTESIAN_POINT('Ctrl Pts',(19.8575365790444,-0.44458280157215,3.55030861879767));
#41715=CARTESIAN_POINT('Ctrl Pts',(19.9052524151072,0.13779637220375,3.3828370770856));
#41716=CARTESIAN_POINT('Ctrl Pts',(19.9529682511701,0.593637901716091,3.7821189081517));
#41717=CARTESIAN_POINT('Ctrl Pts',(20.0006840872329,0.504327165075627,4.38147832337345));
#41718=CARTESIAN_POINT('Ctrl Pts',(20.0483999232957,-0.0481046828163007,
4.63053160650705));
#41719=CARTESIAN_POINT('Ctrl Pts',(20.0961157593586,-0.556380679578279,
4.30053671048834));
#41720=CARTESIAN_POINT('Ctrl Pts',(20.1438315954214,-0.553687069357429,
3.69459455385474));
#41721=CARTESIAN_POINT('Ctrl Pts',(20.1915474314843,-0.0426033430871586,
3.36903495876776));
#41722=CARTESIAN_POINT('Ctrl Pts',(20.2392632675471,0.507734449822709,3.62304374442814));
#41723=CARTESIAN_POINT('Ctrl Pts',(20.2869791036099,0.591564791291533,4.22294595084339));
#41724=CARTESIAN_POINT('Ctrl Pts',(20.3346949396728,0.132620199007312,4.618629012875));
#41725=CARTESIAN_POINT('Ctrl Pts',(20.3824107757356,-0.449008129734859,
4.44521533979349));
#41726=CARTESIAN_POINT('Ctrl Pts',(20.4221739724547,-0.588594799935545,
3.96175478680276));
#41727=CARTESIAN_POINT('Ctrl Pts',(20.4539845298298,-0.419131055782338,
3.63395025773895));
#41728=CARTESIAN_POINT('Ctrl Pts',(20.4778424478613,-0.194099195253748,
3.47709810398663));
#41729=CARTESIAN_POINT('Ctrl Pts',(20.5017003658927,0.0810471032980313,
3.44846366347126));
#41730=CARTESIAN_POINT('Ctrl Pts',(20.5255582839241,0.334940048200093,3.55449674151986));
#41731=CARTESIAN_POINT('Ctrl Pts',(20.5494162019556,0.507694843328107,3.76957374638464));
#41732=CARTESIAN_POINT('Ctrl Pts',(20.5732741199869,0.555899439471162,4.04093981905292));
#41733=CARTESIAN_POINT('Ctrl Pts',(20.5971320380184,0.468386015874758,4.30232489481291));
#41734=CARTESIAN_POINT('Ctrl Pts',(20.6209899560498,0.266225827016684,4.48976745893774));
#41735=CARTESIAN_POINT('Ctrl Pts',(20.6448478740812,-0.000973650874560818,
4.55745692740964));
#41736=CARTESIAN_POINT('Ctrl Pts',(20.6687057921126,-0.267966914960919,
4.48882854939535));
#41737=CARTESIAN_POINT('Ctrl Pts',(20.6925637101441,-0.469418090387657,
4.30067062862012));
#41738=CARTESIAN_POINT('Ctrl Pts',(20.7164216281755,-0.556092695039732,
4.03898930289119));
#41739=CARTESIAN_POINT('Ctrl Pts',(20.7402795462069,-0.506782753954552,
3.7677746905255));
#41740=CARTESIAN_POINT('Ctrl Pts',(20.7641374642383,-0.333553132261349,
3.55334514249538));
#41741=CARTESIAN_POINT('Ctrl Pts',(20.7879953822697,-0.0787593560922578,
3.44813505886707));
#41742=CARTESIAN_POINT('Ctrl Pts',(20.8118533003012,0.19529252477751,3.47787088781106));
#41743=CARTESIAN_POINT('Ctrl Pts',(20.8357112183325,0.421590436108717,3.63528155911584));
#41744=CARTESIAN_POINT('Ctrl Pts',(20.859569136364,0.544797804677434,3.8818757964511));
#41745=CARTESIAN_POINT('Ctrl Pts',(20.8834270543954,0.534787374467886,4.15735463375504));
#41746=CARTESIAN_POINT('Ctrl Pts',(20.9072849724269,0.394006808563119,4.39435596913946));
#41747=CARTESIAN_POINT('Ctrl Pts',(20.9311428904582,0.156880874733563,4.53492653211281));
#41748=CARTESIAN_POINT('Ctrl Pts',(20.9550008084897,-0.118606721834374,
4.54469298471526));
#41749=CARTESIAN_POINT('Ctrl Pts',(20.9788587265211,-0.365091735913813,
4.42126716656144));
#41750=CARTESIAN_POINT('Ctrl Pts',(21.0027166445525,-0.522301880015273,
4.19483005048941));
#41751=CARTESIAN_POINT('Ctrl Pts',(21.0265745625839,-0.55179498493052,3.92075168033001));
#41752=CARTESIAN_POINT('Ctrl Pts',(21.0504324806153,-0.446359186657349,
3.66605168284066));
#41753=CARTESIAN_POINT('Ctrl Pts',(21.0742903986468,-0.231776408019839,
3.49301114555638));
#41754=CARTESIAN_POINT('Ctrl Pts',(21.0981483166782,0.0394820154987394,
3.44394319323497));
#41755=CARTESIAN_POINT('Ctrl Pts',(21.1220062347096,0.301086010940692,3.5308462768762));
#41756=CARTESIAN_POINT('Ctrl Pts',(21.145864152741,0.489066275193333,3.73247022529863));
#41757=CARTESIAN_POINT('Ctrl Pts',(21.1697220707724,0.557456513314207,3.9995124910074));
#41758=CARTESIAN_POINT('Ctrl Pts',(21.1935799888039,0.489533449092281,4.26667396594056));
#41759=CARTESIAN_POINT('Ctrl Pts',(21.2174379068352,0.30190612195814,4.46862639215028));
#41760=CARTESIAN_POINT('Ctrl Pts',(21.2412958248667,0.0404545242400231,
4.55598690035157));
#41761=CARTESIAN_POINT('Ctrl Pts',(21.2651537428981,-0.230889306609896,
4.50739346663836));
#41762=CARTESIAN_POINT('Ctrl Pts',(21.2890116609295,-0.445774412697373,
4.33472850921124));
#41763=CARTESIAN_POINT('Ctrl Pts',(21.312869578961,-0.551655532228011,4.08021331346062));
#41764=CARTESIAN_POINT('Ctrl Pts',(21.3367274969923,-0.522641847334507,
3.80608377760199));
#41765=CARTESIAN_POINT('Ctrl Pts',(21.3605854150238,-0.365827994289322,
3.57937204029158));
#41766=CARTESIAN_POINT('Ctrl Pts',(21.3844433330552,-0.119559231686077,
3.45551529680541));
#41767=CARTESIAN_POINT('Ctrl Pts',(21.4083012510867,0.155945019792583,3.46479989471587));
#41768=CARTESIAN_POINT('Ctrl Pts',(21.432159169118,0.393316466074861,3.60495549692644));
#41769=CARTESIAN_POINT('Ctrl Pts',(21.4560170871495,0.534511322676435,3.84171024093472));
#41770=CARTESIAN_POINT('Ctrl Pts',(21.4798750051809,0.545003601087511,4.11717114276091));
#41771=CARTESIAN_POINT('Ctrl Pts',(21.5037329232123,0.422227653432673,4.36398050850424));
#41772=CARTESIAN_POINT('Ctrl Pts',(21.5275908412437,0.196205543263173,4.52178672528827));
#41773=CARTESIAN_POINT('Ctrl Pts',(21.5514487592751,-0.0777941667658609,
4.5520018745543));
#41774=CARTESIAN_POINT('Ctrl Pts',(21.5753066773066,-0.332771083950078,
4.44723752926263));
#41775=CARTESIAN_POINT('Ctrl Pts',(21.5991645953379,-0.506376406606172,
4.23311142556056));
#41776=CARTESIAN_POINT('Ctrl Pts',(21.6230225133694,-0.556158904430687,
3.96198322848119));
#41777=CARTESIAN_POINT('Ctrl Pts',(21.6468804314008,-0.469945400657515,
3.70015116759423));
#41778=CARTESIAN_POINT('Ctrl Pts',(21.6707383494323,-0.268817445367881,
3.51164031394868));
#41779=CARTESIAN_POINT('Ctrl Pts',(21.6945962674636,-0.00195630224560004,
3.44254670619344));
#41780=CARTESIAN_POINT('Ctrl Pts',(21.7184541854951,0.26538321006433,3.50976561349676));
#41781=CARTESIAN_POINT('Ctrl Pts',(21.7423121035264,0.467829298620023,3.6968601820167));
#41782=CARTESIAN_POINT('Ctrl Pts',(21.766170021558,0.555878380248887,3.95808069339639));
#41783=CARTESIAN_POINT('Ctrl Pts',(21.7900279395893,0.508000056083844,4.22955161709966));
#41784=CARTESIAN_POINT('Ctrl Pts',(21.8138858576208,0.335901880562604,4.44489091756156));
#41785=CARTESIAN_POINT('Ctrl Pts',(21.8377437756521,0.0816665454602928,
4.55144227009437));
#41786=CARTESIAN_POINT('Ctrl Pts',(21.8616016936836,-0.192538484559094,
4.52315096660328));
#41787=CARTESIAN_POINT('Ctrl Pts',(21.885459611715,-0.419662610460766,4.36693500143146));
#41788=CARTESIAN_POINT('Ctrl Pts',(21.9093175297464,-0.544167796724789,
4.12099343330092));
#41789=CARTESIAN_POINT('Ctrl Pts',(21.9331754477779,-0.535609133856441,
3.84546567493331));
#41790=CARTESIAN_POINT('Ctrl Pts',(21.9570333658092,-0.396079448060293,
3.60772576847503));
#41791=CARTESIAN_POINT('Ctrl Pts',(21.9808912838407,-0.159697548225882,
3.46590759696012));
#41792=CARTESIAN_POINT('Ctrl Pts',(22.0047492018721,0.115734752223676,3.45468956637345));
#41793=CARTESIAN_POINT('Ctrl Pts',(22.0286071199035,0.362866753203085,3.5768147907664));
#41794=CARTESIAN_POINT('Ctrl Pts',(22.0524650379349,0.521267948732644,3.80242032615069));
#41795=CARTESIAN_POINT('Ctrl Pts',(22.0763229559664,0.552204931742854,4.07633947375325));
#41796=CARTESIAN_POINT('Ctrl Pts',(22.1001808739978,0.448112767182329,4.33159154057792));
#41797=CARTESIAN_POINT('Ctrl Pts',(22.1240387920292,0.23444482469764,4.5057604433585));
#41798=CARTESIAN_POINT('Ctrl Pts',(22.1478967100606,-0.0365512635718279,
4.55625714110116));
#41799=CARTESIAN_POINT('Ctrl Pts',(22.171754628092,-0.298609572266455,4.47073381570218));
#41800=CARTESIAN_POINT('Ctrl Pts',(22.1956125461234,-0.487649706571227,
4.2701032498363));
#41801=CARTESIAN_POINT('Ctrl Pts',(22.2194704641549,-0.557446204325542,
4.00342508191314));
#41802=CARTESIAN_POINT('Ctrl Pts',(22.2433283821863,-0.490931920559466,
3.73590938817905));
#41803=CARTESIAN_POINT('Ctrl Pts',(22.2671863002177,-0.304371409562025,
3.53297104269219));
#41804=CARTESIAN_POINT('Ctrl Pts',(22.2910442182491,-0.0433837978980346,
3.44423399893113));
#41805=CARTESIAN_POINT('Ctrl Pts',(22.3149021362806,0.228212333880327,3.49139688109763));
#41806=CARTESIAN_POINT('Ctrl Pts',(22.3387600543119,0.444004334066149,3.66292708008725));
#41807=CARTESIAN_POINT('Ctrl Pts',(22.3626179723434,0.551225179343846,3.91688078933633));
#41808=CARTESIAN_POINT('Ctrl Pts',(22.3864758903748,0.523656454698273,4.19115941035881));
#41809=CARTESIAN_POINT('Ctrl Pts',(22.4103338084062,0.368039459933637,4.41869434725418));
#41810=CARTESIAN_POINT('Ctrl Pts',(22.4341917264376,0.122426797365049,4.54384711353805));
#41811=CARTESIAN_POINT('Ctrl Pts',(22.458049644469,-0.153122562087755,4.53601444212637));
#41812=CARTESIAN_POINT('Ctrl Pts',(22.4819075625005,-0.391229265084309,
4.39711164706476));
#41813=CARTESIAN_POINT('Ctrl Pts',(22.5057654805319,-0.533669791868601,
4.16110422172694));
#41814=CARTESIAN_POINT('Ctrl Pts',(22.5296233985633,-0.545613449745194,
3.88570245498666));
#41815=CARTESIAN_POINT('Ctrl Pts',(22.5534813165947,-0.424139885198736,
3.63824949626794));
#41816=CARTESIAN_POINT('Ctrl Pts',(22.5773392346261,-0.198952323217499,
3.47925449370713));
#41817=CARTESIAN_POINT('Ctrl Pts',(22.6011971526576,0.0748840438856019,
3.44759575567767));
#41818=CARTESIAN_POINT('Ctrl Pts',(22.625055070689,0.330410085854462,3.55101527375816));
#41819=CARTESIAN_POINT('Ctrl Pts',(22.6489129887204,0.505140231362423,3.7642230866287));
#41820=CARTESIAN_POINT('Ctrl Pts',(22.6727709067518,0.556352908954721,4.03508610068096));
#41821=CARTESIAN_POINT('Ctrl Pts',(22.6966288247833,0.471516332128332,4.29736710820476));
#41822=CARTESIAN_POINT('Ctrl Pts',(22.7204867428146,0.27139215166714,4.48693847894857));
#41823=CARTESIAN_POINT('Ctrl Pts',(22.7443446608461,0.00488440565515616,
4.55743119390072));
#41824=CARTESIAN_POINT('Ctrl Pts',(22.7682025788775,-0.262778018495442,
4.49163382183027));
#41825=CARTESIAN_POINT('Ctrl Pts',(22.7920604969089,-0.466262514422727,
4.30558517247789));
#41826=CARTESIAN_POINT('Ctrl Pts',(22.8079657755965,-0.525793678117208,
4.1317859159904));
#41827=CARTESIAN_POINT('Ctrl Pts',(22.8159184149403,-0.532958495437544,
4.04301651477895));
#41828=CARTESIAN_POINT('Ctrl Pts',(3.98408158505965,-0.251304309929533,
3.59658905474035));
#41829=CARTESIAN_POINT('Ctrl Pts',(3.99203422440346,-0.184112308377066,
3.5547318870523));
#41830=CARTESIAN_POINT('Ctrl Pts',(4.00793950309107,-0.0284797076443847,
3.50528009766423));
#41831=CARTESIAN_POINT('Ctrl Pts',(4.03179742112249,0.212077873916637,3.55216010213054));
#41832=CARTESIAN_POINT('Ctrl Pts',(4.05565533915392,0.400711255741927,3.70851080938071));
#41833=CARTESIAN_POINT('Ctrl Pts',(4.07951325718533,0.49139298320592,3.93615790384083));
#41834=CARTESIAN_POINT('Ctrl Pts',(4.10337117521676,0.461898357851897,4.17940600742409));
#41835=CARTESIAN_POINT('Ctrl Pts',(4.12722909324816,0.319466186301668,4.37878980142624));
#41836=CARTESIAN_POINT('Ctrl Pts',(4.15108701127959,0.0989109688445654,
4.48554634140719));
#41837=CARTESIAN_POINT('Ctrl Pts',(4.174944929311,-0.145828100556353,4.47357507321567));
#41838=CARTESIAN_POINT('Ctrl Pts',(4.19880284734243,-0.354909590370033,
4.34580100620849));
#41839=CARTESIAN_POINT('Ctrl Pts',(4.22266076537384,-0.477205295803391,
4.13346959398438));
#41840=CARTESIAN_POINT('Ctrl Pts',(4.24651868340526,-0.482811689970624,
3.88850100783657));
#41841=CARTESIAN_POINT('Ctrl Pts',(4.27037660143669,-0.370357271909554,
3.67079708031066));
#41842=CARTESIAN_POINT('Ctrl Pts',(4.2942345194681,-0.167340519784032,3.53359217153378));
#41843=CARTESIAN_POINT('Ctrl Pts',(4.31809243749953,0.0765956044913427,
3.51043671457025));
#41844=CARTESIAN_POINT('Ctrl Pts',(4.34195035553093,0.301801986965541,3.60699279882218));
#41845=CARTESIAN_POINT('Ctrl Pts',(4.36580827356237,0.453209578636439,3.79964985833574));
#41846=CARTESIAN_POINT('Ctrl Pts',(4.38966619159377,0.493795074712635,4.04129798000377));
#41847=CARTESIAN_POINT('Ctrl Pts',(4.4135241096252,0.413634228782107,4.27284762322724));
#41848=CARTESIAN_POINT('Ctrl Pts',(4.43738202765661,0.23232854437776,4.43767858897425));
#41849=CARTESIAN_POINT('Ctrl Pts',(4.46123994568804,-0.00578779637616802,
4.49548521832112));
#41850=CARTESIAN_POINT('Ctrl Pts',(4.48509786371945,-0.242488863923451,
4.43213221465579));
#41851=CARTESIAN_POINT('Ctrl Pts',(4.50895578175088,-0.419894798625899,
4.26311111366653));
#41852=CARTESIAN_POINT('Ctrl Pts',(4.53281369978229,-0.494625017545811,
4.02975217827461));
#41853=CARTESIAN_POINT('Ctrl Pts',(4.55667161781372,-0.448405946262215,
3.78911802491887));
#41854=CARTESIAN_POINT('Ctrl Pts',(4.58052953584513,-0.292539406836986,
3.60005025874973));
#41855=CARTESIAN_POINT('Ctrl Pts',(4.60438745387655,-0.0651390137990107,
3.50878109874461));
#41856=CARTESIAN_POINT('Ctrl Pts',(4.62824537190797,0.178189642449287,3.53762834062211));
#41857=CARTESIAN_POINT('Ctrl Pts',(4.65210328993938,0.377946077338085,3.67953804797316));
#41858=CARTESIAN_POINT('Ctrl Pts',(4.67596120797081,0.485284401269169,3.89980943180067));
#41859=CARTESIAN_POINT('Ctrl Pts',(4.69981912600222,0.473957470210434,4.14458013869048));
#41860=CARTESIAN_POINT('Ctrl Pts',(4.72367704403364,0.34673502734182,4.35399706338589));
#41861=CARTESIAN_POINT('Ctrl Pts',(4.74753496206506,0.134726425416229,4.47685206339739));
#41862=CARTESIAN_POINT('Ctrl Pts',(4.77139288009648,-0.110226457398098,
4.48310374471865));
#41863=CARTESIAN_POINT('Ctrl Pts',(4.7952507981279,-0.328225968870003,4.37122340097448));
#41864=CARTESIAN_POINT('Ctrl Pts',(4.81910871615932,-0.465965290257402,
4.16856882376961));
#41865=CARTESIAN_POINT('Ctrl Pts',(4.84296663419074,-0.489763405537152,
3.92469457743051));
#41866=CARTESIAN_POINT('Ctrl Pts',(4.86682455222216,-0.393801027275785,
3.69923455818817));
#41867=CARTESIAN_POINT('Ctrl Pts',(4.89068247025357,-0.201543570920867,
3.54731988215497));
#41868=CARTESIAN_POINT('Ctrl Pts',(4.914540388285,0.039996778460842,3.50609782569371));
#41869=CARTESIAN_POINT('Ctrl Pts',(4.93839830631641,0.271756826018508,3.58564830447545));
#41870=CARTESIAN_POINT('Ctrl Pts',(4.96225622434784,0.437064927107334,3.76651905952651));
#41871=CARTESIAN_POINT('Ctrl Pts',(4.98611414237925,0.495498748108838,4.00448226441646));
#41872=CARTESIAN_POINT('Ctrl Pts',(5.00997206041068,0.432769628082826,4.24134943356216));
#41873=CARTESIAN_POINT('Ctrl Pts',(5.03382997844209,0.26421654558258,4.41920009197534));
#41874=CARTESIAN_POINT('Ctrl Pts',(5.05768789647352,0.031055320573195,4.49454490911931));
#41875=CARTESIAN_POINT('Ctrl Pts',(5.08154581450493,-0.209699776246285,
4.44896002485074));
#41876=CARTESIAN_POINT('Ctrl Pts',(5.10540373253635,-0.399177565666329,
4.29359218508065));
#41877=CARTESIAN_POINT('Ctrl Pts',(5.12926165056777,-0.491045566902382,
4.06643305876778));
#41878=CARTESIAN_POINT('Ctrl Pts',(5.15311956859918,-0.462839551218119,
3.823029239986));
#41879=CARTESIAN_POINT('Ctrl Pts',(5.17697748663061,-0.321456657764784,
3.62289959261435));
#41880=CARTESIAN_POINT('Ctrl Pts',(5.20083540466202,-0.101468855184408,
3.51498126685736));
#41881=CARTESIAN_POINT('Ctrl Pts',(5.22469332269345,0.143330846444675,3.52566323299877));
#41882=CARTESIAN_POINT('Ctrl Pts',(5.24855124072486,0.353082251864168,3.6523334593461));
#41883=CARTESIAN_POINT('Ctrl Pts',(5.27240915875629,0.476495428935435,3.86401762512973));
#41884=CARTESIAN_POINT('Ctrl Pts',(5.2962670767877,0.483392494157105,4.10895318565465));
#41885=CARTESIAN_POINT('Ctrl Pts',(5.32012499481913,0.372086927210194,4.32724672446184));
#41886=CARTESIAN_POINT('Ctrl Pts',(5.34398291285054,0.169795971115995,4.46551952511629));
#41887=CARTESIAN_POINT('Ctrl Pts',(5.36784083088196,-0.0740147250654609,
4.48996012138256));
#41888=CARTESIAN_POINT('Ctrl Pts',(5.39169874891337,-0.299726804847767,
4.39459212172504));
#41889=CARTESIAN_POINT('Ctrl Pts',(5.4155566669448,-0.452147516450583,4.20273559983216));
#41890=CARTESIAN_POINT('Ctrl Pts',(5.43941458497621,-0.494005844030112,
3.96130470137348));
#41891=CARTESIAN_POINT('Ctrl Pts',(5.46327250300764,-0.415066286295368,
3.72933585746768));
#41892=CARTESIAN_POINT('Ctrl Pts',(5.48713042103905,-0.234631715382576,
3.56355176915442));
#41893=CARTESIAN_POINT('Ctrl Pts',(5.51098833907048,0.00317670118048804,
3.50449116189365));
#41894=CARTESIAN_POINT('Ctrl Pts',(5.53484625710188,0.240208327774024,3.56659596294035));
#41895=CARTESIAN_POINT('Ctrl Pts',(5.55870417513332,0.418502475082003,3.73467985673571));
#41896=CARTESIAN_POINT('Ctrl Pts',(5.58256209316472,0.494461367456411,3.96764175273735));
#41897=CARTESIAN_POINT('Ctrl Pts',(5.60642001119615,0.449510986625754,4.20851612161082));
#41898=CARTESIAN_POINT('Ctrl Pts',(5.63027792922757,0.294642925140636,4.39840261889448));
#41899=CARTESIAN_POINT('Ctrl Pts',(5.65413584725899,0.0677266425295592,
4.49086882357174));
#41900=CARTESIAN_POINT('Ctrl Pts',(5.6779937652904,-0.17575064898472,4.46330422991997));
#41901=CARTESIAN_POINT('Ctrl Pts',(5.70185168332183,-0.376252119531055,
4.32244913183746));
#41902=CARTESIAN_POINT('Ctrl Pts',(5.72570960135325,-0.48474969783608,4.10274643779879));
#41903=CARTESIAN_POINT('Ctrl Pts',(5.74956751938466,-0.474712770918799,
3.85791944074229));
#41904=CARTESIAN_POINT('Ctrl Pts',(5.77342543741608,-0.348595640189148,
3.64783501103505));
#41905=CARTESIAN_POINT('Ctrl Pts',(5.7972833554475,-0.13723738064616,3.52386451312966));
#41906=CARTESIAN_POINT('Ctrl Pts',(5.82114127347893,0.1076791581852,3.5163221129105));
#41907=CARTESIAN_POINT('Ctrl Pts',(5.84499919151033,0.326265206982528,3.62705212841851));
#41908=CARTESIAN_POINT('Ctrl Pts',(5.86885710954176,0.465070530553655,3.82897806268729));
#41909=CARTESIAN_POINT('Ctrl Pts',(5.89271502757317,0.490153431381492,4.07272350923538));
#41910=CARTESIAN_POINT('Ctrl Pts',(5.9165729456046,0.395380485146506,4.29868609559117));
#41911=CARTESIAN_POINT('Ctrl Pts',(5.94043086363601,0.203926205561759,4.45161176009809));
#41912=CARTESIAN_POINT('Ctrl Pts',(5.96428878166744,-0.0373935204432717,
4.49410611450448));
#41913=CARTESIAN_POINT('Ctrl Pts',(5.98814669969885,-0.26956963613406,4.41577793841189));
#41914=CARTESIAN_POINT('Ctrl Pts',(6.01200461773027,-0.435828398698505,
4.23578096933615));
#41915=CARTESIAN_POINT('Ctrl Pts',(6.0358625357617,-0.495515688199628,3.99812868033461));
#41916=CARTESIAN_POINT('Ctrl Pts',(6.0597204537931,-0.434035059498629,3.76093483037113));
#41917=CARTESIAN_POINT('Ctrl Pts',(6.08357837182454,-0.266422612259865,
3.58219732064663));
#41918=CARTESIAN_POINT('Ctrl Pts',(6.10743628985594,-0.0336596025775484,
3.50562697870369));
#41919=CARTESIAN_POINT('Ctrl Pts',(6.13129420788738,0.207328476491996,3.54993858195554));
#41920=CARTESIAN_POINT('Ctrl Pts',(6.15515212591877,0.397629707835022,3.70431327123879));
#41921=CARTESIAN_POINT('Ctrl Pts',(6.17901004395022,0.490679606253205,3.93097100878581));
#41922=CARTESIAN_POINT('Ctrl Pts',(6.20286796198161,0.463782811036945,4.17454675550933));
#41923=CARTESIAN_POINT('Ctrl Pts',(6.22672588001306,0.323407044622774,4.3753682944706));
#41924=CARTESIAN_POINT('Ctrl Pts',(6.25058379804445,0.104084330837213,4.48453946106473));
#41925=CARTESIAN_POINT('Ctrl Pts',(6.27444171607588,-0.140944443623038,
4.4749681472433));
#41926=CARTESIAN_POINT('Ctrl Pts',(6.29829963410731,-0.351028389709017,
4.349743491311));
#41927=CARTESIAN_POINT('Ctrl Pts',(6.32215755213872,-0.476177279109797,
4.13807688197341));
#41928=CARTESIAN_POINT('Ctrl Pts',(6.34601547017014,-0.483231738207782,
3.89435343878414));
#41929=CARTESIAN_POINT('Ctrl Pts',(6.37782602754537,-0.338784024988664,
3.5998542259592));
#41930=CARTESIAN_POINT('Ctrl Pts',(6.41758922426439,0.0803770223010952,
3.44371490521648));
#41931=CARTESIAN_POINT('Ctrl Pts',(6.46530506032724,0.512014121509362,3.7673575683149));
#41932=CARTESIAN_POINT('Ctrl Pts',(6.51302089639006,0.472271980317209,4.30452828893312));
#41933=CARTESIAN_POINT('Ctrl Pts',(6.56073673245292,-0.000548856210248058,
4.56210751581942));
#41934=CARTESIAN_POINT('Ctrl Pts',(6.60845256851575,-0.473190198344468,
4.30346185287483));
#41935=CARTESIAN_POINT('Ctrl Pts',(6.65616840457859,-0.511122033036262,
3.76615996983968));
#41936=CARTESIAN_POINT('Ctrl Pts',(6.70388424064142,-0.0797735308749388,
3.44358772816382));
#41937=CARTESIAN_POINT('Ctrl Pts',(6.75160007670426,0.424880365184703,3.63198234005898));
#41938=CARTESIAN_POINT('Ctrl Pts',(6.7993159127671,0.539334593204737,4.15833063512042));
#41939=CARTESIAN_POINT('Ctrl Pts',(6.84703174882994,0.158523065679302,4.53928284691909));
#41940=CARTESIAN_POINT('Ctrl Pts',(6.89474758489278,-0.367869781963911,
4.42500259414721));
#41941=CARTESIAN_POINT('Ctrl Pts',(6.94246342095561,-0.556438361909488,
3.92043630538129));
#41942=CARTESIAN_POINT('Ctrl Pts',(6.99017925701846,-0.234023037562683,
3.48893437735136));
#41943=CARTESIAN_POINT('Ctrl Pts',(7.03789509308128,0.303300305128555,3.52675198254107));
#41944=CARTESIAN_POINT('Ctrl Pts',(7.08561092914413,0.562097748282813,3.99916046672433));
#41945=CARTESIAN_POINT('Ctrl Pts',(7.13332676520696,0.304712478085684,4.47233993757656));
#41946=CARTESIAN_POINT('Ctrl Pts',(7.18104260126981,-0.232495107101315,
4.51176235979777));
#41947=CARTESIAN_POINT('Ctrl Pts',(7.22875843733264,-0.556198774489988,
4.08122554105153));
#41948=CARTESIAN_POINT('Ctrl Pts',(7.27647427339549,-0.369136593294786,
3.57609805363465));
#41949=CARTESIAN_POINT('Ctrl Pts',(7.32419010945832,0.156909424853758,3.46024624852207));
#41950=CARTESIAN_POINT('Ctrl Pts',(7.37190594552116,0.538863091386428,3.84005861730642));
#41951=CARTESIAN_POINT('Ctrl Pts',(7.41962178158399,0.425970496197337,4.36674761950234));
#41952=CARTESIAN_POINT('Ctrl Pts',(7.46733761764684,-0.0780973635293338,
4.55664663921719));
#41953=CARTESIAN_POINT('Ctrl Pts',(7.51505345370967,-0.510447210801067,
4.2353684852172));
#41954=CARTESIAN_POINT('Ctrl Pts',(7.56276928977251,-0.474045531130633,
3.69794782953315));
#41955=CARTESIAN_POINT('Ctrl Pts',(7.61048512583535,-0.00232054557778912,
3.43790632971152));
#41956=CARTESIAN_POINT('Ctrl Pts',(7.65820096189818,0.471535432411473,3.69404409621074));
#41957=CARTESIAN_POINT('Ctrl Pts',(7.70591679796103,0.512373167457076,4.23114587691112));
#41958=CARTESIAN_POINT('Ctrl Pts',(7.75363263402387,0.0826907388754792,
4.55598284219971));
#41959=CARTESIAN_POINT('Ctrl Pts',(7.80134847008669,-0.422927867535356,
4.3702522086048));
#41960=CARTESIAN_POINT('Ctrl Pts',(7.84906430614955,-0.540165305628305,
3.84451327478339));
#41961=CARTESIAN_POINT('Ctrl Pts',(7.89678014221237,-0.161360632039799,
3.46156019320034));
#41962=CARTESIAN_POINT('Ctrl Pts',(7.94449597827521,0.365623992797271,3.57306467116217));
#41963=CARTESIAN_POINT('Ctrl Pts',(7.99221181433806,0.556850479203549,4.07663043084052));
#41964=CARTESIAN_POINT('Ctrl Pts',(8.03992765040089,0.236712602309549,4.50982528676712));
#41965=CARTESIAN_POINT('Ctrl Pts',(8.08764348646373,-0.300802099575971,
4.47483973718518));
#41966=CARTESIAN_POINT('Ctrl Pts',(8.13535932252656,-0.562085604986122,
4.00380155059756));
#41967=CARTESIAN_POINT('Ctrl Pts',(8.18307515858941,-0.307197250538534,
3.52927234160183));
#41968=CARTESIAN_POINT('Ctrl Pts',(8.23079099465223,0.229795065915734,3.48701958438918));
#41969=CARTESIAN_POINT('Ctrl Pts',(8.27850683071509,0.555763037488074,3.91584463605021));
#41970=CARTESIAN_POINT('Ctrl Pts',(8.32622266677791,0.371365260221553,4.42195085332305));
#41971=CARTESIAN_POINT('Ctrl Pts',(8.37393850284076,-0.154062949695418,
4.54057310944092));
#41972=CARTESIAN_POINT('Ctrl Pts',(8.4216543389036,-0.538012782343907,4.16277876137275));
#41973=CARTESIAN_POINT('Ctrl Pts',(8.46937017496643,-0.427897198575242,
3.6355021720628));
#41974=CARTESIAN_POINT('Ctrl Pts',(8.51708601102927,0.0751629666897603,
3.44294954666756));
#41975=CARTESIAN_POINT('Ctrl Pts',(8.56480184709211,0.50919982311266,3.76194492389047));
#41976=CARTESIAN_POINT('Ctrl Pts',(8.61251768315494,0.475630646924824,4.29954994045293));
#41977=CARTESIAN_POINT('Ctrl Pts',(8.66023351921779,0.00528252914771292,
4.56207363752918));
#41978=CARTESIAN_POINT('Ctrl Pts',(8.70794935528062,-0.469916616427902,
4.30843646464781));
#41979=CARTESIAN_POINT('Ctrl Pts',(8.75566519134346,-0.513584102541225,
3.7715573403753));
#41980=CARTESIAN_POINT('Ctrl Pts',(8.8033810274063,-0.0856194047837525,
3.44446062547832));
#41981=CARTESIAN_POINT('Ctrl Pts',(8.85109686346913,0.420970909810523,3.6275242662766));
#41982=CARTESIAN_POINT('Ctrl Pts',(8.89881269953199,0.540977160455745,4.15263810462895));
#41983=CARTESIAN_POINT('Ctrl Pts',(8.9465285355948,0.1641957606509,4.5375820228614));
#41984=CARTESIAN_POINT('Ctrl Pts',(8.99424437165766,-0.363369132636193,
4.42885609773758));
#41985=CARTESIAN_POINT('Ctrl Pts',(9.04196020772048,-0.557246560270691,
3.92630501926208));
#41986=CARTESIAN_POINT('Ctrl Pts',(9.08967604378333,-0.239395897268157,
3.49142917554125));
#41987=CARTESIAN_POINT('Ctrl Pts',(9.13739187984617,0.298295701775085,3.52358174528888));
#41988=CARTESIAN_POINT('Ctrl Pts',(9.18510771590899,0.562057768008922,3.99323652897485));
#41989=CARTESIAN_POINT('Ctrl Pts',(9.23282355197185,0.309673537509763,4.46910231217259));
#41990=CARTESIAN_POINT('Ctrl Pts',(9.28053938803466,-0.227088667424462,
4.51418422403538));
#41991=CARTESIAN_POINT('Ctrl Pts',(9.32825522409753,-0.555311854854516,
4.08708285122523));
#41992=CARTESIAN_POINT('Ctrl Pts',(9.37597106016035,-0.373583621400482,
3.58001195619306));
#41993=CARTESIAN_POINT('Ctrl Pts',(9.4236868962232,0.151212199908504,3.45862254413551));
#41994=CARTESIAN_POINT('Ctrl Pts',(9.47140273228603,0.537147531342748,3.83438837996121));
#41995=CARTESIAN_POINT('Ctrl Pts',(9.51911856834887,0.429812019667804,4.36223791473086));
#41996=CARTESIAN_POINT('Ctrl Pts',(9.5668344044117,-0.0722264831760907,
4.5574387986564));
#41997=CARTESIAN_POINT('Ctrl Pts',(9.61455024047456,-0.507938295172089,
4.24073505647735));
#41998=CARTESIAN_POINT('Ctrl Pts',(9.66226607653738,-0.477202555076283,
3.70296060775017));
#41999=CARTESIAN_POINT('Ctrl Pts',(9.70998191260023,-0.00824436594879979,
3.43796200346455));
#42000=CARTESIAN_POINT('Ctrl Pts',(9.75769774866306,0.46828475128534,3.68909153946361));
#42001=CARTESIAN_POINT('Ctrl Pts',(9.80541358472589,0.514780775927077,4.22573309871483));
#42002=CARTESIAN_POINT('Ctrl Pts',(9.85312942078874,0.0885456931146035,
4.55508048006603));
#42003=CARTESIAN_POINT('Ctrl Pts',(9.90084525685159,-0.419002262135622,
4.37468891556157));
#42004=CARTESIAN_POINT('Ctrl Pts',(9.9485610929144,-0.541773992888202,3.8502147545669));
#42005=CARTESIAN_POINT('Ctrl Pts',(9.99627692897727,-0.167026329707142,
3.46329068919569));
#42006=CARTESIAN_POINT('Ctrl Pts',(10.0439927650401,0.361104182074418,3.56923504227033));
#42007=CARTESIAN_POINT('Ctrl Pts',(10.0917086011029,0.557627167155001,4.07075748419897));
#42008=CARTESIAN_POINT('Ctrl Pts',(10.1394244371657,0.242072544440304,4.50730223964386));
#42009=CARTESIAN_POINT('Ctrl Pts',(10.1871402732286,-0.295781020598791,
4.47798354257549));
#42010=CARTESIAN_POINT('Ctrl Pts',(10.2348561092914,-0.56201432324602,4.00972520363789));
#42011=CARTESIAN_POINT('Ctrl Pts',(10.2825719453543,-0.312141225154507,
3.53253606055812));
#42012=CARTESIAN_POINT('Ctrl Pts',(10.3302877814171,0.224375962906492,3.48462624592509));
#42013=CARTESIAN_POINT('Ctrl Pts',(10.37800361748,0.554845251762499,3.90999207970357));
#42014=CARTESIAN_POINT('Ctrl Pts',(10.4257194535428,0.375791608533427,4.41801357164013));
#42015=CARTESIAN_POINT('Ctrl Pts',(10.4734352896056,-0.148357251109035,
4.54216676877402));
#42016=CARTESIAN_POINT('Ctrl Pts',(10.5211511256685,-0.536267364288337,
4.16843987983467));
#42017=CARTESIAN_POINT('Ctrl Pts',(10.5688669617313,-0.431714905307627,
3.64003205746247));
#42018=CARTESIAN_POINT('Ctrl Pts',(10.6165827977942,0.0692879940047382,
3.44218833554121));
#42019=CARTESIAN_POINT('Ctrl Pts',(10.664298633857,0.50666266228973,3.75659164812817));
#42020=CARTESIAN_POINT('Ctrl Pts',(10.7120144699198,0.478761211786921,4.29452059555793));
#42021=CARTESIAN_POINT('Ctrl Pts',(10.7597303059827,0.0112059738120427,
4.56198674830498));
#42022=CARTESIAN_POINT('Ctrl Pts',(10.8074461420455,-0.466639882340508,
4.31337182280594));
#42023=CARTESIAN_POINT('Ctrl Pts',(10.8551619781083,-0.515963154362253,
3.77698273057893));
#42024=CARTESIAN_POINT('Ctrl Pts',(10.9028778141712,-0.0914695226195351,
3.44539382842306));
#42025=CARTESIAN_POINT('Ctrl Pts',(10.950593650234,0.417021979184216,3.62310830733915));
#42026=CARTESIAN_POINT('Ctrl Pts',(10.9983094862969,0.542555780795161,4.14692822684982));
#42027=CARTESIAN_POINT('Ctrl Pts',(11.0460253223597,0.169852260608159,4.53582169486292));
#42028=CARTESIAN_POINT('Ctrl Pts',(11.0937411584225,-0.358829204008283,
4.43266185580689));
#42029=CARTESIAN_POINT('Ctrl Pts',(11.1414569944853,-0.55799228928692,3.93218197720501));
#42030=CARTESIAN_POINT('Ctrl Pts',(11.1891728305482,-0.244742469498405,
3.49398043245019));
#42031=CARTESIAN_POINT('Ctrl Pts',(11.236888666611,0.293258125877444,3.5204644426882));
#42032=CARTESIAN_POINT('Ctrl Pts',(11.2846045026739,0.561955271903759,3.98731333380864));
#42033=CARTESIAN_POINT('Ctrl Pts',(11.3323203387367,0.314600244947554,4.46581258570203));
#42034=CARTESIAN_POINT('Ctrl Pts',(11.3800361747996,-0.221657027690976,
4.51654897269734));
#42035=CARTESIAN_POINT('Ctrl Pts',(11.4277520108624,-0.554363241169119,
4.0929304899371));
#42036=CARTESIAN_POINT('Ctrl Pts',(11.4754678469252,-0.377989160306769,
3.58397250834823));
#42037=CARTESIAN_POINT('Ctrl Pts',(11.5231836829881,0.145498182576105,3.45705897374896));
#42038=CARTESIAN_POINT('Ctrl Pts',(11.5708995190509,0.535372305622036,3.82873653777755));
#42039=CARTESIAN_POINT('Ctrl Pts',(11.6186153551137,0.43360580265347,4.35768797439208));
#42040=CARTESIAN_POINT('Ctrl Pts',(11.6663311911766,-0.0663475807746441,
4.55816904038548));
#42041=CARTESIAN_POINT('Ctrl Pts',(11.7140470272394,-0.505372959888646,
4.24607488805821));
#42042=CARTESIAN_POINT('Ctrl Pts',(11.7617628633023,-0.480306573774387,
3.70800637967828));
#42043=CARTESIAN_POINT('Ctrl Pts',(11.8094786993651,-0.0141672704965164,
3.43808010573911));
#42044=CARTESIAN_POINT('Ctrl Pts',(11.8571945354279,0.464982055269784,3.68417351694868));
#42045=CARTESIAN_POINT('Ctrl Pts',(11.9049103714908,0.517131205013274,4.22029524715934));
#42046=CARTESIAN_POINT('Ctrl Pts',(11.9526262075536,0.0943908121067024,
4.55411646222552));
#42047=CARTESIAN_POINT('Ctrl Pts',(12.0003420436165,-0.415030115946784,
4.37908400385228));
#42048=CARTESIAN_POINT('Ctrl Pts',(12.0480578796793,-0.543322502467158,
3.85593287178435));
#42049=CARTESIAN_POINT('Ctrl Pts',(12.0957737157421,-0.172673474880652,
3.46508080031456));
#42050=CARTESIAN_POINT('Ctrl Pts',(12.143489551805,0.356544261611682,3.56545326070575));
#42051=CARTESIAN_POINT('Ctrl Pts',(12.1912053878678,0.558341916527368,4.06487667815191));
#42052=CARTESIAN_POINT('Ctrl Pts',(12.2389212239306,0.247405598301292,4.50472284379514));
#42053=CARTESIAN_POINT('Ctrl Pts',(12.2866370599935,-0.290727087669313,
4.48107425582212));
#42054=CARTESIAN_POINT('Ctrl Pts',(12.3343528960563,-0.56188061562194,4.01564777644873));
#42055=CARTESIAN_POINT('Ctrl Pts',(12.3820687321191,-0.317050528604376,
3.5358517031905));
#42056=CARTESIAN_POINT('Ctrl Pts',(12.429784568182,0.218931937280033,3.48229015273196));
#42057=CARTESIAN_POINT('Ctrl Pts',(12.4775004042448,0.553865836459325,3.90414952100961));
#42058=CARTESIAN_POINT('Ctrl Pts',(12.5252162403077,0.380176215696692,4.4140298589933));
#42059=CARTESIAN_POINT('Ctrl Pts',(12.5729320763705,-0.142635073703209,
4.54370020679522));
#42060=CARTESIAN_POINT('Ctrl Pts',(12.6206479124333,-0.53446238019874,4.17408228879405));
#42061=CARTESIAN_POINT('Ctrl Pts',(12.6683637484962,-0.435484659196984,
3.644601926393));
#42062=CARTESIAN_POINT('Ctrl Pts',(12.716079584559,0.0634053251381518,3.44148908348752));
#42063=CARTESIAN_POINT('Ctrl Pts',(12.7637954206219,0.504069223782589,3.75126540901054));
#42064=CARTESIAN_POINT('Ctrl Pts',(12.8115112566847,0.481838598125516,4.2894585367128));
#42065=CARTESIAN_POINT('Ctrl Pts',(12.8592270927475,0.0171281737699642,
4.56183743625962));
#42066=CARTESIAN_POINT('Ctrl Pts',(12.9069429288104,-0.463311316109371,
4.31827237310907));
#42067=CARTESIAN_POINT('Ctrl Pts',(12.9546587648732,-0.518284895444539,
3.78243289248252));
#42068=CARTESIAN_POINT('Ctrl Pts',(13.0023746009361,-0.0973094804548018,
3.44638863438952));
#42069=CARTESIAN_POINT('Ctrl Pts',(13.0500904369989,0.413026727735397,3.61873421174243));
#42070=CARTESIAN_POINT('Ctrl Pts',(13.0978062730617,0.544074136613086,4.14120202898048));
#42071=CARTESIAN_POINT('Ctrl Pts',(13.1455221091246,0.17548989418231,4.53400185033327));
#42072=CARTESIAN_POINT('Ctrl Pts',(13.1932379451874,-0.354249418335187,
4.4364195558504));
#42073=CARTESIAN_POINT('Ctrl Pts',(13.2409537812502,-0.558676039167545,
3.93806646805208));
#42074=CARTESIAN_POINT('Ctrl Pts',(13.2886696173131,-0.250061856896528,
3.49658789561142));
#42075=CARTESIAN_POINT('Ctrl Pts',(13.3363854533759,0.288187976258808,3.51740040462167));
#42076=CARTESIAN_POINT('Ctrl Pts',(13.3841012894388,0.56179035647369,3.9813915478171));
#42077=CARTESIAN_POINT('Ctrl Pts',(13.4318171255016,0.319492008083037,4.46247111897993));
#42078=CARTESIAN_POINT('Ctrl Pts',(13.4795329615644,-0.21620076734671,4.51885634555065));
#42079=CARTESIAN_POINT('Ctrl Pts',(13.5272487976273,-0.553353051445561,
4.09876780637113));
#42080=CARTESIAN_POINT('Ctrl Pts',(13.5749646336901,-0.382352713970831,
3.58797927086295));
#42081=CARTESIAN_POINT('Ctrl Pts',(13.6226804697529,0.139768003996038,3.45555571067516));
#42082=CARTESIAN_POINT('Ctrl Pts',(13.6703963058158,0.53353761328617,3.82310371872654));
#42083=CARTESIAN_POINT('Ctrl Pts',(13.7181121418786,0.437351422764197,4.35309830377052));
#42084=CARTESIAN_POINT('Ctrl Pts',(13.7658279779415,-0.0604613087987784,
4.55883728334624));
#42085=CARTESIAN_POINT('Ctrl Pts',(13.8135438140043,-0.502751490175015,
4.25138738680826));
#42086=CARTESIAN_POINT('Ctrl Pts',(13.8612596500671,-0.483357242297515,
3.71308458487209));
#42087=CARTESIAN_POINT('Ctrl Pts',(13.90897548613,-0.0200886014110514,3.43826062340902));
#42088=CARTESIAN_POINT('Ctrl Pts',(13.9566913221928,0.461627711254046,3.67929057494076));
#42089=CARTESIAN_POINT('Ctrl Pts',(14.0044071582557,0.519424193619207,4.21483292625321));
#42090=CARTESIAN_POINT('Ctrl Pts',(14.0521229943185,0.100225446615308,4.55309089575788));
#42091=CARTESIAN_POINT('Ctrl Pts',(14.0998388303813,-0.411011870182152,
4.38343698529073));
#42092=CARTESIAN_POINT('Ctrl Pts',(14.1475546664441,-0.544810662360815,
3.86166699129474));
#42093=CARTESIAN_POINT('Ctrl Pts',(14.195270502507,-0.178301440303968,3.46693032771971));
#42094=CARTESIAN_POINT('Ctrl Pts',(14.2429863385698,0.351944737904315,3.5617197465309));
#42095=CARTESIAN_POINT('Ctrl Pts',(14.2907021746327,0.558994647929194,4.05898866591129));
#42096=CARTESIAN_POINT('Ctrl Pts',(14.3384180106955,0.252711171522458,4.50208738572805));
#42097=CARTESIAN_POINT('Ctrl Pts',(14.3861338467583,-0.28564086215454,4.48411153362329));
#42098=CARTESIAN_POINT('Ctrl Pts',(14.4338496828212,-0.561684496965419,
4.02156861117883));
#42099=CARTESIAN_POINT('Ctrl Pts',(14.481565518884,-0.321924615586062,3.53921890121312));
#42100=CARTESIAN_POINT('Ctrl Pts',(14.5292813549469,0.213463593732893,3.48001156429194));
#42101=CARTESIAN_POINT('Ctrl Pts',(14.5769971910097,0.552824900367352,3.89831760893199));
#42102=CARTESIAN_POINT('Ctrl Pts',(14.6247130270725,0.384518594689996,4.4100001578745));
#42103=CARTESIAN_POINT('Ctrl Pts',(14.6724288631354,-0.136897053070264,
4.54517325317752));
#42104=CARTESIAN_POINT('Ctrl Pts',(14.7201446991982,-0.532598030564186,
4.17970536151887));
#42105=CARTESIAN_POINT('Ctrl Pts',(14.7678605352611,-0.439206041516937,
3.64921127125505));
#42106=CARTESIAN_POINT('Ctrl Pts',(14.8155763713239,0.0575156135089261,
3.44085186817608));
#42107=CARTESIAN_POINT('Ctrl Pts',(14.8632922073868,0.501419795658073,3.74596679815093));
#42108=CARTESIAN_POINT('Ctrl Pts',(14.9110080434496,0.484862464119148,4.284364326187));
#42109=CARTESIAN_POINT('Ctrl Pts',(14.9587238795124,0.0230484712116303,
4.56162571797798));
#42110=CARTESIAN_POINT('Ctrl Pts',(15.0064397155752,-0.459931287455839,
4.32313757122732));
#42111=CARTESIAN_POINT('Ctrl Pts',(15.0541555516381,-0.5205490679001,3.78790722070797));
#42112=CARTESIAN_POINT('Ctrl Pts',(15.1018713877009,-0.103138629614742,
3.44744493287938));
#42113=CARTESIAN_POINT('Ctrl Pts',(15.1495872237638,0.40898559923764,3.61440246534021));
#42114=CARTESIAN_POINT('Ctrl Pts',(15.1973030598266,0.545532059257757,4.13546014705983));
#42115=CARTESIAN_POINT('Ctrl Pts',(15.2450188958894,0.181108035171788,4.53212269141213));
#42116=CARTESIAN_POINT('Ctrl Pts',(15.2927347319523,-0.349630284317748,
4.44012878048063));
#42117=CARTESIAN_POINT('Ctrl Pts',(15.3404505680151,-0.559297733964875,
3.94395783818199));
#42118=CARTESIAN_POINT('Ctrl Pts',(15.3881664040779,-0.255353468610234,
3.49925127540033));
#42119=CARTESIAN_POINT('Ctrl Pts',(15.4358822401408,0.283085816087337,3.51438997142805));
#42120=CARTESIAN_POINT('Ctrl Pts',(15.4835980762036,0.561563040036739,3.97547182876414));
#42121=CARTESIAN_POINT('Ctrl Pts',(15.5313139122665,0.324348283562367,4.45907828316053));
#42122=CARTESIAN_POINT('Ctrl Pts',(15.5790297483293,-0.210720492447169,
4.52110608630326));
#42123=CARTESIAN_POINT('Ctrl Pts',(15.6267455843921,-0.552281397890927,
4.10459415214592));
#42124=CARTESIAN_POINT('Ctrl Pts',(15.674461420455,-0.386673797709831,3.59203179868507));
#42125=CARTESIAN_POINT('Ctrl Pts',(15.7221772565178,0.134022300649356,3.45411292188939));
#42126=CARTESIAN_POINT('Ctrl Pts',(15.7698930925807,0.531643658124066,3.81749054847505));
#42127=CARTESIAN_POINT('Ctrl Pts',(15.8176089286435,0.441048463954279,4.34846941266494));
#42128=CARTESIAN_POINT('Ctrl Pts',(15.8653247647064,-0.054568321067637,
4.5594434533135));
#42129=CARTESIAN_POINT('Ctrl Pts',(15.9130406007692,-0.500074177211609,
4.25667196264028));
#42130=CARTESIAN_POINT('Ctrl Pts',(15.960756436832,-0.486354221791887,3.71819465926869));
#42131=CARTESIAN_POINT('Ctrl Pts',(16.0084722728949,-0.0260077009790528,
3.4385035364232));
#42132=CARTESIAN_POINT('Ctrl Pts',(16.0561881089577,0.458222091822753,3.6744432558139));
#42133=CARTESIAN_POINT('Ctrl Pts',(16.1039039450206,0.52165948705058,4.2093467427251));
#42134=CARTESIAN_POINT('Ctrl Pts',(16.1516197810833,0.106048948556897,4.55200389457816));
#42135=CARTESIAN_POINT('Ctrl Pts',(16.1993356171462,-0.406947971169398,
4.38774737636841));
#42136=CARTESIAN_POINT('Ctrl Pts',(16.247051453209,-0.546238307271431,3.86741647617928));
#42137=CARTESIAN_POINT('Ctrl Pts',(16.2947672892719,-0.183909600849411,
3.46883906597446));
#42138=CARTESIAN_POINT('Ctrl Pts',(16.3424831253347,0.347306121845567,3.55803491444678));
#42139=CARTESIAN_POINT('Ctrl Pts',(16.3901989613975,0.559585288858183,4.05309410148958));
#42140=CARTESIAN_POINT('Ctrl Pts',(16.4379147974604,0.257988674785898,4.49939615817675));
#42141=CARTESIAN_POINT('Ctrl Pts',(16.4856306335232,-0.280522909008289,
4.4870950386126));
#42142=CARTESIAN_POINT('Ctrl Pts',(16.5333464695861,-0.561425989060384,
4.02748705016995));
#42143=CARTESIAN_POINT('Ctrl Pts',(16.5810623056489,-0.326762944709103,
3.54263728061361));
#42144=CARTESIAN_POINT('Ctrl Pts',(16.6287781417117,0.207971539662738,3.4777907336998));
#42145=CARTESIAN_POINT('Ctrl Pts',(16.6764939777746,0.551722559108811,3.89249699125187));
#42146=CARTESIAN_POINT('Ctrl Pts',(16.7242098138374,0.388818263182495,4.40592491588375));
#42147=CARTESIAN_POINT('Ctrl Pts',(16.7719256499003,-0.131143826562283,
4.54658574430191));
#42148=CARTESIAN_POINT('Ctrl Pts',(16.8196414859631,-0.53067452246778,4.18530847342493));
#42149=CARTESIAN_POINT('Ctrl Pts',(16.8673573220259,-0.442878638914007,
3.65385958006445));
#42150=CARTESIAN_POINT('Ctrl Pts',(16.9150731580888,0.0516195133182915,
3.44027676038576));
#42151=CARTESIAN_POINT('Ctrl Pts',(16.9627889941516,0.498714672202087,3.74069640409388));
#42152=CARTESIAN_POINT('Ctrl Pts',(17.0105048302145,0.487832473891125,4.27923852982128));
#42153=CARTESIAN_POINT('Ctrl Pts',(17.0582206662773,0.0289662085384809,
4.56135161697672));
#42154=CARTESIAN_POINT('Ctrl Pts',(17.1059365023401,-0.456500171817451,
4.32796687675757));
#42155=CARTESIAN_POINT('Ctrl Pts',(17.1536523384029,-0.522755420235406,
3.79340510719289));
#42156=CARTESIAN_POINT('Ctrl Pts',(17.2013681744658,-0.108956322625149,
3.44856260656401));
#42157=CARTESIAN_POINT('Ctrl Pts',(17.2490840105286,0.404899042560309,3.61011354928233));
#42158=CARTESIAN_POINT('Ctrl Pts',(17.2967998465915,0.54692938679005,4.12970321886885));
#42159=CARTESIAN_POINT('Ctrl Pts',(17.3445156826543,0.186706059540143,4.53018442682757));
#42160=CARTESIAN_POINT('Ctrl Pts',(17.3922315187172,-0.344972315027459,
4.4437891176945));
#42161=CARTESIAN_POINT('Ctrl Pts',(17.43994735478,-0.559857304624004,3.94985543320929));
#42162=CARTESIAN_POINT('Ctrl Pts',(17.4876631908428,-0.260616716872392,
3.5019702759813));
#42163=CARTESIAN_POINT('Ctrl Pts',(17.5353790269057,0.277952212086773,3.51143347749201));
#42164=CARTESIAN_POINT('Ctrl Pts',(17.5830948629685,0.561273347842132,3.96955483418404));
#42165=CARTESIAN_POINT('Ctrl Pts',(17.6308106990313,0.329168531973526,4.45563445510394));
#42166=CARTESIAN_POINT('Ctrl Pts',(17.6785265350942,-0.205216811715269,
4.52329794506467));
#42167=CARTESIAN_POINT('Ctrl Pts',(17.726242371157,-0.551148399539408,4.11040888009862));
#42168=CARTESIAN_POINT('Ctrl Pts',(17.7739582072198,-0.390951931558304,
3.59612964167903));
#42169=CARTESIAN_POINT('Ctrl Pts',(17.8216740432827,0.128261710741471,3.45273076764982));
#42170=CARTESIAN_POINT('Ctrl Pts',(17.8693898793456,0.529690650507269,3.81189765050732));
#42171=CARTESIAN_POINT('Ctrl Pts',(17.9171057154083,0.44469651557395,4.34380181523062));
#42172=CARTESIAN_POINT('Ctrl Pts',(17.9648215514712,-0.0486692721463468,
4.55998748295674));
#42173=CARTESIAN_POINT('Ctrl Pts',(18.012537387534,-0.497341318381634,4.26192802856871));
#42174=CARTESIAN_POINT('Ctrl Pts',(18.0602532235969,-0.489297179367249,
3.72333603526529));
#42175=CARTESIAN_POINT('Ctrl Pts',(18.1079690596597,-0.0319239117350811,
3.43880881780002));
#42176=CARTESIAN_POINT('Ctrl Pts',(18.1556848957225,0.454765575255941,3.66963209798526));
#42177=CARTESIAN_POINT('Ctrl Pts',(18.2034007317854,0.523836837021606,4.20383730595423));
#42178=CARTESIAN_POINT('Ctrl Pts',(18.2511165678483,0.111860671084556,4.5508555794253));
#42179=CARTESIAN_POINT('Ctrl Pts',(18.298832403911,-0.402838870307115,4.39201469830757));
#42180=CARTESIAN_POINT('Ctrl Pts',(18.346548239974,-0.547605278623001,3.87318068781251));
#42181=CARTESIAN_POINT('Ctrl Pts',(18.3942640760367,-0.189497333589109,
3.47080680306518));
#42182=CARTESIAN_POINT('Ctrl Pts',(18.4419799120997,0.342628928670919,3.55439917374707));
#42183=CARTESIAN_POINT('Ctrl Pts',(18.4896957481624,0.560113773708727,4.04719363962704));
#42184=CARTESIAN_POINT('Ctrl Pts',(18.5374115842253,0.263237521891608,4.49664946007004));
#42185=CARTESIAN_POINT('Ctrl Pts',(18.5851274202881,-0.275373796708506,
4.49002443939646));
#42186=CARTESIAN_POINT('Ctrl Pts',(18.632843256351,-0.561105120620647,4.03340243603));
#42187=CARTESIAN_POINT('Ctrl Pts',(18.6805590924138,-0.331564978554912,
3.54610646169455));
#42188=CARTESIAN_POINT('Ctrl Pts',(18.7282749284766,0.202456385100939,3.47562790763498));
#42189=CARTESIAN_POINT('Ctrl Pts',(18.7759907645394,0.550558935126376,3.8866883144956));
#42190=CARTESIAN_POINT('Ctrl Pts',(18.8237066006023,0.393074743587739,4.40180458567998));
#42191=CARTESIAN_POINT('Ctrl Pts',(18.8714224366651,-0.125376033221007,
4.54793752327491));
#42192=CARTESIAN_POINT('Ctrl Pts',(18.919138272728,-0.528692069562509,4.19089100214638));
#42193=CARTESIAN_POINT('Ctrl Pts',(18.9668541087908,-0.4465020434557,3.6585463365067));
#42194=CARTESIAN_POINT('Ctrl Pts',(19.0145699448537,0.0457176794812401,
3.43976382400136));
#42195=CARTESIAN_POINT('Ctrl Pts',(19.0622857809165,0.495954153879041,3.73545481224116));
#42196=CARTESIAN_POINT('Ctrl Pts',(19.1100016169793,0.490748297561716,4.27408171698104));
#42197=CARTESIAN_POINT('Ctrl Pts',(19.1577174530421,0.0348807284082936,
4.5610151636709));
#42198=CARTESIAN_POINT('Ctrl Pts',(19.205433289105,-0.453018350253257,4.33275975334162));
#42199=CARTESIAN_POINT('Ctrl Pts',(19.2531491251678,-0.524903707479367,
3.79892594114836));
#42200=CARTESIAN_POINT('Ctrl Pts',(19.3008649612307,-0.11476191309534,3.44974153150476));
#42201=CARTESIAN_POINT('Ctrl Pts',(19.3485807972935,0.400767511262006,3.60586793956989));
#42202=CARTESIAN_POINT('Ctrl Pts',(19.3962966333564,0.548265964675035,4.12393188459875));
#42203=CARTESIAN_POINT('Ctrl Pts',(19.4440124694192,0.192283344213529,4.52818727047755));
#42204=CARTESIAN_POINT('Ctrl Pts',(19.491728305482,-0.340276025447905,4.44740016355363));
#42205=CARTESIAN_POINT('Ctrl Pts',(19.5394441415448,-0.560354693525076,
3.95575859308266));
#42206=CARTESIAN_POINT('Ctrl Pts',(19.5871599776077,-0.265851008504119,
3.50474460473346));
#42207=CARTESIAN_POINT('Ctrl Pts',(19.6348758136705,0.272787718306182,3.5085312334714));
#42208=CARTESIAN_POINT('Ctrl Pts',(19.6825916497334,0.560921342594646,3.96364125479661));
#42209=CARTESIAN_POINT('Ctrl Pts',(19.7303074857962,0.33395216026474,4.45213995410186));
#42210=CARTESIAN_POINT('Ctrl Pts',(19.7780233218591,-0.199690227635008,
4.52543179776919));
#42211=CARTESIAN_POINT('Ctrl Pts',(19.8257391579219,-0.549954387748789,
4.11621111891367));
#42212=CARTESIAN_POINT('Ctrl Pts',(19.8734549939848,-0.395186252277308,
3.60027277035845));
#42213=CARTESIAN_POINT('Ctrl Pts',(19.9211708300475,0.122486141425193,3.45140859770427));
#42214=CARTESIAN_POINT('Ctrl Pts',(19.9688866661104,0.527680190865048,3.80632716374734));
#42215=CARTESIAN_POINT('Ctrl Pts',(20.0166025021732,0.448292560087992,4.33909316421112));
#42216=CARTESIAN_POINT('Ctrl Pts',(20.0643183382361,-0.0427598846646947,
4.56047472290141));
#42217=CARTESIAN_POINT('Ctrl Pts',(20.1120341742989,-0.49456253103916,4.26714478353561));
#42218=CARTESIAN_POINT('Ctrl Pts',(20.1597500103618,-0.492168201513856,
3.72852743457374));
#42219=CARTESIAN_POINT('Ctrl Pts',(20.2074658464246,-0.0378697858522375,
3.43914000028616));
#42220=CARTESIAN_POINT('Ctrl Pts',(20.2551816824874,0.451321269441671,3.66492646727415));
#42221=CARTESIAN_POINT('Ctrl Pts',(20.3028975185503,0.52583741886325,4.1981749506787));
#42222=CARTESIAN_POINT('Ctrl Pts',(20.3506133546131,0.117885080656874,4.54989459844945));
#42223=CARTESIAN_POINT('Ctrl Pts',(20.398329190676,-0.399119892637424,4.39574851066478));
#42224=CARTESIAN_POINT('Ctrl Pts',(20.438092387395,-0.523197416260526,3.96600412247733));
#42225=CARTESIAN_POINT('Ctrl Pts',(20.4699029447702,-0.3725623900923,3.67462118354637));
#42226=CARTESIAN_POINT('Ctrl Pts',(20.4937608628016,-0.172533290246804,
3.53519650363565));
#42227=CARTESIAN_POINT('Ctrl Pts',(20.5176187808331,0.0720421502968434,
3.50974356844941));
#42228=CARTESIAN_POINT('Ctrl Pts',(20.5414766988645,0.297725647320748,3.60399556061657));
#42229=CARTESIAN_POINT('Ctrl Pts',(20.5653346168959,0.451286063531533,3.79517586539437));
#42230=CARTESIAN_POINT('Ctrl Pts',(20.5891925349273,0.494134760388362,4.03639109206021));
#42231=CARTESIAN_POINT('Ctrl Pts',(20.6130504529587,0.416344747430809,4.26873428690612));
#42232=CARTESIAN_POINT('Ctrl Pts',(20.6369083709901,0.23664610161733,4.43535054865035));
#42233=CARTESIAN_POINT('Ctrl Pts',(20.6607662890216,-0.000865470816140784,
4.49551919950567));
#42234=CARTESIAN_POINT('Ctrl Pts',(20.684624207053,-0.238193741375527,4.43451595913869));
#42235=CARTESIAN_POINT('Ctrl Pts',(20.7084821250844,-0.417262150572256,
4.26726382233879));
#42236=CARTESIAN_POINT('Ctrl Pts',(20.7323400431158,-0.494306543785295,
4.03465729316116));
#42237=CARTESIAN_POINT('Ctrl Pts',(20.7561979611472,-0.45047531426282,3.79357669839993));
#42238=CARTESIAN_POINT('Ctrl Pts',(20.7800558791787,-0.296492828349621,
3.60297191305088));
#42239=CARTESIAN_POINT('Ctrl Pts',(20.80391379721,-0.0700085893017688,3.50945147432983));
#42240=CARTESIAN_POINT('Ctrl Pts',(20.8277717152415,0.173594031734132,3.53588342526713));
#42241=CARTESIAN_POINT('Ctrl Pts',(20.8516296332729,0.374748514455718,3.6758045671588));
#42242=CARTESIAN_POINT('Ctrl Pts',(20.8754875513043,0.484266602122282,3.89500029884494));
#42243=CARTESIAN_POINT('Ctrl Pts',(20.8993454693358,0.475368407265908,4.13987133054223));
#42244=CARTESIAN_POINT('Ctrl Pts',(20.9232033873671,0.350229638882089,4.35054000504804));
#42245=CARTESIAN_POINT('Ctrl Pts',(20.9470613053986,0.139450209771325,4.47549210343221));
#42246=CARTESIAN_POINT('Ctrl Pts',(20.97091922343,-0.105428607968738,4.48417342845956));
#42247=CARTESIAN_POINT('Ctrl Pts',(20.9947771414615,-0.324527251938122,
4.37446116262749));
#42248=CARTESIAN_POINT('Ctrl Pts',(21.0186350594928,-0.464270146732381,
4.17318294187641));
#42249=CARTESIAN_POINT('Ctrl Pts',(21.0424929775243,-0.490486342136868,
3.92955677471355));
#42250=CARTESIAN_POINT('Ctrl Pts',(21.0663508955557,-0.396765267394252,
3.7031558948169));
#42251=CARTESIAN_POINT('Ctrl Pts',(21.0902088135871,-0.206024276530194,
3.54934148458869));
#42252=CARTESIAN_POINT('Ctrl Pts',(21.1140667316185,0.0350952616297792,
3.50572535702762));
#42253=CARTESIAN_POINT('Ctrl Pts',(21.1379246496499,0.267633052506714,3.58297284346672));
#42254=CARTESIAN_POINT('Ctrl Pts',(21.1617825676814,0.434727271782411,3.76219482925797));
#42255=CARTESIAN_POINT('Ctrl Pts',(21.1856404857128,0.495518831419392,3.99956665698474));
#42256=CARTESIAN_POINT('Ctrl Pts',(21.2094984037442,0.43514253908843,4.23704444887943));
#42257=CARTESIAN_POINT('Ctrl Pts',(21.2333563217756,0.268362042918248,4.41655841606373));
#42258=CARTESIAN_POINT('Ctrl Pts',(21.257214239807,0.0359597172125542,4.49421250369607));
#42259=CARTESIAN_POINT('Ctrl Pts',(21.2810721578384,-0.205235738871087,
4.45101817209691));
#42260=CARTESIAN_POINT('Ctrl Pts',(21.3049300758699,-0.396245466293343,
4.29753761193144));
#42261=CARTESIAN_POINT('Ctrl Pts',(21.3287879939013,-0.490362383696085,
4.07130100088706));
#42262=CARTESIAN_POINT('Ctrl Pts',(21.3526459119327,-0.464572341082516,
3.82762935292545));
#42263=CARTESIAN_POINT('Ctrl Pts',(21.3765038299641,-0.325181706377507,
3.62610702345576));
#42264=CARTESIAN_POINT('Ctrl Pts',(21.4003617479955,-0.106275286691508,
3.51601171139131));
#42265=CARTESIAN_POINT('Ctrl Pts',(21.424219666027,0.138618335471326,3.52426471946798));
#42266=CARTESIAN_POINT('Ctrl Pts',(21.4480775840584,0.349615998723735,3.64884796240357));
#42267=CARTESIAN_POINT('Ctrl Pts',(21.4719355020898,0.475123026939619,3.85929744372095));
#42268=CARTESIAN_POINT('Ctrl Pts',(21.4957934201212,0.484449532977353,4.10415253270923));
#42269=CARTESIAN_POINT('Ctrl Pts',(21.5196513381527,0.375314932061802,4.32353949039209));
#42270=CARTESIAN_POINT('Ctrl Pts',(21.543509256184,0.174405606883644,4.4638122296353));
#42271=CARTESIAN_POINT('Ctrl Pts',(21.5673671742155,-0.069150639890911,
4.49067024474121));
#42272=CARTESIAN_POINT('Ctrl Pts',(21.5912250922469,-0.29579767158652,4.39754601941878));
#42273=CARTESIAN_POINT('Ctrl Pts',(21.6150830102783,-0.450114115212426,
4.20721096341231));
#42274=CARTESIAN_POINT('Ctrl Pts',(21.6389409283097,-0.494365396806572,
3.96620718253823));
#42275=CARTESIAN_POINT('Ctrl Pts',(21.6627988463412,-0.417730872638478,
3.73346666603139));
#42276=CARTESIAN_POINT('Ctrl Pts',(21.6866567643726,-0.238949771349764,
3.56590080990214));
#42277=CARTESIAN_POINT('Ctrl Pts',(21.710514682404,-0.00173894210493873,
3.50448403037633));
#42278=CARTESIAN_POINT('Ctrl Pts',(21.7343726004354,0.235897105852373,3.56423440300754));
#42279=CARTESIAN_POINT('Ctrl Pts',(21.7582305184669,0.415849885720624,3.73054133411992));
#42280=CARTESIAN_POINT('Ctrl Pts',(21.7820884364982,0.49411604100673,3.96273824894669));
#42281=CARTESIAN_POINT('Ctrl Pts',(21.8059463545297,0.451557364815975,4.20404667689569));
#42282=CARTESIAN_POINT('Ctrl Pts',(21.8298042725611,0.29858061275206,4.39546013422383));
#42283=CARTESIAN_POINT('Ctrl Pts',(21.8536621905925,0.0725927676976751,
4.49017281661646));
#42284=CARTESIAN_POINT('Ctrl Pts',(21.8775201086239,-0.171145986446082,
4.46502489330693));
#42285=CARTESIAN_POINT('Ctrl Pts',(21.9013780266554,-0.373034884980705,
4.32616571656009));
#42286=CARTESIAN_POINT('Ctrl Pts',(21.9252359446868,-0.483706592871294,
4.10755013753858));
#42287=CARTESIAN_POINT('Ctrl Pts',(21.9490938627182,-0.476098862901817,
3.86263562028194));
#42288=CARTESIAN_POINT('Ctrl Pts',(21.9729517807496,-0.352071992280181,
3.65131043559696));
#42289=CARTESIAN_POINT('Ctrl Pts',(21.996809698781,-0.141953929297546,3.52524934752154));
#42290=CARTESIAN_POINT('Ctrl Pts',(22.0206676168125,0.102875736145779,3.51527772592526));
#42291=CARTESIAN_POINT('Ctrl Pts',(22.0445255348438,0.322549481822576,3.62383390390986));
#42292=CARTESIAN_POINT('Ctrl Pts',(22.0683834528753,0.46335109312246,3.82437293894729));
#42293=CARTESIAN_POINT('Ctrl Pts',(22.0922413709067,0.490850740723195,4.06785757439707));
#42294=CARTESIAN_POINT('Ctrl Pts',(22.1160992889381,0.398324011712033,4.29474918450382));
#42295=CARTESIAN_POINT('Ctrl Pts',(22.1399572069695,0.208396211707814,4.44956659019228));
#42296=CARTESIAN_POINT('Ctrl Pts',(22.163815125001,-0.0324901386554863,
4.49445271863166));
#42297=CARTESIAN_POINT('Ctrl Pts',(22.1876730430324,-0.265431765108271,
4.41843168874211));
#42298=CARTESIAN_POINT('Ctrl Pts',(22.2115309610638,-0.433468094767725,
4.24009271310828));
#42299=CARTESIAN_POINT('Ctrl Pts',(22.2353888790952,-0.495509667838209,
4.00304452911861));
#42300=CARTESIAN_POINT('Ctrl Pts',(22.2592467971266,-0.436385629680506,
3.76525187484075));
#42301=CARTESIAN_POINT('Ctrl Pts',(22.2831047151581,-0.270553418215538,
3.58486153155103));
#42302=CARTESIAN_POINT('Ctrl Pts',(22.3069626331895,-0.0385635261649252,
3.50598385198694));
#42303=CARTESIAN_POINT('Ctrl Pts',(22.3308205512209,0.202856198284482,3.54790657725669));
#42304=CARTESIAN_POINT('Ctrl Pts',(22.3546784692523,0.394672056935096,3.70037845932536));
#42305=CARTESIAN_POINT('Ctrl Pts',(22.3785363872837,0.489979846308564,3.9261159693126));
#42306=CARTESIAN_POINT('Ctrl Pts',(22.4023943053151,0.465474217808745,4.1699201379362));
#42307=CARTESIAN_POINT('Ctrl Pts',(22.4262522233466,0.327147461276091,4.37217420322137));
#42308=CARTESIAN_POINT('Ctrl Pts',(22.450110141378,0.108824243893236,4.4834215400391));
#42309=CARTESIAN_POINT('Ctrl Pts',(22.4739680594094,-0.136109474402841,
4.47645913832327));
#42310=CARTESIAN_POINT('Ctrl Pts',(22.4978259774408,-0.347760701725541,
4.3529895060813));
#42311=CARTESIAN_POINT('Ctrl Pts',(22.5216838954723,-0.474374996640319,
4.1432043106148));
#42312=CARTESIAN_POINT('Ctrl Pts',(22.5455418135036,-0.484991622785221,
3.89840178635216));
#42313=CARTESIAN_POINT('Ctrl Pts',(22.5693997315351,-0.377014700254462,
3.67844274379546));
#42314=CARTESIAN_POINT('Ctrl Pts',(22.5932576495665,-0.176847198578467,
3.53711330196678));
#42315=CARTESIAN_POINT('Ctrl Pts',(22.6171155675979,0.0665638539184235,
3.50897209184919));
#42316=CARTESIAN_POINT('Ctrl Pts',(22.6409734856293,0.293698998435555,3.60090091054846));
#42317=CARTESIAN_POINT('Ctrl Pts',(22.6648314036608,0.449015288492166,3.79041970485759));
#42318=CARTESIAN_POINT('Ctrl Pts',(22.6886893216922,0.494537845944295,4.03118776656693));
#42319=CARTESIAN_POINT('Ctrl Pts',(22.7125472397236,0.419127261608858,4.26432734830583));
#42320=CARTESIAN_POINT('Ctrl Pts',(22.736405157755,0.241238408088568,4.43283588997321));
#42321=CARTESIAN_POINT('Ctrl Pts',(22.7602630757865,0.00434171083240793,
4.49549632518638));
#42322=CARTESIAN_POINT('Ctrl Pts',(22.7841209938178,-0.233581370990537,
4.43700954435219));
#42323=CARTESIAN_POINT('Ctrl Pts',(22.8079789118493,-0.414457183229959,
4.27163232278894));
#42324=CARTESIAN_POINT('Ctrl Pts',(22.8238841905369,-0.46737397936094,4.11714349286348));
#42325=CARTESIAN_POINT('Ctrl Pts',(22.8318368298807,-0.473742730682552,
4.03823705100924));
#42326=CARTESIAN_POINT('Ctrl Pts',(4.,-0.219892372743211,3.64701365460636));
#42327=CARTESIAN_POINT('Ctrl Pts',(4.00795263934381,-0.161099076858729,
3.61038844940468));
#42328=CARTESIAN_POINT('Ctrl Pts',(4.02385791803142,-0.0249198690254346,
3.56711791692558));
#42329=CARTESIAN_POINT('Ctrl Pts',(4.04771583606284,0.185569069288609,3.60813812632505));
#42330=CARTESIAN_POINT('Ctrl Pts',(4.07157375409426,0.350624105231944,3.74494568050885));
#42331=CARTESIAN_POINT('Ctrl Pts',(4.09543167212568,0.429971014252744,3.94413788601839));
#42332=CARTESIAN_POINT('Ctrl Pts',(4.1192895901571,0.40416308778273,4.15698104289539));
#42333=CARTESIAN_POINT('Ctrl Pts',(4.14314750818851,0.279534313346206,4.3314427366163));
#42334=CARTESIAN_POINT('Ctrl Pts',(4.16700542621994,0.0865475313004802,
4.42485517705098));
#42335=CARTESIAN_POINT('Ctrl Pts',(4.19086334425134,-0.127600227202394,
4.41438026490915));
#42336=CARTESIAN_POINT('Ctrl Pts',(4.21472126228278,-0.310547447266788,
4.30257739619942));
#42337=CARTESIAN_POINT('Ctrl Pts',(4.23857918031418,-0.417556725585918,
4.11678647978038));
#42338=CARTESIAN_POINT('Ctrl Pts',(4.26243709834561,-0.422462345057068,
3.90243789311793));
#42339=CARTESIAN_POINT('Ctrl Pts',(4.28629501637703,-0.324064236326554,
3.71194600226016));
#42340=CARTESIAN_POINT('Ctrl Pts',(4.31015293440845,-0.146423688323203,
3.59189110566319));
#42341=CARTESIAN_POINT('Ctrl Pts',(4.33401085243986,0.0670214896752265,
3.5716299793216));
#42342=CARTESIAN_POINT('Ctrl Pts',(4.35786877047129,0.264078061498623,3.65611697628114));
#42343=CARTESIAN_POINT('Ctrl Pts',(4.38172668850271,0.396560367883193,3.82469274783887));
#42344=CARTESIAN_POINT('Ctrl Pts',(4.40558460653412,0.432072854850341,4.03613591352675));
#42345=CARTESIAN_POINT('Ctrl Pts',(4.42944252456555,0.361931763288092,4.23874286631049));
#42346=CARTESIAN_POINT('Ctrl Pts',(4.45330044259696,0.203288494707987,4.382970683851));
#42347=CARTESIAN_POINT('Ctrl Pts',(4.47715836062838,-0.00506434719902249,
4.43355173791626));
#42348=CARTESIAN_POINT('Ctrl Pts',(4.5010162786598,-0.212178818846594,4.37811758201071));
#42349=CARTESIAN_POINT('Ctrl Pts',(4.52487419669122,-0.367409789343613,
4.23022337776645));
#42350=CARTESIAN_POINT('Ctrl Pts',(4.54873211472264,-0.432799058467291,
4.02603328640456));
#42351=CARTESIAN_POINT('Ctrl Pts',(4.57259003275406,-0.392357168499796,
3.8154773474345));
#42352=CARTESIAN_POINT('Ctrl Pts',(4.59644795078547,-0.255973263285106,
3.65004222328625));
#42353=CARTESIAN_POINT('Ctrl Pts',(4.6203058688169,-0.0569969226013119,
3.57018130821703));
#42354=CARTESIAN_POINT('Ctrl Pts',(4.64416378684831,0.155916718210686,3.59542277130738));
#42355=CARTESIAN_POINT('Ctrl Pts',(4.66802170487973,0.330704474340828,3.71959438727947));
#42356=CARTESIAN_POINT('Ctrl Pts',(4.69187962291115,0.424625978282027,3.91233281365517));
#42357=CARTESIAN_POINT('Ctrl Pts',(4.71573754094257,0.41471486395576,4.1265082550995));
#42358=CARTESIAN_POINT('Ctrl Pts',(4.73959545897399,0.303394668785218,4.30974898215573));
#42359=CARTESIAN_POINT('Ctrl Pts',(4.76345337700541,0.117886212792376,4.41724764568232));
#42360=CARTESIAN_POINT('Ctrl Pts',(4.78731129503683,-0.0964486333844469,
4.42271789424177));
#42361=CARTESIAN_POINT('Ctrl Pts',(4.81116921306824,-0.287199161490599,
4.32482210305491));
#42362=CARTESIAN_POINT('Ctrl Pts',(4.83502713109967,-0.407721671464292,
4.14749845969467));
#42363=CARTESIAN_POINT('Ctrl Pts',(4.85888504913109,-0.42854512664958,3.93410742516172));
#42364=CARTESIAN_POINT('Ctrl Pts',(4.8827429671625,-0.344577625034195,3.73682892005441));
#42365=CARTESIAN_POINT('Ctrl Pts',(4.90660088519393,-0.176351507991885,
3.60390291263011));
#42366=CARTESIAN_POINT('Ctrl Pts',(4.93045880322534,0.0349973564730633,
3.56783343253575));
#42367=CARTESIAN_POINT('Ctrl Pts',(4.95431672125677,0.237788413971502,3.63744045016736));
#42368=CARTESIAN_POINT('Ctrl Pts',(4.97817463928818,0.382433727027559,3.79570315365689));
#42369=CARTESIAN_POINT('Ctrl Pts',(5.0020325573196,0.433563576539811,4.00392200101168));
#42370=CARTESIAN_POINT('Ctrl Pts',(5.02589047535102,0.378675321553375,4.21118181228595));
#42371=CARTESIAN_POINT('Ctrl Pts',(5.04974839338244,0.231190635538481,4.36680191797922));
#42372=CARTESIAN_POINT('Ctrl Pts',(5.07360631141386,0.0271735416279573,
4.43272896324296));
#42373=CARTESIAN_POINT('Ctrl Pts',(5.09746422944527,-0.183488223403015,
4.39284198969348));
#42374=CARTESIAN_POINT('Ctrl Pts',(5.1213221474767,-0.349282119693095,4.256894448863));
#42375=CARTESIAN_POINT('Ctrl Pts',(5.1451800655081,-0.4296670234643,4.05812921762123));
#42376=CARTESIAN_POINT('Ctrl Pts',(5.16903798353954,-0.404986636103755,
3.84514980926298));
#42377=CARTESIAN_POINT('Ctrl Pts',(5.19289590157095,-0.281275984601366,
3.67003549057442));
#42378=CARTESIAN_POINT('Ctrl Pts',(5.21675381960238,-0.0887856930599551,
3.5756064824932));
#42379=CARTESIAN_POINT('Ctrl Pts',(5.24061173763379,0.125415118908336,3.58495324968971));
#42380=CARTESIAN_POINT('Ctrl Pts',(5.26446965566521,0.308948518064291,3.69579025298356));
#42381=CARTESIAN_POINT('Ctrl Pts',(5.28832757369662,0.416935588964862,3.88101482593007));
#42382=CARTESIAN_POINT('Ctrl Pts',(5.31218549172805,0.422970551266107,4.09533451502773));
#42383=CARTESIAN_POINT('Ctrl Pts',(5.33604340975946,0.325577692296299,4.28634231834109));
#42384=CARTESIAN_POINT('Ctrl Pts',(5.35990132779089,0.148572219001774,4.40733162501188));
#42385=CARTESIAN_POINT('Ctrl Pts',(5.3837592458223,-0.0647632088646815,
4.42871725387658));
#42386=CARTESIAN_POINT('Ctrl Pts',(5.40761716385372,-0.26226226804932,4.34526983614494));
#42387=CARTESIAN_POINT('Ctrl Pts',(5.43147508188515,-0.395631058815178,
4.17739453851434));
#42388=CARTESIAN_POINT('Ctrl Pts',(5.45533299991656,-0.432257278927009,
3.96614144408682));
#42389=CARTESIAN_POINT('Ctrl Pts',(5.47919091794798,-0.363184819889405,
3.76316768886851));
#42390=CARTESIAN_POINT('Ctrl Pts',(5.5030488359794,-0.205303779432806,3.61810588490468));
#42391=CARTESIAN_POINT('Ctrl Pts',(5.52690675401082,0.00277962745745752,
3.56642759466814));
#42392=CARTESIAN_POINT('Ctrl Pts',(5.55076467204224,0.210183339719457,3.62076956781107));
#42393=CARTESIAN_POINT('Ctrl Pts',(5.57462259007365,0.36619150013966,3.76784371165257));
#42394=CARTESIAN_POINT('Ctrl Pts',(5.59848050810508,0.432655863921731,3.97168639180759));
#42395=CARTESIAN_POINT('Ctrl Pts',(5.62233842613649,0.393324083661671,4.18245252040861));
#42396=CARTESIAN_POINT('Ctrl Pts',(5.64619634416792,0.257813851021257,4.34860403787086));
#42397=CARTESIAN_POINT('Ctrl Pts',(5.67005426219933,0.0592611090830247,
4.42951237227525));
#42398=CARTESIAN_POINT('Ctrl Pts',(5.69391218023075,-0.153782588238227,
4.40539323200473));
#42399=CARTESIAN_POINT('Ctrl Pts',(5.71777009826218,-0.329222253834466,
4.28214440376531));
#42400=CARTESIAN_POINT('Ctrl Pts',(5.74162801629359,-0.424158110434281,
4.08990358344764));
#42401=CARTESIAN_POINT('Ctrl Pts',(5.76548593432501,-0.415375755386326,
3.8756788878607));
#42402=CARTESIAN_POINT('Ctrl Pts',(5.78934385235642,-0.305022713182347,
3.69185409099321));
#42403=CARTESIAN_POINT('Ctrl Pts',(5.81320177038785,-0.120083309624962,
3.58337936191985));
#42404=CARTESIAN_POINT('Ctrl Pts',(5.83705968841926,0.0942197354074567,
3.57677972866706));
#42405=CARTESIAN_POINT('Ctrl Pts',(5.86091760645069,0.285483486244351,3.673668977605));
#42406=CARTESIAN_POINT('Ctrl Pts',(5.8847755244821,0.406938752801468,3.85035505520226));
#42407=CARTESIAN_POINT('Ctrl Pts',(5.90863344251353,0.428886400972996,4.06363338935351));
#42408=CARTESIAN_POINT('Ctrl Pts',(5.93249136054494,0.345959657594393,4.261351642888));
#42409=CARTESIAN_POINT('Ctrl Pts',(5.95634927857636,0.178436323746589,4.39516226965834));
#42410=CARTESIAN_POINT('Ctrl Pts',(5.98020719660778,-0.0327194942966983,
4.4323450160316));
#42411=CARTESIAN_POINT('Ctrl Pts',(6.0040651146392,-0.23587461323539,4.36380751861078));
#42412=CARTESIAN_POINT('Ctrl Pts',(6.02792303267061,-0.381351759249696,
4.20630938167977));
#42413=CARTESIAN_POINT('Ctrl Pts',(6.05178095070204,-0.433578399193506,
3.9983625870902));
#42414=CARTESIAN_POINT('Ctrl Pts',(6.07563886873346,-0.379782579589031,
3.79081692866841));
#42415=CARTESIAN_POINT('Ctrl Pts',(6.09949678676487,-0.233120953551068,
3.63442082419035));
#42416=CARTESIAN_POINT('Ctrl Pts',(6.12335470479629,-0.0294522997972467,
3.5674214393556));
#42417=CARTESIAN_POINT('Ctrl Pts',(6.14721262282771,0.181413325723775,3.60619428643423));
#42418=CARTESIAN_POINT('Ctrl Pts',(6.17107054085913,0.347927737305898,3.74127281623538));
#42419=CARTESIAN_POINT('Ctrl Pts',(6.19492845889055,0.429346806292137,3.93959933010928));
#42420=CARTESIAN_POINT('Ctrl Pts',(6.21878637692197,0.405811992579865,4.15272917617017));
#42421=CARTESIAN_POINT('Ctrl Pts',(6.24264429495339,0.282982581651336,4.32844890303245));
#42422=CARTESIAN_POINT('Ctrl Pts',(6.26650221298481,0.0910742457207041,
4.42397415233781));
#42423=CARTESIAN_POINT('Ctrl Pts',(6.29036013101623,-0.123327005978964,
4.41559921078967));
#42424=CARTESIAN_POINT('Ctrl Pts',(6.31421804904765,-0.307151379675736,
4.3060270879454));
#42425=CARTESIAN_POINT('Ctrl Pts',(6.33807596707907,-0.416657206472865,
4.12081787696614));
#42426=CARTESIAN_POINT('Ctrl Pts',(6.36193388511048,-0.422829889105799,
3.9075587958503));
#42427=CARTESIAN_POINT('Ctrl Pts',(6.39374444248571,-0.296437506874183,
3.64987069373525));
#42428=CARTESIAN_POINT('Ctrl Pts',(6.43350763920474,0.0703302468340302,
3.51324810367198));
#42429=CARTESIAN_POINT('Ctrl Pts',(6.48122347526758,0.448014600657906,3.7964368525222));
#42430=CARTESIAN_POINT('Ctrl Pts',(6.52893931133042,0.413240052911115,4.26646358767058));
#42431=CARTESIAN_POINT('Ctrl Pts',(6.57665514739325,-0.000480251589724132,
4.49184654025612));
#42432=CARTESIAN_POINT('Ctrl Pts',(6.62437098345609,-0.41404349770976,4.26553045144514));
#42433=CARTESIAN_POINT('Ctrl Pts',(6.67208681951894,-0.447234019333667,
3.79538894860702));
#42434=CARTESIAN_POINT('Ctrl Pts',(6.71980265558177,-0.0698021891909718,
3.51313682319347));
#42435=CARTESIAN_POINT('Ctrl Pts',(6.76751849164461,0.371772181936036,3.67798293440124));
#42436=CARTESIAN_POINT('Ctrl Pts',(6.81523432770745,0.471920133146607,4.13853999974893));
#42437=CARTESIAN_POINT('Ctrl Pts',(6.86295016377028,0.138708377331583,4.4718748549198));
#42438=CARTESIAN_POINT('Ctrl Pts',(6.91066599983312,-0.32188767172048,4.37187913281409));
#42439=CARTESIAN_POINT('Ctrl Pts',(6.95838183589596,-0.486886005735063,
3.93038141845316));
#42440=CARTESIAN_POINT('Ctrl Pts',(7.0060976719588,-0.204771183672361,3.55281534000283));
#42441=CARTESIAN_POINT('Ctrl Pts',(7.05381350802163,0.265389096458903,3.58590591031157));
#42442=CARTESIAN_POINT('Ctrl Pts',(7.10152934408448,0.491837993618785,3.99926540470374));
#42443=CARTESIAN_POINT('Ctrl Pts',(7.14924518014731,0.266624753986561,4.41329951581085));
#42444=CARTESIAN_POINT('Ctrl Pts',(7.19696101621015,-0.203434237821079,
4.44779430805676));
#42445=CARTESIAN_POINT('Ctrl Pts',(7.24467685227299,-0.486676365692783,
4.07107270446015));
#42446=CARTESIAN_POINT('Ctrl Pts',(7.29239268833582,-0.322996137187983,
3.62908393881966));
#42447=CARTESIAN_POINT('Ctrl Pts',(7.34010852439867,0.137296434535941,3.52771310152703));
#42448=CARTESIAN_POINT('Ctrl Pts',(7.3878243604615,0.471507566988788,3.86005058906394));
#42449=CARTESIAN_POINT('Ctrl Pts',(7.43554019652434,0.372726051350611,4.32090577464778));
#42450=CARTESIAN_POINT('Ctrl Pts',(7.48325603258718,-0.0683355354161961,
4.48706824929225));
#42451=CARTESIAN_POINT('Ctrl Pts',(7.53097186865002,-0.44664354691983,4.20594845626764));
#42452=CARTESIAN_POINT('Ctrl Pts',(7.57868770471286,-0.414791917646955,
3.73570302684109));
#42453=CARTESIAN_POINT('Ctrl Pts',(7.62640354077569,-0.00203048755240202,
3.50816557464413));
#42454=CARTESIAN_POINT('Ctrl Pts',(7.67411937683853,0.412595570264971,3.73228724307244));
#42455=CARTESIAN_POINT('Ctrl Pts',(7.72183521290137,0.448328767436039,4.20225365549051));
#42456=CARTESIAN_POINT('Ctrl Pts',(7.7695510489642,0.0723547589785895,4.48648742399228));
#42457=CARTESIAN_POINT('Ctrl Pts',(7.81726688502705,-0.370063737934377,
4.32397230547438));
#42458=CARTESIAN_POINT('Ctrl Pts',(7.86498272108989,-0.472647010158531,
3.86394843388276));
#42459=CARTESIAN_POINT('Ctrl Pts',(7.91269855715272,-0.141191260335066,
3.52886280888004));
#42460=CARTESIAN_POINT('Ctrl Pts',(7.96041439321556,0.31992259635559,3.62642971585976));
#42461=CARTESIAN_POINT('Ctrl Pts',(8.0081302292784,0.48724661017382,4.0670519628834));
#42462=CARTESIAN_POINT('Ctrl Pts',(8.05584606534124,0.207124564615173,4.44609936066402));
#42463=CARTESIAN_POINT('Ctrl Pts',(8.10356190140407,-0.263203155649882,
4.41548685142597));
#42464=CARTESIAN_POINT('Ctrl Pts',(8.15127773746691,-0.491827368180951,
4.00332637343646));
#42465=CARTESIAN_POINT('Ctrl Pts',(8.19899357352975,-0.268798940774433,
3.58811123553743));
#42466=CARTESIAN_POINT('Ctrl Pts',(8.24670940959259,0.201071689948468,3.55113988776764));
#42467=CARTESIAN_POINT('Ctrl Pts',(8.29442524565542,0.486295093906121,3.92636368766143));
#42468=CARTESIAN_POINT('Ctrl Pts',(8.34214108171827,0.324946230517931,4.36920884621601));
#42469=CARTESIAN_POINT('Ctrl Pts',(8.3898569177811,-0.134805756295296,4.47300384028212));
#42470=CARTESIAN_POINT('Ctrl Pts',(8.43757275384394,-0.470763542849379,
4.14243212971755));
#42471=CARTESIAN_POINT('Ctrl Pts',(8.48528858990678,-0.37441192437669,3.68106280283335));
#42472=CARTESIAN_POINT('Ctrl Pts',(8.53300442596962,0.0657679253190804,
3.51257841158684));
#42473=CARTESIAN_POINT('Ctrl Pts',(8.58072026203246,0.445552077224736,3.79170076492532));
#42474=CARTESIAN_POINT('Ctrl Pts',(8.62843609809529,0.41617890091499,4.26210751092856));
#42475=CARTESIAN_POINT('Ctrl Pts',(8.67615193415813,0.0046222361594965,
4.49181689660367));
#42476=CARTESIAN_POINT('Ctrl Pts',(8.72386777022097,-0.411179099183508,
4.26988325855195));
#42477=CARTESIAN_POINT('Ctrl Pts',(8.7715836062838,-0.449388340942622,3.80011167148426));
#42478=CARTESIAN_POINT('Ctrl Pts',(8.81929944234665,-0.0749173544856965,
3.51390061216986));
#42479=CARTESIAN_POINT('Ctrl Pts',(8.86701527840948,0.368351391347115,3.67408210030036));
#42480=CARTESIAN_POINT('Ctrl Pts',(8.91473111447233,0.473357386691186,4.13355901061654));
#42481=CARTESIAN_POINT('Ctrl Pts',(8.96244695053515,0.14367201029714,4.47038662641401));
#42482=CARTESIAN_POINT('Ctrl Pts',(9.01016278659801,-0.317949583830803,
4.37525096534692));
#42483=CARTESIAN_POINT('Ctrl Pts',(9.05787862266083,-0.487593182843731,
3.93551656882348));
#42484=CARTESIAN_POINT('Ctrl Pts',(9.10559445872368,-0.209472459465777,
3.55499829935456));
#42485=CARTESIAN_POINT('Ctrl Pts',(9.15331029478651,0.261010046587687,3.58313193881964));
#42486=CARTESIAN_POINT('Ctrl Pts',(9.20102613084934,0.491803010703882,3.99408193320625));
#42487=CARTESIAN_POINT('Ctrl Pts',(9.2487419669122,0.270965702728691,4.41046657939073));
#42488=CARTESIAN_POINT('Ctrl Pts',(9.29645780297501,-0.198703579405513,
4.44991344988054));
#42489=CARTESIAN_POINT('Ctrl Pts',(9.34417363903789,-0.485900307124067,
4.07619787653679));
#42490=CARTESIAN_POINT('Ctrl Pts',(9.39188947510068,-0.326887306273347,
3.63250862071426));
#42491=CARTESIAN_POINT('Ctrl Pts',(9.43960531116356,0.13231133773591,3.52629235307153));
#42492=CARTESIAN_POINT('Ctrl Pts',(9.48732114722637,0.470006444430667,3.85508910653225));
#42493=CARTESIAN_POINT('Ctrl Pts',(9.53503698328922,0.376087401226012,4.31695976320512));
#42494=CARTESIAN_POINT('Ctrl Pts',(9.58275281935206,-0.0631984893729827,
4.48776139227388));
#42495=CARTESIAN_POINT('Ctrl Pts',(9.63046865541489,-0.444448234747017,
4.21064422964382));
#42496=CARTESIAN_POINT('Ctrl Pts',(9.67818449147773,-0.41755432743774,3.74008922975375));
#42497=CARTESIAN_POINT('Ctrl Pts',(9.72590032754057,-0.00721385634321597,
3.50821428942208));
#42498=CARTESIAN_POINT('Ctrl Pts',(9.77361616360341,0.40975121003073,3.72795373420991));
#42499=CARTESIAN_POINT('Ctrl Pts',(9.82133199966624,0.450435435400681,4.19751745084266));
#42500=CARTESIAN_POINT('Ctrl Pts',(9.86904783572909,0.077477869602138,4.48569785316993));
#42501=CARTESIAN_POINT('Ctrl Pts',(9.91676367179192,-0.366628816002305,
4.3278544435092));
#42502=CARTESIAN_POINT('Ctrl Pts',(9.96447950785476,-0.474054618562381,
3.8689372536849));
#42503=CARTESIAN_POINT('Ctrl Pts',(10.0121953439176,-0.146148770628728,
3.53037700046135));
#42504=CARTESIAN_POINT('Ctrl Pts',(10.0599111799804,0.315967742161179,3.62307877379278));
#42505=CARTESIAN_POINT('Ctrl Pts',(10.1076270160433,0.487926215535836,4.06191310882887));
#42506=CARTESIAN_POINT('Ctrl Pts',(10.1553428521061,0.211814537474087,4.44389168337175));
#42507=CARTESIAN_POINT('Ctrl Pts',(10.203058688169,-0.258809689535701,4.4182376949229));
#42508=CARTESIAN_POINT('Ctrl Pts',(10.2507745242318,-0.491764996345908,
4.00850959581219));
#42509=CARTESIAN_POINT('Ctrl Pts',(10.2984903602946,-0.273124940234581,
3.59096700393021));
#42510=CARTESIAN_POINT('Ctrl Pts',(10.3462061963575,0.196329951061554,3.54904570612073));
#42511=CARTESIAN_POINT('Ctrl Pts',(10.3939220324203,0.485492027373267,3.92124267520431));
#42512=CARTESIAN_POINT('Ctrl Pts',(10.4416378684831,0.328819304693055,4.36576370748498));
#42513=CARTESIAN_POINT('Ctrl Pts',(10.489353704546,-0.129813245022134,4.47439829918413));
#42514=CARTESIAN_POINT('Ctrl Pts',(10.5370695406088,-0.469236294399976,
4.14738563318641));
#42515=CARTESIAN_POINT('Ctrl Pts',(10.5847853766716,-0.377752434501872,
3.68502647241413));
#42516=CARTESIAN_POINT('Ctrl Pts',(10.6325012127345,0.0606272984676223,
3.51191234851464));
#42517=CARTESIAN_POINT('Ctrl Pts',(10.6802170487973,0.443332050383407,3.78701662516801));
#42518=CARTESIAN_POINT('Ctrl Pts',(10.7279328848602,0.418918158891686,4.25770681210006));
#42519=CARTESIAN_POINT('Ctrl Pts',(10.775648720923,0.00980527620531799,
4.49174086815163));
#42520=CARTESIAN_POINT('Ctrl Pts',(10.8233645569858,-0.408311942493964,
4.27420171857372));
#42521=CARTESIAN_POINT('Ctrl Pts',(10.8710803930487,-0.451470021714238,
3.80485891169382));
#42522=CARTESIAN_POINT('Ctrl Pts',(10.9187962291115,-0.080036233235122,
3.51471716883706));
#42523=CARTESIAN_POINT('Ctrl Pts',(10.9665120651743,0.364896059739551,3.6702181168734));
#42524=CARTESIAN_POINT('Ctrl Pts',(11.0142279012372,0.47473868640782,4.1285628425314));
#42525=CARTESIAN_POINT('Ctrl Pts',(11.0619437373,0.148621472554162,4.46884633169921));
#42526=CARTESIAN_POINT('Ctrl Pts',(11.1096595733629,-0.313977126381285,
4.37858102033954));
#42527=CARTESIAN_POINT('Ctrl Pts',(11.1573754094257,-0.488245699001722,
3.94065893278431));
#42528=CARTESIAN_POINT('Ctrl Pts',(11.2050912454886,-0.214150733603143,
3.55723066033293));
#42529=CARTESIAN_POINT('Ctrl Pts',(11.2528070815514,0.256602145595791,3.58040428537983));
#42530=CARTESIAN_POINT('Ctrl Pts',(11.3005229176142,0.491713326162588,3.98889911147238));
#42531=CARTESIAN_POINT('Ctrl Pts',(11.3482387536771,0.275276593332242,4.40758805430897));
#42532=CARTESIAN_POINT('Ctrl Pts',(11.3959545897399,-0.193950870829933,
4.45198261532529));
#42533=CARTESIAN_POINT('Ctrl Pts',(11.4436704258028,-0.485070265991237,
4.08131458604192));
#42534=CARTESIAN_POINT('Ctrl Pts',(11.4913862618656,-0.330742172127369,
3.63597412121053));
#42535=CARTESIAN_POINT('Ctrl Pts',(11.5391020979284,0.127311547523522,3.52492422212962));
#42536=CARTESIAN_POINT('Ctrl Pts',(11.5868179339912,0.468453114143607,3.85014371984754));
#42537=CARTESIAN_POINT('Ctrl Pts',(11.6345337700541,0.379406977967949,4.31297854546471));
#42538=CARTESIAN_POINT('Ctrl Pts',(11.6822496061169,-0.0580544240024287,
4.48840035698771));
#42539=CARTESIAN_POINT('Ctrl Pts',(11.7299654421798,-0.44220355512924,4.21531660568344));
#42540=CARTESIAN_POINT('Ctrl Pts',(11.7776812782426,-0.420270357404582,
3.74450430230823));
#42541=CARTESIAN_POINT('Ctrl Pts',(11.8253971143054,-0.0123964237846327,
3.50831762943));
#42542=CARTESIAN_POINT('Ctrl Pts',(11.8731129503683,0.406861336540243,3.72365044295193));
#42543=CARTESIAN_POINT('Ctrl Pts',(11.9208287864311,0.452492071153857,4.1927593068956));
#42544=CARTESIAN_POINT('Ctrl Pts',(11.968544622494,0.0825923743414284,4.48485433333386));
#42545=CARTESIAN_POINT('Ctrl Pts',(12.0162604585568,-0.363153170675764,
4.33170016502878));
#42546=CARTESIAN_POINT('Ctrl Pts',(12.0639762946196,-0.475409571231627,
3.87394063131468));
#42547=CARTESIAN_POINT('Ctrl Pts',(12.1116921306825,-0.151090047408964,
3.53194335553704));
#42548=CARTESIAN_POINT('Ctrl Pts',(12.1594079667453,0.311977791768556,3.61976969834691));
#42549=CARTESIAN_POINT('Ctrl Pts',(12.2071238028081,0.488551624369653,4.05676737776005));
#42550=CARTESIAN_POINT('Ctrl Pts',(12.254839638871,0.216480982979095,4.44163470069774));
#42551=CARTESIAN_POINT('Ctrl Pts',(12.3025554749338,-0.254387476069249,
4.42094208256136));
#42552=CARTESIAN_POINT('Ctrl Pts',(12.3502713109967,-0.49164800158875,4.0136918729824));
#42553=CARTESIAN_POINT('Ctrl Pts',(12.3979871470595,-0.277420602272412,
3.59386820576715));
#42554=CARTESIAN_POINT('Ctrl Pts',(12.4457029831224,0.191566404775332,3.54700161433684));
#42555=CARTESIAN_POINT('Ctrl Pts',(12.4934188191852,0.484635034689867,3.91613041073711));
#42556=CARTESIAN_POINT('Ctrl Pts',(12.541134655248,0.332655855180181,4.362277941457));
#42557=CARTESIAN_POINT('Ctrl Pts',(12.5888504913109,-0.124806314709729,
4.47574006417428));
#42558=CARTESIAN_POINT('Ctrl Pts',(12.6365663273737,-0.4676569254097,4.15232276575852));
#42559=CARTESIAN_POINT('Ctrl Pts',(12.6842821634365,-0.381050985679211,
3.68902512775968));
#42560=CARTESIAN_POINT('Ctrl Pts',(12.7319979994994,0.0554799374235607,
3.5113004999026));
#42561=CARTESIAN_POINT('Ctrl Pts',(12.7797138355622,0.441062780321708,3.78235614259331));
#42562=CARTESIAN_POINT('Ctrl Pts',(12.8274296716251,0.421610885427219,4.2532774884218));
#42563=CARTESIAN_POINT('Ctrl Pts',(12.8751455076879,0.0149872271275763,
4.49161021945745));
#42564=CARTESIAN_POINT('Ctrl Pts',(12.9228613437507,-0.405399432451448,
4.27848972156979));
#42565=CARTESIAN_POINT('Ctrl Pts',(12.9705771798136,-0.453501555338242,
3.80962782724943));
#42566=CARTESIAN_POINT('Ctrl Pts',(13.0182930158764,-0.0851462219395619,
3.51558762841831));
#42567=CARTESIAN_POINT('Ctrl Pts',(13.0660088519392,0.361400197209248,3.66639076405307));
#42568=CARTESIAN_POINT('Ctrl Pts',(13.1137246880021,0.476067254403989,4.1235523942958));
#42569=CARTESIAN_POINT('Ctrl Pts',(13.1614405240649,0.153554426643267,4.46725395975876));
#42570=CARTESIAN_POINT('Ctrl Pts',(13.2091563601278,-0.30996979384252,4.38186902434892));
#42571=CARTESIAN_POINT('Ctrl Pts',(13.2568721961906,-0.488843983144383,
3.94580788806928));
#42572=CARTESIAN_POINT('Ctrl Pts',(13.3045880322534,-0.218805220893238,
3.55951220202843));
#42573=CARTESIAN_POINT('Ctrl Pts',(13.3523038683163,0.252165742455243,3.57772323864086));
#42574=CARTESIAN_POINT('Ctrl Pts',(13.4000197043791,0.491569024438394,3.98371752277252));
#42575=CARTESIAN_POINT('Ctrl Pts',(13.447735540442,0.279556907518101,4.40466425628032));
#42576=CARTESIAN_POINT('Ctrl Pts',(13.4954513765048,-0.189176619112,4.45400157668594));
#42577=CARTESIAN_POINT('Ctrl Pts',(13.5431672125676,-0.484186345555107,
4.08642226350871));
#42578=CARTESIAN_POINT('Ctrl Pts',(13.5908830486304,-0.334560300710407,
3.63948005597396));
#42579=CARTESIAN_POINT('Ctrl Pts',(13.6385988846933,0.122297616148583,3.52360886035071));
#42580=CARTESIAN_POINT('Ctrl Pts',(13.6863147207561,0.466847750307624,3.8452149784873));
#42581=CARTESIAN_POINT('Ctrl Pts',(13.734030556819,0.3826844119832,4.30896256355269));
#42582=CARTESIAN_POINT('Ctrl Pts',(13.7817463928818,-0.0529039102219543,
4.48898507250754));
#42583=CARTESIAN_POINT('Ctrl Pts',(13.8294622289446,-0.439909757638992,
4.21996506537626));
#42584=CARTESIAN_POINT('Ctrl Pts',(13.8771780650075,-0.422939705734467,
3.74894775411238));
#42585=CARTESIAN_POINT('Ctrl Pts',(13.9248939010703,-0.0175776142901187,
3.50847558318244));
#42586=CARTESIAN_POINT('Ctrl Pts',(13.9726097371332,0.403926270823208,3.71937784729135));
#42587=CARTESIAN_POINT('Ctrl Pts',(14.020325573196,0.454498446235019,4.18797975215946));
#42588=CARTESIAN_POINT('Ctrl Pts',(14.0680414092588,0.0876977051117048,
4.48395695817926));
#42589=CARTESIAN_POINT('Ctrl Pts',(14.1157572453217,-0.359637188018331,
4.33550904286807));
#42590=CARTESIAN_POINT('Ctrl Pts',(14.1634730813845,-0.476711717661702,
3.87895801102093));
#42591=CARTESIAN_POINT('Ctrl Pts',(14.2111889174473,-0.156014541823709,
3.53356170012368));
#42592=CARTESIAN_POINT('Ctrl Pts',(14.2589047535102,0.307953188363286,3.61650285707861));
#42593=CARTESIAN_POINT('Ctrl Pts',(14.306620589573,0.4891227672074,4.05161534124029));
#42594=CARTESIAN_POINT('Ctrl Pts',(14.3543364256359,0.2211233828038,4.4393286633369));
#42595=CARTESIAN_POINT('Ctrl Pts',(14.4020522616987,-0.249937006449114,
4.42359971395084));
#42596=CARTESIAN_POINT('Ctrl Pts',(14.4497680977616,-0.491476396904638,
4.01887262932433));
#42597=CARTESIAN_POINT('Ctrl Pts',(14.4974839338244,-0.281685449746218,
3.59681451879656));
#42598=CARTESIAN_POINT('Ctrl Pts',(14.5451997698872,0.186781580201919,3.54500783946397));
#42599=CARTESIAN_POINT('Ctrl Pts',(14.59291560595,0.483724211046603,3.91102746210588));
#42600=CARTESIAN_POINT('Ctrl Pts',(14.6406314420129,0.33645545583349,4.35875193531444));
#42601=CARTESIAN_POINT('Ctrl Pts',(14.6883472780757,-0.119785521504147,
4.47702898621568));
#42602=CARTESIAN_POINT('Ctrl Pts',(14.7360631141386,-0.466025611307368,
4.15724297904063));
#42603=CARTESIAN_POINT('Ctrl Pts',(14.7837789502014,-0.38430721152129,3.69305832471834));
#42604=CARTESIAN_POINT('Ctrl Pts',(14.8314947862642,0.0503264139313189,
3.51074293371195));
#42605=CARTESIAN_POINT('Ctrl Pts',(14.8792106223271,0.438744519099385,3.77771983486548));
#42606=CARTESIAN_POINT('Ctrl Pts',(14.9269264583899,0.42425678142631,4.24882003188202));
#42607=CARTESIAN_POINT('Ctrl Pts',(14.9746422944528,0.0201675133397715,
4.49142496503298));
#42608=CARTESIAN_POINT('Ctrl Pts',(15.0223581305156,-0.402441892563756,
4.28274679124913));
#42609=CARTESIAN_POINT('Ctrl Pts',(15.0700739665785,-0.455482716161518,
3.8144178884426));
#42610=CARTESIAN_POINT('Ctrl Pts',(15.1177898026413,-0.0902467530057116,
3.51651189422706));
#42611=CARTESIAN_POINT('Ctrl Pts',(15.1655056387041,0.357864192060027,3.66260046696357));
#42612=CARTESIAN_POINT('Ctrl Pts',(15.2132214747669,0.47734294310866,4.11852822244656));
#42613=CARTESIAN_POINT('Ctrl Pts',(15.2609373108298,0.15847032463534,4.46560968746574));
#42614=CARTESIAN_POINT('Ctrl Pts',(15.3086531468926,-0.305928031329979,
4.38511461215921));
#42615=CARTESIAN_POINT('Ctrl Pts',(15.3563689829555,-0.489387968817152,
3.95096286275689));
#42616=CARTESIAN_POINT('Ctrl Pts',(15.4040848190183,-0.223435404337718,
3.56184267101825));
#42617=CARTESIAN_POINT('Ctrl Pts',(15.4518006550811,0.24770132994065,3.57508909640066));
#42618=CARTESIAN_POINT('Ctrl Pts',(15.499516491144,0.491370121559653,3.97853774265298));
#42619=CARTESIAN_POINT('Ctrl Pts',(15.5472323272068,0.283806169849271,4.40169551006635));
#42620=CARTESIAN_POINT('Ctrl Pts',(15.5949481632697,-0.184381354552937,
4.4559701097059));
#42621=CARTESIAN_POINT('Ctrl Pts',(15.6426639993325,-0.483248643997369,
4.09152034160055));
#42622=CARTESIAN_POINT('Ctrl Pts',(15.6903798353953,-0.338341267922855,
3.64302603558196));
#42623=CARTESIAN_POINT('Ctrl Pts',(15.7380956714582,0.117270100534806,3.52234641383892));
#42624=CARTESIAN_POINT('Ctrl Pts',(15.785811507521,0.465190531238913,3.84030342991275));
#42625=CARTESIAN_POINT('Ctrl Pts',(15.8335273435838,0.385919339229949,4.30491226354526));
#42626=CARTESIAN_POINT('Ctrl Pts',(15.8812431796467,-0.0477475201261761,
4.48951547388594));
#42627=CARTESIAN_POINT('Ctrl Pts',(15.9289590157095,-0.437567097060412,
4.22458909239344));
#42628=CARTESIAN_POINT('Ctrl Pts',(15.9766748517724,-0.425562075928853,
3.75341909160864));
#42629=CARTESIAN_POINT('Ctrl Pts',(16.0243906878352,-0.0227568523576073,
3.50868813313462));
#42630=CARTESIAN_POINT('Ctrl Pts',(16.072106523898,0.400946338892803,3.71513642180785));
#42631=CARTESIAN_POINT('Ctrl Pts',(16.1198223599609,0.456454337785543,4.1831793175245));
#42632=CARTESIAN_POINT('Ctrl Pts',(16.1675381960237,0.0927932948370443,
4.4830058273823));
#42633=CARTESIAN_POINT('Ctrl Pts',(16.2152540320865,-0.356081258568678,
4.33928065395499));
#42634=CARTESIAN_POINT('Ctrl Pts',(16.2629698681494,-0.477960913216358,
3.88398883549692));
#42635=CARTESIAN_POINT('Ctrl Pts',(16.3106857042122,-0.160921706883503,
3.53523185446324));
#42636=CARTESIAN_POINT('Ctrl Pts',(16.358401540275,0.303894378979202,3.6132786128531));
#42637=CARTESIAN_POINT('Ctrl Pts',(16.4061173763379,0.489639580609251,4.04645757153336));
#42638=CARTESIAN_POINT('Ctrl Pts',(16.4538332124007,0.225741221292456,4.43697382743292));
#42639=CARTESIAN_POINT('Ctrl Pts',(16.5015490484636,-0.245458775012363,
4.42621029389423));
#42640=CARTESIAN_POINT('Ctrl Pts',(16.5492648845264,-0.4912502013546,4.02405128938415));
#42641=CARTESIAN_POINT('Ctrl Pts',(16.5969807205893,-0.285919008936969,
3.59980561575594));
#42642=CARTESIAN_POINT('Ctrl Pts',(16.6446965566521,0.181976008816936,3.54306460296116));
#42643=CARTESIAN_POINT('Ctrl Pts',(16.6924123927149,0.482759657613431,3.90593439612197));
#42644=CARTESIAN_POINT('Ctrl Pts',(16.7401282287778,0.340217684611379,4.35518608070932));
#42645=CARTESIAN_POINT('Ctrl Pts',(16.7878440648406,-0.114751423091257,
4.47826492214097));
#42646=CARTESIAN_POINT('Ctrl Pts',(16.8355599009034,-0.464342533291602,
4.16214572651883));
#42647=CARTESIAN_POINT('Ctrl Pts',(16.8832757369663,-0.387520750342007,
3.69712561530174));
#42648=CARTESIAN_POINT('Ctrl Pts',(16.9309915730291,0.0451673004198413,
3.51023971187451));
#42649=CARTESIAN_POINT('Ctrl Pts',(16.978707409092,0.436377524217892,3.7731082169636));
#42650=CARTESIAN_POINT('Ctrl Pts',(17.0264232451548,0.426855552995382,4.24433493759383));
#42651=CARTESIAN_POINT('Ctrl Pts',(17.0741390812176,0.0253455594402812,
4.49118512545541));
#42652=CARTESIAN_POINT('Ctrl Pts',(17.1218549172805,-0.399439651340385,
4.28697245475663));
#42653=CARTESIAN_POINT('Ctrl Pts',(17.1695707533433,-0.457413284126125,
3.81922856321607));
#42654=CARTESIAN_POINT('Ctrl Pts',(17.2172865894061,-0.0953372598908034,
3.51748986360026));
#42655=CARTESIAN_POINT('Ctrl Pts',(17.265002425469,0.354288437054553,3.6588476466131));
#42656=CARTESIAN_POINT('Ctrl Pts',(17.3127182615318,0.478565610824392,4.11349088504481));
#42657=CARTESIAN_POINT('Ctrl Pts',(17.3604340975947,0.163368620495752,4.46391369745815));
#42658=CARTESIAN_POINT('Ctrl Pts',(17.4081499336575,-0.301852287783465,
4.38831742326589));
#42659=CARTESIAN_POINT('Ctrl Pts',(17.4558657697204,-0.489877595596684,
3.956123284257));
#42660=CARTESIAN_POINT('Ctrl Pts',(17.5035816057832,-0.228040769637767,
3.56422180844494));
#42661=CARTESIAN_POINT('Ctrl Pts',(17.551297441846,0.243209403937772,3.57250215124727));
#42662=CARTESIAN_POINT('Ctrl Pts',(17.5990132779089,0.491116639619549,3.97336034645914));
#42663=CARTESIAN_POINT('Ctrl Pts',(17.6467291139717,0.288023908337871,4.39868214542132));
#42664=CARTESIAN_POINT('Ctrl Pts',(17.6944449500345,-0.179565609787963,
4.45788799572981));
#42665=CARTESIAN_POINT('Ctrl Pts',(17.7421607860973,-0.48225726547346,4.09660825404716));
#42666=CARTESIAN_POINT('Ctrl Pts',(17.7898766221602,-0.342084653792828,
3.64661166616396));
#42667=CARTESIAN_POINT('Ctrl Pts',(17.837592458223,0.112229559114723,3.52113702282083));
#42668=CARTESIAN_POINT('Ctrl Pts',(17.8853082942859,0.463481641013499,3.83540961967535));
#42669=CARTESIAN_POINT('Ctrl Pts',(17.9330241303487,0.389111400387848,4.30082809533052));
#42670=CARTESIAN_POINT('Ctrl Pts',(17.9807399664116,-0.0425858264624495,
4.48999150220845));
#42671=CARTESIAN_POINT('Ctrl Pts',(18.0284558024744,-0.435175833605105,
4.22918817311999));
#42672=CARTESIAN_POINT('Ctrl Pts',(18.0761716385373,-0.428137176707308,
3.75791781814212));
#42673=CARTESIAN_POINT('Ctrl Pts',(18.1238874746,-0.0279335627019553,3.5089552556775));
#42674=CARTESIAN_POINT('Ctrl Pts',(18.1716033106629,0.397921871745719,3.71092663761881));
#42675=CARTESIAN_POINT('Ctrl Pts',(18.2193191467257,0.458359528554279,4.17835853620019));
#42676=CARTESIAN_POINT('Ctrl Pts',(18.2670349827886,0.097878577523561,4.48200104659009));
#42677=CARTESIAN_POINT('Ctrl Pts',(18.3147508188514,-0.352485777302551,
4.34301457935691));
#42678=CARTESIAN_POINT('Ctrl Pts',(18.3624666549143,-0.479157019140895,
3.88903254594255));
#42679=CARTESIAN_POINT('Ctrl Pts',(18.4101824909771,-0.165810997523729,
3.5369536330429));
#42680=CARTESIAN_POINT('Ctrl Pts',(18.4578983270399,0.299801814449608,3.61009732380414));
#42681=CARTESIAN_POINT('Ctrl Pts',(18.5056141631028,0.49010200717001,4.04129464153984));
#42682=CARTESIAN_POINT('Ctrl Pts',(18.5533299991656,0.230333985517487,4.43457045454981));
#42683=CARTESIAN_POINT('Ctrl Pts',(18.6010458352284,-0.24095327917969,4.42877353242069));
#42684=CARTESIAN_POINT('Ctrl Pts',(18.6487616712913,-0.49096944006335,4.0292272779409));
#42685=CARTESIAN_POINT('Ctrl Pts',(18.6964775073541,-0.290120809601049,
3.60284116440841));
#42686=CARTESIAN_POINT('Ctrl Pts',(18.744193343417,0.177150224400508,3.54117212067402));
#42687=CARTESIAN_POINT('Ctrl Pts',(18.7919091794797,0.481741481528227,3.90085177849878));
#42688=CARTESIAN_POINT('Ctrl Pts',(18.8396250155427,0.343942123623612,4.35158077372017));
#42689=CARTESIAN_POINT('Ctrl Pts',(18.8873408516054,-0.109704578635382,
4.47944773466767));
#42690=CARTESIAN_POINT('Ctrl Pts',(18.9350566876684,-0.462607878309702,
4.16703046362027));
#42691=CARTESIAN_POINT('Ctrl Pts',(18.9827725237311,-0.39069124519864,3.70122654773242));
#42692=CARTESIAN_POINT('Ctrl Pts',(19.030488359794,0.0400031699426168,3.50979089028978));
#42693=CARTESIAN_POINT('Ctrl Pts',(19.0782041958568,0.433962058584907,3.76852180111673));
#42694=CARTESIAN_POINT('Ctrl Pts',(19.1259200319197,0.429406911488226,4.23982270375453));
#42695=CARTESIAN_POINT('Ctrl Pts',(19.1736358679825,0.0305207902517796,
4.49089072733801));
#42696=CARTESIAN_POINT('Ctrl Pts',(19.2213517040454,-0.396393042209671,
4.29116624277653));
#42697=CARTESIAN_POINT('Ctrl Pts',(19.2690675401082,-0.459293044881286,
3.82405931712685));
#42698=CARTESIAN_POINT('Ctrl Pts',(19.316783376171,-0.100417177000157,3.51852142809106));
#42699=CARTESIAN_POINT('Ctrl Pts',(19.3644992122339,0.350673329058588,3.65513271950473));
#42700=CARTESIAN_POINT('Ctrl Pts',(19.4122150482967,0.479735122332443,4.10844094226069));
#42701=CARTESIAN_POINT('Ctrl Pts',(19.4599308843596,0.168248769032157,4.46216617689766));
#42702=CARTESIAN_POINT('Ctrl Pts',(19.5076467204224,-0.297743013815871,
4.39147710422109));
#42703=CARTESIAN_POINT('Ctrl Pts',(19.5553625564852,-0.490312813065352,
3.96128857502183));
#42704=CARTESIAN_POINT('Ctrl Pts',(19.603078392548,-0.232620797759261,3.56664935826393));
#42705=CARTESIAN_POINT('Ctrl Pts',(19.6507942286109,0.238690449241969,3.56996267500769));
#42706=CARTESIAN_POINT('Ctrl Pts',(19.6985100646737,0.490808633485035,3.96818593857384));
#42707=CARTESIAN_POINT('Ctrl Pts',(19.7462259007366,0.292209604061002,4.39562444172689));
#42708=CARTESIAN_POINT('Ctrl Pts',(19.7939417367994,-0.174729824492781,
4.45975512619968));
#42709=CARTESIAN_POINT('Ctrl Pts',(19.8416575728622,-0.481212499922896,
4.10168523844358));
#42710=CARTESIAN_POINT('Ctrl Pts',(19.8893734089251,-0.345789702982467,
3.65023692191923));
#42711=CARTESIAN_POINT('Ctrl Pts',(19.9370892449879,0.107175910646637,3.51998011832295));
#42712=CARTESIAN_POINT('Ctrl Pts',(19.9848050810508,0.461722480014006,3.83053541934297));
#42713=CARTESIAN_POINT('Ctrl Pts',(20.0325209171136,0.392257955100357,4.29670800504879));
#42714=CARTESIAN_POINT('Ctrl Pts',(20.0802367531764,-0.0374150865130887,
4.49041783929577));
#42715=CARTESIAN_POINT('Ctrl Pts',(20.1279525892393,-0.432744382500041,
4.23375285658289));
#42716=CARTESIAN_POINT('Ctrl Pts',(20.1756684253021,-0.430649333670284,
3.76246031529274));
#42717=CARTESIAN_POINT('Ctrl Pts',(20.223384261365,-0.033136228617316,3.50924504180455));
#42718=CARTESIAN_POINT('Ctrl Pts',(20.2711000974278,0.394908089060633,3.70680919012016));
#42719=CARTESIAN_POINT('Ctrl Pts',(20.3188159334906,0.460110046434968,4.17340395051402));
#42720=CARTESIAN_POINT('Ctrl Pts',(20.3665317695535,0.103149962306437,4.48116018402389));
#42721=CARTESIAN_POINT('Ctrl Pts',(20.4142476056163,-0.34923165553999,4.34628168153608));
#42722=CARTESIAN_POINT('Ctrl Pts',(20.4540108023354,-0.457800032585507,
3.97025345815189));
#42723=CARTESIAN_POINT('Ctrl Pts',(20.4858213597105,-0.325993724402262,
3.71529210935379));
#42724=CARTESIAN_POINT('Ctrl Pts',(20.509679277742,-0.15096738523986,3.59329490328468));
#42725=CARTESIAN_POINT('Ctrl Pts',(20.5335371957734,0.0630371972956549,
3.57102347342756));
#42726=CARTESIAN_POINT('Ctrl Pts',(20.5573951138048,0.260511246441404,3.65349437971329));
#42727=CARTESIAN_POINT('Ctrl Pts',(20.5812530318362,0.394877283734959,3.82077798440408));
#42728=CARTESIAN_POINT('Ctrl Pts',(20.6051109498677,0.432370081305563,4.03184236506754));
#42729=CARTESIAN_POINT('Ctrl Pts',(20.6289688678991,0.364303478986858,4.23514367899931));
#42730=CARTESIAN_POINT('Ctrl Pts',(20.6528267859305,0.207066376217976,4.38093363836299));
#42731=CARTESIAN_POINT('Ctrl Pts',(20.6766847039619,-0.000757290757721993,
4.43358147160167));
#42732=CARTESIAN_POINT('Ctrl Pts',(20.7005426219933,-0.208420567790133,
4.38020336888205));
#42733=CARTESIAN_POINT('Ctrl Pts',(20.7244005400248,-0.365106210756856,
4.23385701605743));
#42734=CARTESIAN_POINT('Ctrl Pts',(20.7482584580562,-0.432520392530856,
4.03032528343114));
#42735=CARTESIAN_POINT('Ctrl Pts',(20.7721163760876,-0.394167874571092,
3.81937870627435));
#42736=CARTESIAN_POINT('Ctrl Pts',(20.795974294119,-0.259432524437891,3.65259868360638));
#42737=CARTESIAN_POINT('Ctrl Pts',(20.8198322121504,-0.0612578225112809,
3.57076788979259));
#42738=CARTESIAN_POINT('Ctrl Pts',(20.8436901301819,0.151895538690754,3.5938959627232));
#42739=CARTESIAN_POINT('Ctrl Pts',(20.8675480482132,0.327906592802717,3.71632757520176));
#42740=CARTESIAN_POINT('Ctrl Pts',(20.8914059662447,0.423735399567132,3.90812480123879));
#42741=CARTESIAN_POINT('Ctrl Pts',(20.9152638842761,0.415949440063929,4.12238802732943));
#42742=CARTESIAN_POINT('Ctrl Pts',(20.9391218023075,0.30645246920106,4.30672404095661));
#42743=CARTESIAN_POINT('Ctrl Pts',(20.962979720339,0.122019544809087,4.41605767475162));
#42744=CARTESIAN_POINT('Ctrl Pts',(20.9868376383703,-0.0922504941031022,
4.42365387220386));
#42745=CARTESIAN_POINT('Ctrl Pts',(21.0106955564018,-0.28396276796243,4.32765515869354));
#42746=CARTESIAN_POINT('Ctrl Pts',(21.0345534744332,-0.40623841344949,4.15153583326342));
#42747=CARTESIAN_POINT('Ctrl Pts',(21.0584113924646,-0.429177699343215,
3.93836186909709));
#42748=CARTESIAN_POINT('Ctrl Pts',(21.082269310496,-0.347171348131155,3.74026010679315));
#42749=CARTESIAN_POINT('Ctrl Pts',(21.1061272285274,-0.180272145040548,
3.605671823621));
#42750=CARTESIAN_POINT('Ctrl Pts',(21.1299851465589,0.0307085077608185,
3.56750752082027));
#42751=CARTESIAN_POINT('Ctrl Pts',(21.1538430645903,0.234180094072738,3.63509941005724));
#42752=CARTESIAN_POINT('Ctrl Pts',(21.1777009826217,0.380388268371489,3.79191943321731));
#42753=CARTESIAN_POINT('Ctrl Pts',(21.2015589006531,0.433581149524578,3.99962082296209));
#42754=CARTESIAN_POINT('Ctrl Pts',(21.2254168186846,0.380751629084578,4.2074149318183));
#42755=CARTESIAN_POINT('Ctrl Pts',(21.2492747367159,0.234817963878357,4.36449043997717));
#42756=CARTESIAN_POINT('Ctrl Pts',(21.2731326547474,0.0314649101850846,
4.43243810704058));
#42757=CARTESIAN_POINT('Ctrl Pts',(21.2969905727788,-0.179582171132277,
4.39464287755545));
#42758=CARTESIAN_POINT('Ctrl Pts',(21.3208484908102,-0.346716519889314,
4.26034671465164));
#42759=CARTESIAN_POINT('Ctrl Pts',(21.3447064088417,-0.429069235164158,
4.0623886883135));
#42760=CARTESIAN_POINT('Ctrl Pts',(21.368564326873,-0.406502834830527,3.8491749282489));
#42761=CARTESIAN_POINT('Ctrl Pts',(21.3924222449045,-0.284535418465691,
3.67284200661995));
#42762=CARTESIAN_POINT('Ctrl Pts',(21.4162801629359,-0.0929913416969399,
3.5765081259772));
#42763=CARTESIAN_POINT('Ctrl Pts',(21.4401380809674,0.121291651150069,3.58372954422009));
#42764=CARTESIAN_POINT('Ctrl Pts',(21.4639959989987,0.305915531372611,3.69274042788069));
#42765=CARTESIAN_POINT('Ctrl Pts',(21.4878539170302,0.415734731202803,3.87688464650718));
#42766=CARTESIAN_POINT('Ctrl Pts',(21.5117118350615,0.423895464867194,4.09113392265755));
#42767=CARTESIAN_POINT('Ctrl Pts',(21.535569753093,0.328402210690932,4.28309847227994));
#42768=CARTESIAN_POINT('Ctrl Pts',(21.5594276711244,0.152605670504114,4.40583773398234));
#42769=CARTESIAN_POINT('Ctrl Pts',(21.5832855891559,-0.0605071130159612,
4.42933861492812));
#42770=CARTESIAN_POINT('Ctrl Pts',(21.6071435071872,-0.258824259222961,
4.34785450957493));
#42771=CARTESIAN_POINT('Ctrl Pts',(21.6310014252187,-0.39385182381868,4.18131050126406));
#42772=CARTESIAN_POINT('Ctrl Pts',(21.6548593432501,-0.432571889182456,
3.97043113659525));
#42773=CARTESIAN_POINT('Ctrl Pts',(21.6787172612815,-0.365516344619441,
3.76678216446856));
#42774=CARTESIAN_POINT('Ctrl Pts',(21.702575179313,-0.209082097331647,3.62016130585559));
#42775=CARTESIAN_POINT('Ctrl Pts',(21.7264330973443,-0.00152158196427748,
3.56642135455923));
#42776=CARTESIAN_POINT('Ctrl Pts',(21.7502910153758,0.206411001640417,3.61870319251831));
#42777=CARTESIAN_POINT('Ctrl Pts',(21.7741489334072,0.363870472821225,3.76422248622317));
#42778=CARTESIAN_POINT('Ctrl Pts',(21.7980068514386,0.432353701764573,3.96739580449697));
#42779=CARTESIAN_POINT('Ctrl Pts',(21.82186476947,0.395114673548107,4.17854173669174));
#42780=CARTESIAN_POINT('Ctrl Pts',(21.8457226875014,0.261259344941517,4.3460293508861));
#42781=CARTESIAN_POINT('Ctrl Pts',(21.8695806055329,0.0635189899350569,
4.42890336313855));
#42782=CARTESIAN_POINT('Ctrl Pts',(21.8934385235643,-0.14975348833307,4.40689882001058));
#42783=CARTESIAN_POINT('Ctrl Pts',(21.9172964415957,-0.326407159500644,
4.28539643168872));
#42784=CARTESIAN_POINT('Ctrl Pts',(21.9411543596271,-0.423245389017799,
4.09410684177624));
#42785=CARTESIAN_POINT('Ctrl Pts',(21.9650122776585,-0.416588591947193,
3.87980556563057));
#42786=CARTESIAN_POINT('Ctrl Pts',(21.98887019569,-0.30806453650007,3.69489510271888));
#42787=CARTESIAN_POINT('Ctrl Pts',(22.0127281137213,-0.12421031036921,3.58459109808296));
#42788=CARTESIAN_POINT('Ctrl Pts',(22.0365860317528,0.0900167200678817,
3.57586588547707));
#42789=CARTESIAN_POINT('Ctrl Pts',(22.0604439497842,0.282232210442068,3.67085301705332));
#42790=CARTESIAN_POINT('Ctrl Pts',(22.0843018678157,0.405434237512275,3.8463255517439));
#42791=CARTESIAN_POINT('Ctrl Pts',(22.108159785847,0.429496549703537,4.05937567504088));
#42792=CARTESIAN_POINT('Ctrl Pts',(22.1320177038785,0.348535256241736,4.25790682842971));
#42793=CARTESIAN_POINT('Ctrl Pts',(22.1558756219099,0.182347598717988,4.39337273702606));
#42794=CARTESIAN_POINT('Ctrl Pts',(22.1797335399413,-0.0284290137391457,
4.43264829616218));
#42795=CARTESIAN_POINT('Ctrl Pts',(22.2035914579727,-0.232253957950086,
4.36612956178204));
#42796=CARTESIAN_POINT('Ctrl Pts',(22.2274493760041,-0.379286482964224,
4.21008217638027));
#42797=CARTESIAN_POINT('Ctrl Pts',(22.2513072940356,-0.433573131350875,
4.00266397632408));
#42798=CARTESIAN_POINT('Ctrl Pts',(22.275165212067,-0.381839338801546,3.79459436150246));
#42799=CARTESIAN_POINT('Ctrl Pts',(22.2990231300984,-0.236735426869051,
3.63675202040985));
#42800=CARTESIAN_POINT('Ctrl Pts',(22.3228810481298,-0.0337432544318164,
3.56773370504276));
#42801=CARTESIAN_POINT('Ctrl Pts',(22.3467389661613,0.177500062688638,3.60441627341574));
#42802=CARTESIAN_POINT('Ctrl Pts',(22.3705968841926,0.345339779804043,3.73782983856348));
#42803=CARTESIAN_POINT('Ctrl Pts',(22.3944548022241,0.428734513273282,3.93535114928888));
#42804=CARTESIAN_POINT('Ctrl Pts',(22.4183127202555,0.407291980919218,4.1486808655136));
#42805=CARTESIAN_POINT('Ctrl Pts',(22.4421706382869,0.286255462618544,4.32565405918856));
#42806=CARTESIAN_POINT('Ctrl Pts',(22.4660285563183,0.0952216904214238,
4.42299596654013));
#42807=CARTESIAN_POINT('Ctrl Pts',(22.4898864743497,-0.119096386717928,
4.41690383452019));
#42808=CARTESIAN_POINT('Ctrl Pts',(22.5137443923812,-0.304292138366774,
4.30886736509782));
#42809=CARTESIAN_POINT('Ctrl Pts',(22.5376023104126,-0.415080201412036,
4.12530439950267));
#42810=CARTESIAN_POINT('Ctrl Pts',(22.561460228444,-0.424369795825249,3.91110111771763));
#42811=CARTESIAN_POINT('Ctrl Pts',(22.5853181464754,-0.329889515310188,
3.71863599132299));
#42812=CARTESIAN_POINT('Ctrl Pts',(22.6091760645068,-0.154742073939436,
3.59497211022641));
#42813=CARTESIAN_POINT('Ctrl Pts',(22.6330339825383,0.0582436639512456,
3.57034842802071));
#42814=CARTESIAN_POINT('Ctrl Pts',(22.6568919005697,0.256987911016647,3.65078654733876));
#42815=CARTESIAN_POINT('Ctrl Pts',(22.6807498186011,0.39289034562191,3.81661632308649));
#42816=CARTESIAN_POINT('Ctrl Pts',(22.7046077366325,0.432722782933869,4.02728943245291));
#42817=CARTESIAN_POINT('Ctrl Pts',(22.7284656546639,0.366738191089385,4.2312875884069));
#42818=CARTESIAN_POINT('Ctrl Pts',(22.7523235726953,0.211084664509997,4.37873330099785));
#42819=CARTESIAN_POINT('Ctrl Pts',(22.7761814907268,0.00379901600965994,
4.43356145647204));
#42820=CARTESIAN_POINT('Ctrl Pts',(22.8000394087582,-0.204384723485633,
4.3823852668741));
#42821=CARTESIAN_POINT('Ctrl Pts',(22.8238973267896,-0.36265185203719,4.2376794731));
#42822=CARTESIAN_POINT('Ctrl Pts',(22.8398026054772,-0.408954280604672,
4.10250106973657));
#42823=CARTESIAN_POINT('Ctrl Pts',(22.847755244821,-0.414526965927561,4.03345758723954));
#42824=CARTESIAN_POINT('',(22.8,-0.592174260192535,4.04779597854866));
#42825=CARTESIAN_POINT('Ctrl Pts',(22.8,-0.19576256658266,4.36695865185836));
#42826=CARTESIAN_POINT('Ctrl Pts',(22.8,-0.195886593570853,4.36694806728808));
#42827=CARTESIAN_POINT('Ctrl Pts',(22.8,-0.196010613870461,4.36693742279878));
#42828=CARTESIAN_POINT('Ctrl Pts',(22.8,-0.196134627427637,4.36692671841166));
#42829=CARTESIAN_POINT('Ctrl Pts',(22.8,-0.216622178843513,4.36515830948628));
#42830=CARTESIAN_POINT('Ctrl Pts',(22.8,-0.236921239981942,4.36175743074964));
#42831=CARTESIAN_POINT('Ctrl Pts',(22.8,-0.256857422940798,4.35688458679081));
#42832=CARTESIAN_POINT('Ctrl Pts',(22.8,-0.271809560159941,4.35322995382169));
#42833=CARTESIAN_POINT('Ctrl Pts',(22.8,-0.286558947067823,4.34874691155445));
#42834=CARTESIAN_POINT('Ctrl Pts',(22.8,-0.301048271828705,4.34349077646485));
#42835=CARTESIAN_POINT('Ctrl Pts',(22.8,-0.310003423377303,4.3402422133286));
#42836=CARTESIAN_POINT('Ctrl Pts',(22.8,-0.318859482942331,4.33669811041118));
#42837=CARTESIAN_POINT('Ctrl Pts',(22.8,-0.327604744452034,4.33286912874946));
#42838=CARTESIAN_POINT('Ctrl Pts',(22.8,-0.333457186121174,4.33030672489195));
#42839=CARTESIAN_POINT('Ctrl Pts',(22.8,-0.33926207870774,4.32761569029118));
#42840=CARTESIAN_POINT('Ctrl Pts',(22.8,-0.345009487597299,4.32480202294401));
#42841=CARTESIAN_POINT('Ctrl Pts',(22.8,-0.365309066997251,4.31486428146495));
#42842=CARTESIAN_POINT('Ctrl Pts',(22.8,-0.384828901796994,4.30343044333042));
#42843=CARTESIAN_POINT('Ctrl Pts',(22.8,-0.403416958856431,4.29067119823496));
#42844=CARTESIAN_POINT('Ctrl Pts',(22.8,-0.409874425773003,4.28623865303559));
#42845=CARTESIAN_POINT('Ctrl Pts',(22.8,-0.416219739836017,4.28164578247975));
#42846=CARTESIAN_POINT('Ctrl Pts',(22.8,-0.422447327171508,4.27689854297234));
#42847=CARTESIAN_POINT('Ctrl Pts',(22.8,-0.43500295340691,4.2673274905416));
#42848=CARTESIAN_POINT('Ctrl Pts',(22.8,-0.447079966647781,4.25712966465555));
#42849=CARTESIAN_POINT('Ctrl Pts',(22.8,-0.458660056443695,4.24636133358853));
#42850=CARTESIAN_POINT('Ctrl Pts',(22.8,-0.465333929961841,4.24015529539631));
#42851=CARTESIAN_POINT('Ctrl Pts',(22.8,-0.471842796551704,4.23375955955572));
#42852=CARTESIAN_POINT('Ctrl Pts',(22.8,-0.478183280583292,4.22718326898633));
#42853=CARTESIAN_POINT('Ctrl Pts',(22.8,-0.48330469601013,4.22187138494));
#42854=CARTESIAN_POINT('Ctrl Pts',(22.8,-0.488310096860405,4.21644792156372));
#42855=CARTESIAN_POINT('Ctrl Pts',(22.8,-0.49319389770791,4.21092357737429));
#42856=CARTESIAN_POINT('Ctrl Pts',(22.8,-0.509882204568999,4.19204648678071));
#42857=CARTESIAN_POINT('Ctrl Pts',(22.8,-0.525164669297395,4.17198027236651));
#42858=CARTESIAN_POINT('Ctrl Pts',(22.8,-0.538985569877159,4.15095378743758));
#42859=CARTESIAN_POINT('Ctrl Pts',(22.8,-0.553292287721507,4.12918820238033));
#42860=CARTESIAN_POINT('Ctrl Pts',(22.8,-0.566034197593199,4.10639346234103));
#42861=CARTESIAN_POINT('Ctrl Pts',(22.8,-0.577149101532509,4.08276767497818));
#42862=CARTESIAN_POINT('Ctrl Pts',(22.8,-0.582543745751794,4.07130084468266));
#42863=CARTESIAN_POINT('Ctrl Pts',(22.8,-0.587554988912119,4.05963744408228));
#42864=CARTESIAN_POINT('Ctrl Pts',(22.8,-0.592174260192535,4.04779597854866));
#42865=CARTESIAN_POINT('Ctrl Pts',(22.8,-0.592174260192532,4.04779597854869));
#42866=CARTESIAN_POINT('Ctrl Pts',(22.7920473606562,-0.584213376873468,
4.14642833911734));
#42867=CARTESIAN_POINT('Ctrl Pts',(22.7840947213124,-0.551140611244481,
4.24298318064208));
#42868=CARTESIAN_POINT('Ctrl Pts',(22.7761420819686,-0.496922031827459,
4.32571394759471));
#42869=CARTESIAN_POINT('Ctrl Pts',(22.7681894426248,-0.442703452410443,
4.40844471454734));
#42870=CARTESIAN_POINT('Ctrl Pts',(22.760236803281,-0.367339059205388,4.47735140692785));
#42871=CARTESIAN_POINT('Ctrl Pts',(22.7522841639372,-0.280089901523161,
4.52398941366922));
#42872=CARTESIAN_POINT('Ctrl Pts',(22.7444712463773,-0.194373644734646,
4.56980802634291));
#42873=CARTESIAN_POINT('Ctrl Pts',(22.7366583288174,-0.0971865673270821,
4.59413356703531));
#42874=CARTESIAN_POINT('Ctrl Pts',(22.7288454112575,-7.11440487624268E-7,
4.59414971000239));
#42875=CARTESIAN_POINT('Origin',(27.2,0.3,2.9));
#42876=CARTESIAN_POINT('',(29.2,0.3,3.04606079858305));
#42877=CARTESIAN_POINT('',(27.2,0.3,3.04606079858305));
#42878=CARTESIAN_POINT('',(23.3,0.3,3.04606079858305));
#42879=CARTESIAN_POINT('',(29.2,0.3,3.35));
#42880=CARTESIAN_POINT('',(29.2,0.3,2.9));
#42881=CARTESIAN_POINT('',(27.2,0.3,3.35));
#42882=CARTESIAN_POINT('',(27.2,0.3,3.35));
#42883=CARTESIAN_POINT('',(27.2,0.3,2.9));
#42884=CARTESIAN_POINT('Origin',(27.2,0.,3.125));
#42885=CARTESIAN_POINT('',(27.2,-0.3,3.04606079858305));
#42886=CARTESIAN_POINT('Origin',(27.2,0.,4.));
#42887=CARTESIAN_POINT('',(27.2,-0.3,3.35));
#42888=CARTESIAN_POINT('',(27.2,0.3,3.35));
#42889=CARTESIAN_POINT('',(27.2,-0.3,3.35));
#42890=CARTESIAN_POINT('Origin',(27.2,0.3,3.35));
#42891=CARTESIAN_POINT('',(29.2,-0.3,3.35));
#42892=CARTESIAN_POINT('',(29.2,0.3,3.35));
#42893=CARTESIAN_POINT('',(27.2,-0.3,3.35));
#42894=CARTESIAN_POINT('Origin',(27.2,-0.3,3.35));
#42895=CARTESIAN_POINT('',(29.2,-0.3,3.04606079858305));
#42896=CARTESIAN_POINT('',(23.3,-0.3,3.04606079858305));
#42897=CARTESIAN_POINT('',(29.2,-0.3,3.35));
#42898=CARTESIAN_POINT('Origin',(29.2,0.,3.125));
#42899=CARTESIAN_POINT('Origin',(29.2,0.,4.));
#42900=CARTESIAN_POINT('Origin',(23.3,0.,4.));
#42901=CARTESIAN_POINT('',(29.4,-1.22464679914735E-16,5.));
#42902=CARTESIAN_POINT('Origin',(29.4,0.,4.));
#42903=CARTESIAN_POINT('',(23.3,-1.22464679914735E-16,5.));
#42904=CARTESIAN_POINT('',(23.3,-1.22464679914735E-16,5.));
#42905=CARTESIAN_POINT('Origin',(23.3,0.,4.));
#42906=CARTESIAN_POINT('Origin',(29.4,0.,4.));
#42907=CARTESIAN_POINT('Origin',(22.8,0.,4.));
#42908=CARTESIAN_POINT('',(22.8,-1.65327317884893E-16,5.35));
#42909=CARTESIAN_POINT('Origin',(22.8,0.,4.));
#42910=CARTESIAN_POINT('Origin',(22.8,0.,4.));
#42911=CARTESIAN_POINT('Origin',(22.8,0.,4.));
#42912=CARTESIAN_POINT('',(23.3,-1.65327317884893E-16,5.35));
#42913=CARTESIAN_POINT('Origin',(23.3,0.,4.));
#42914=CARTESIAN_POINT('',(22.8,-1.65327317884893E-16,5.35));
#42915=CARTESIAN_POINT('Origin',(23.3,0.,4.));
#42916=CARTESIAN_POINT('Origin',(4.,0.,4.));
#42917=CARTESIAN_POINT('',(0.,0.,0.));
#42918=CARTESIAN_POINT('Origin',(24.7,0.,4.));
#42919=CARTESIAN_POINT('',(25.4,-1.23689326713883E-16,5.01));
#42920=CARTESIAN_POINT('Origin',(25.4,0.,4.));
#42921=CARTESIAN_POINT('',(24.7,-1.23689326713883E-16,5.01));
#42922=CARTESIAN_POINT('',(24.7,-1.23689326713883E-16,5.01));
#42923=CARTESIAN_POINT('Origin',(24.7,0.,4.));
#42924=CARTESIAN_POINT('Origin',(24.7,0.,4.));
#42925=CARTESIAN_POINT('',(25.4,-1.65327317884893E-16,5.35));
#42926=CARTESIAN_POINT('Origin',(25.4,0.,4.));
#42927=CARTESIAN_POINT('',(24.7,-1.65327317884893E-16,5.35));
#42928=CARTESIAN_POINT('',(24.7,-1.65327317884893E-16,5.35));
#42929=CARTESIAN_POINT('Origin',(24.7,0.,4.));
#42930=CARTESIAN_POINT('Origin',(25.4,0.,4.));
#42931=CARTESIAN_POINT('Origin',(24.7,0.,4.));
#42932=CARTESIAN_POINT('',(0.,0.,0.));
#42933=CARTESIAN_POINT('Origin',(25.8,0.99,4.));
#42934=CARTESIAN_POINT('',(25.6809411910021,0.99,4.17298843892006));
#42935=CARTESIAN_POINT('',(25.9190588089979,0.99,4.17298843892006));
#42936=CARTESIAN_POINT('',(25.4,0.99,4.17298843892006));
#42937=CARTESIAN_POINT('Origin',(25.8,0.99,4.));
#42938=CARTESIAN_POINT('Origin',(25.8,0.99,4.));
#42939=CARTESIAN_POINT('',(25.6809411910021,0.99,3.82701156107994));
#42940=CARTESIAN_POINT('',(25.59,1.005,4.));
#42941=CARTESIAN_POINT('Ctrl Pts',(25.6809411910021,0.989999999999999,3.82701156107994));
#42942=CARTESIAN_POINT('Ctrl Pts',(25.6701985776047,0.99129192197638,3.83440513468868));
#42943=CARTESIAN_POINT('Ctrl Pts',(25.6603122906273,0.992653949439047,3.84270286127439));
#42944=CARTESIAN_POINT('Ctrl Pts',(25.6329072257467,0.996748084390898,3.87010792615492));
#42945=CARTESIAN_POINT('Ctrl Pts',(25.6167579436671,0.999695893276376,3.89366983224072));
#42946=CARTESIAN_POINT('Ctrl Pts',(25.5953022060351,1.00385029472357,3.94538709536759));
#42947=CARTESIAN_POINT('Ctrl Pts',(25.59,1.005,3.97354876917015));
#42948=CARTESIAN_POINT('Ctrl Pts',(25.59,1.005,4.));
#42949=CARTESIAN_POINT('',(25.9190588089979,0.99,3.82701156107994));
#42950=CARTESIAN_POINT('Origin',(25.8,0.99,4.));
#42951=CARTESIAN_POINT('Ctrl Pts',(25.9190588089979,0.99,4.17298843892006));
#42952=CARTESIAN_POINT('Ctrl Pts',(25.9298014223953,0.991291921976381,4.16559486531132));
#42953=CARTESIAN_POINT('Ctrl Pts',(25.9396877093727,0.992653949439047,4.15729713872561));
#42954=CARTESIAN_POINT('Ctrl Pts',(25.9670927742533,0.996748084390898,4.12989207384508));
#42955=CARTESIAN_POINT('Ctrl Pts',(25.9832420563329,0.999695893276376,4.10633016775929));
#42956=CARTESIAN_POINT('Ctrl Pts',(26.0046977939649,1.00385029472357,4.05461290463241));
#42957=CARTESIAN_POINT('Ctrl Pts',(26.01,1.005,4.02645123082985));
#42958=CARTESIAN_POINT('Ctrl Pts',(26.01,1.005,3.97354876917015));
#42959=CARTESIAN_POINT('Ctrl Pts',(26.0046977939649,1.00385029472357,3.94538709536759));
#42960=CARTESIAN_POINT('Ctrl Pts',(25.9832420563329,0.999695893276376,3.89366983224072));
#42961=CARTESIAN_POINT('Ctrl Pts',(25.9670927742533,0.996748084390898,3.87010792615492));
#42962=CARTESIAN_POINT('Ctrl Pts',(25.9396877093727,0.992653949439047,3.84270286127439));
#42963=CARTESIAN_POINT('Ctrl Pts',(25.9298014223953,0.991291921976381,3.83440513468868));
#42964=CARTESIAN_POINT('Ctrl Pts',(25.9190588089979,0.99,3.82701156107994));
#42965=CARTESIAN_POINT('Ctrl Pts',(25.59,1.005,4.));
#42966=CARTESIAN_POINT('Ctrl Pts',(25.59,1.005,4.02645123082985));
#42967=CARTESIAN_POINT('Ctrl Pts',(25.5953022060351,1.00385029472357,4.05461290463241));
#42968=CARTESIAN_POINT('Ctrl Pts',(25.6167579436671,0.999695893276376,4.10633016775929));
#42969=CARTESIAN_POINT('Ctrl Pts',(25.6329072257467,0.996748084390898,4.12989207384508));
#42970=CARTESIAN_POINT('Ctrl Pts',(25.6603122906273,0.992653949439047,4.15729713872561));
#42971=CARTESIAN_POINT('Ctrl Pts',(25.6701985776047,0.991291921976381,4.16559486531132));
#42972=CARTESIAN_POINT('Ctrl Pts',(25.6809411910021,0.99,4.17298843892006));
#42973=CARTESIAN_POINT('',(25.59,1.5,4.));
#42974=CARTESIAN_POINT('',(25.59,0.99,4.));
#42975=CARTESIAN_POINT('',(25.8,1.48522725533839,4.21));
#42976=CARTESIAN_POINT('Ctrl Pts',(25.8,1.48522725533839,4.21));
#42977=CARTESIAN_POINT('Ctrl Pts',(25.7735944730755,1.48522725533839,4.21));
#42978=CARTESIAN_POINT('Ctrl Pts',(25.7454529259093,1.48600415954412,4.2047157372696));
#42979=CARTESIAN_POINT('Ctrl Pts',(25.6937237310949,1.48880073282317,4.18327376303633));
#42980=CARTESIAN_POINT('Ctrl Pts',(25.670133075872,1.49077897157582,4.16711792397039));
#42981=CARTESIAN_POINT('Ctrl Pts',(25.632882321789,1.49448481141327,4.12986716988737));
#42982=CARTESIAN_POINT('Ctrl Pts',(25.6167262899986,1.49645455657129,4.10627640830577));
#42983=CARTESIAN_POINT('Ctrl Pts',(25.5952841751738,1.49923165515646,4.0545468514059));
#42984=CARTESIAN_POINT('Ctrl Pts',(25.59,1.5,4.02640517850928));
#42985=CARTESIAN_POINT('Ctrl Pts',(25.59,1.5,4.));
#42986=CARTESIAN_POINT('Ctrl Pts',(25.59,1.5,4.));
#42987=CARTESIAN_POINT('Ctrl Pts',(25.59,1.5,3.97359482149072));
#42988=CARTESIAN_POINT('Ctrl Pts',(25.5952841751738,1.49923165515646,3.9454531485941));
#42989=CARTESIAN_POINT('Ctrl Pts',(25.6167262899986,1.49645455657129,3.89372359169423));
#42990=CARTESIAN_POINT('Ctrl Pts',(25.632882321789,1.49448481141327,3.87013283011263));
#42991=CARTESIAN_POINT('Ctrl Pts',(25.670133075872,1.49077897157582,3.83288207602961));
#42992=CARTESIAN_POINT('Ctrl Pts',(25.6937237310949,1.48880073282317,3.81672623696366));
#42993=CARTESIAN_POINT('Ctrl Pts',(25.7454529259093,1.48600415954412,3.7952842627304));
#42994=CARTESIAN_POINT('Ctrl Pts',(25.7735944730755,1.48522725533839,3.79));
#42995=CARTESIAN_POINT('Ctrl Pts',(25.8264055269245,1.48522725533839,3.79));
#42996=CARTESIAN_POINT('Ctrl Pts',(25.8545470740907,1.48600415954412,3.7952842627304));
#42997=CARTESIAN_POINT('Ctrl Pts',(25.9062762689051,1.48880073282317,3.81672623696367));
#42998=CARTESIAN_POINT('Ctrl Pts',(25.929866924128,1.49077897157582,3.83288207602961));
#42999=CARTESIAN_POINT('Ctrl Pts',(25.967117678211,1.49448481141327,3.87013283011263));
#43000=CARTESIAN_POINT('Ctrl Pts',(25.9832737100014,1.49645455657129,3.89372359169423));
#43001=CARTESIAN_POINT('Ctrl Pts',(26.0047158248262,1.49923165515646,3.9454531485941));
#43002=CARTESIAN_POINT('Ctrl Pts',(26.01,1.5,3.97359482149072));
#43003=CARTESIAN_POINT('Ctrl Pts',(26.01,1.5,4.02640517850928));
#43004=CARTESIAN_POINT('Ctrl Pts',(26.0047158248262,1.49923165515646,4.0545468514059));
#43005=CARTESIAN_POINT('Ctrl Pts',(25.9832737100014,1.49645455657129,4.10627640830577));
#43006=CARTESIAN_POINT('Ctrl Pts',(25.967117678211,1.49448481141327,4.12986716988737));
#43007=CARTESIAN_POINT('Ctrl Pts',(25.929866924128,1.49077897157582,4.16711792397039));
#43008=CARTESIAN_POINT('Ctrl Pts',(25.9062762689051,1.48880073282317,4.18327376303633));
#43009=CARTESIAN_POINT('Ctrl Pts',(25.8545470740907,1.48600415954412,4.20471573726959));
#43010=CARTESIAN_POINT('Ctrl Pts',(25.8264055269245,1.48522725533839,4.21));
#43011=CARTESIAN_POINT('Ctrl Pts',(25.8,1.48522725533839,4.21));
#43012=CARTESIAN_POINT('Origin',(25.8,0.99,4.));
#43013=CARTESIAN_POINT('',(25.4,0.99,3.82701156107994));
#43014=CARTESIAN_POINT('Origin',(25.4,0.,4.));
#43015=CARTESIAN_POINT('',(26.2,-1.23077003314309E-16,5.005));
#43016=CARTESIAN_POINT('Origin',(26.2,0.,4.));
#43017=CARTESIAN_POINT('',(25.4,-1.23077003314309E-16,5.005));
#43018=CARTESIAN_POINT('',(25.4,-1.23077003314309E-16,5.005));
#43019=CARTESIAN_POINT('Origin',(25.4,0.,4.));
#43020=CARTESIAN_POINT('Origin',(25.4,0.,4.));
#43021=CARTESIAN_POINT('',(26.2,-1.83697019872103E-16,5.5));
#43022=CARTESIAN_POINT('Origin',(26.2,0.,4.));
#43023=CARTESIAN_POINT('',(25.4,-1.83697019872103E-16,5.5));
#43024=CARTESIAN_POINT('',(25.4,-1.83697019872103E-16,5.5));
#43025=CARTESIAN_POINT('Origin',(25.4,0.,4.));
#43026=CARTESIAN_POINT('Origin',(26.2,0.,4.));
#43027=CARTESIAN_POINT('Origin',(25.4,0.,4.));
#43028=CARTESIAN_POINT('',(0.,0.,0.));
#43029=CARTESIAN_POINT('Origin',(28.7,0.,6.5));
#43030=CARTESIAN_POINT('',(28.8,-3.06161699786838E-17,6.75));
#43031=CARTESIAN_POINT('Origin',(28.8,0.,6.5));
#43032=CARTESIAN_POINT('',(29.4,3.06161699786838E-17,6.75));
#43033=CARTESIAN_POINT('',(28.7,-3.06161699786838E-17,6.75));
#43034=CARTESIAN_POINT('Origin',(29.4,0.,6.5));
#43035=CARTESIAN_POINT('Origin',(28.,0.99,4.));
#43036=CARTESIAN_POINT('',(27.844436508139,0.99,4.14106735979666));
#43037=CARTESIAN_POINT('',(28.155563491861,0.99,4.14106735979666));
#43038=CARTESIAN_POINT('',(27.,0.99,4.14106735979666));
#43039=CARTESIAN_POINT('Origin',(28.,0.99,4.));
#43040=CARTESIAN_POINT('Origin',(28.,0.99,4.));
#43041=CARTESIAN_POINT('',(27.844436508139,0.99,3.85893264020334));
#43042=CARTESIAN_POINT('',(27.79,1.,4.));
#43043=CARTESIAN_POINT('Ctrl Pts',(27.844436508139,0.99,3.85893264020334));
#43044=CARTESIAN_POINT('Ctrl Pts',(27.8287948476368,0.992457849824465,3.87618164330178));
#43045=CARTESIAN_POINT('Ctrl Pts',(27.815375956669,0.994938193049464,3.8970013568903));
#43046=CARTESIAN_POINT('Ctrl Pts',(27.7953025362756,0.998844492372413,3.94538588560165));
#43047=CARTESIAN_POINT('Ctrl Pts',(27.79,1.,3.97354792631755));
#43048=CARTESIAN_POINT('Ctrl Pts',(27.79,1.,4.));
#43049=CARTESIAN_POINT('',(28.155563491861,0.99,3.85893264020334));
#43050=CARTESIAN_POINT('Origin',(28.,0.99,4.));
#43051=CARTESIAN_POINT('Ctrl Pts',(28.155563491861,0.99,4.14106735979666));
#43052=CARTESIAN_POINT('Ctrl Pts',(28.1712051523632,0.992457849824465,4.12381835669823));
#43053=CARTESIAN_POINT('Ctrl Pts',(28.184624043331,0.994938193049464,4.1029986431097));
#43054=CARTESIAN_POINT('Ctrl Pts',(28.2046974637244,0.998844492372413,4.05461411439835));
#43055=CARTESIAN_POINT('Ctrl Pts',(28.21,1.,4.02645207368245));
#43056=CARTESIAN_POINT('Ctrl Pts',(28.21,1.,3.97354792631755));
#43057=CARTESIAN_POINT('Ctrl Pts',(28.2046974637244,0.998844492372413,3.94538588560165));
#43058=CARTESIAN_POINT('Ctrl Pts',(28.184624043331,0.994938193049464,3.8970013568903));
#43059=CARTESIAN_POINT('Ctrl Pts',(28.1712051523632,0.992457849824465,3.87618164330178));
#43060=CARTESIAN_POINT('Ctrl Pts',(28.155563491861,0.99,3.85893264020334));
#43061=CARTESIAN_POINT('Ctrl Pts',(27.79,1.,4.));
#43062=CARTESIAN_POINT('Ctrl Pts',(27.79,1.,4.02645207368245));
#43063=CARTESIAN_POINT('Ctrl Pts',(27.7953025362756,0.998844492372413,4.05461411439835));
#43064=CARTESIAN_POINT('Ctrl Pts',(27.815375956669,0.994938193049464,4.1029986431097));
#43065=CARTESIAN_POINT('Ctrl Pts',(27.8287948476368,0.992457849824465,4.12381835669823));
#43066=CARTESIAN_POINT('Ctrl Pts',(27.844436508139,0.99,4.14106735979666));
#43067=CARTESIAN_POINT('',(27.79,1.5,4.));
#43068=CARTESIAN_POINT('',(27.79,0.99,4.));
#43069=CARTESIAN_POINT('',(28.,1.48522725533839,4.21));
#43070=CARTESIAN_POINT('Ctrl Pts',(28.,1.48522725533839,4.21));
#43071=CARTESIAN_POINT('Ctrl Pts',(27.9735944730755,1.48522725533839,4.21));
#43072=CARTESIAN_POINT('Ctrl Pts',(27.9454529259093,1.48600415954412,4.20471573726959));
#43073=CARTESIAN_POINT('Ctrl Pts',(27.8937237310949,1.48880073282317,4.18327376303633));
#43074=CARTESIAN_POINT('Ctrl Pts',(27.870133075872,1.49077897157582,4.16711792397039));
#43075=CARTESIAN_POINT('Ctrl Pts',(27.832882321789,1.49448481141327,4.12986716988737));
#43076=CARTESIAN_POINT('Ctrl Pts',(27.8167262899986,1.49645455657129,4.10627640830576));
#43077=CARTESIAN_POINT('Ctrl Pts',(27.7952841751738,1.49923165515646,4.0545468514059));
#43078=CARTESIAN_POINT('Ctrl Pts',(27.79,1.5,4.02640517850928));
#43079=CARTESIAN_POINT('Ctrl Pts',(27.79,1.5,4.));
#43080=CARTESIAN_POINT('Ctrl Pts',(27.79,1.5,4.));
#43081=CARTESIAN_POINT('Ctrl Pts',(27.79,1.5,3.97359482149072));
#43082=CARTESIAN_POINT('Ctrl Pts',(27.7952841751738,1.49923165515646,3.9454531485941));
#43083=CARTESIAN_POINT('Ctrl Pts',(27.8167262899986,1.49645455657129,3.89372359169424));
#43084=CARTESIAN_POINT('Ctrl Pts',(27.832882321789,1.49448481141327,3.87013283011263));
#43085=CARTESIAN_POINT('Ctrl Pts',(27.870133075872,1.49077897157582,3.83288207602961));
#43086=CARTESIAN_POINT('Ctrl Pts',(27.8937237310949,1.48880073282317,3.81672623696367));
#43087=CARTESIAN_POINT('Ctrl Pts',(27.9454529259093,1.48600415954412,3.7952842627304));
#43088=CARTESIAN_POINT('Ctrl Pts',(27.9735944730755,1.48522725533839,3.79));
#43089=CARTESIAN_POINT('Ctrl Pts',(28.0264055269245,1.48522725533839,3.79));
#43090=CARTESIAN_POINT('Ctrl Pts',(28.0545470740907,1.48600415954412,3.7952842627304));
#43091=CARTESIAN_POINT('Ctrl Pts',(28.1062762689051,1.48880073282317,3.81672623696367));
#43092=CARTESIAN_POINT('Ctrl Pts',(28.129866924128,1.49077897157582,3.83288207602961));
#43093=CARTESIAN_POINT('Ctrl Pts',(28.167117678211,1.49448481141327,3.87013283011263));
#43094=CARTESIAN_POINT('Ctrl Pts',(28.1832737100014,1.49645455657129,3.89372359169424));
#43095=CARTESIAN_POINT('Ctrl Pts',(28.2047158248262,1.49923165515646,3.9454531485941));
#43096=CARTESIAN_POINT('Ctrl Pts',(28.21,1.5,3.97359482149072));
#43097=CARTESIAN_POINT('Ctrl Pts',(28.21,1.5,4.02640517850928));
#43098=CARTESIAN_POINT('Ctrl Pts',(28.2047158248262,1.49923165515646,4.0545468514059));
#43099=CARTESIAN_POINT('Ctrl Pts',(28.1832737100014,1.49645455657129,4.10627640830576));
#43100=CARTESIAN_POINT('Ctrl Pts',(28.167117678211,1.49448481141327,4.12986716988737));
#43101=CARTESIAN_POINT('Ctrl Pts',(28.129866924128,1.49077897157582,4.16711792397039));
#43102=CARTESIAN_POINT('Ctrl Pts',(28.1062762689051,1.48880073282317,4.18327376303633));
#43103=CARTESIAN_POINT('Ctrl Pts',(28.0545470740907,1.48600415954412,4.2047157372696));
#43104=CARTESIAN_POINT('Ctrl Pts',(28.0264055269245,1.48522725533839,4.21));
#43105=CARTESIAN_POINT('Ctrl Pts',(28.,1.48522725533839,4.21));
#43106=CARTESIAN_POINT('Origin',(28.,0.99,4.));
#43107=CARTESIAN_POINT('',(27.,0.99,3.85893264020334));
#43108=CARTESIAN_POINT('Origin',(26.9,-0.3,4.));
#43109=CARTESIAN_POINT('',(29.4,-0.3,2.5));
#43110=CARTESIAN_POINT('',(29.4,-0.3,3.04606079858305));
#43111=CARTESIAN_POINT('',(29.4,-0.3,4.));
#43112=CARTESIAN_POINT('',(28.8,-0.3,2.5));
#43113=CARTESIAN_POINT('',(26.9,-0.3,2.5));
#43114=CARTESIAN_POINT('',(28.8,-0.3,2.53030615433009));
#43115=CARTESIAN_POINT('',(28.8,-0.3,4.));
#43116=CARTESIAN_POINT('',(27.,-0.3,2.53030615433009));
#43117=CARTESIAN_POINT('',(27.,-0.3,2.53030615433009));
#43118=CARTESIAN_POINT('',(27.,-0.3,3.04606079858305));
#43119=CARTESIAN_POINT('',(27.,-0.3,4.));
#43120=CARTESIAN_POINT('',(27.,-0.3,3.04606079858305));
#43121=CARTESIAN_POINT('Origin',(26.9,-0.3,2.5));
#43122=CARTESIAN_POINT('',(29.4,0.3,2.5));
#43123=CARTESIAN_POINT('',(29.4,-0.15,2.5));
#43124=CARTESIAN_POINT('',(28.8,0.3,2.5));
#43125=CARTESIAN_POINT('',(26.9,0.3,2.5));
#43126=CARTESIAN_POINT('',(28.8,-0.15,2.5));
#43127=CARTESIAN_POINT('Origin',(26.9,0.3,2.5));
#43128=CARTESIAN_POINT('',(29.4,0.3,3.04606079858305));
#43129=CARTESIAN_POINT('',(29.4,0.3,3.25));
#43130=CARTESIAN_POINT('',(27.,0.3,3.04606079858305));
#43131=CARTESIAN_POINT('',(27.,0.3,3.04606079858305));
#43132=CARTESIAN_POINT('',(27.,0.3,2.53030615433009));
#43133=CARTESIAN_POINT('',(27.,0.3,3.25));
#43134=CARTESIAN_POINT('',(28.8,0.3,2.53030615433009));
#43135=CARTESIAN_POINT('',(27.,0.3,2.53030615433009));
#43136=CARTESIAN_POINT('',(28.8,0.3,3.25));
#43137=CARTESIAN_POINT('Origin',(29.4,0.,4.));
#43138=CARTESIAN_POINT('',(29.4,-4.28626379701574E-16,7.5));
#43139=CARTESIAN_POINT('Origin',(29.4,0.,4.));
#43140=CARTESIAN_POINT('Origin',(29.4,0.,4.));
#43141=CARTESIAN_POINT('Origin',(28.8,0.,4.));
#43142=CARTESIAN_POINT('',(28.8,-4.28626379701574E-16,7.5));
#43143=CARTESIAN_POINT('Origin',(28.8,0.,4.));
#43144=CARTESIAN_POINT('Origin',(28.8,0.,4.));
#43145=CARTESIAN_POINT('Origin',(28.8,0.,4.));
#43146=CARTESIAN_POINT('',(28.8,-4.28626379701574E-16,7.5));
#43147=CARTESIAN_POINT('Origin',(27.,0.,4.));
#43148=CARTESIAN_POINT('Origin',(27.,0.,4.));
#43149=CARTESIAN_POINT('Origin',(27.,0.,4.));
#43150=CARTESIAN_POINT('Origin',(27.,0.,4.));
#43151=CARTESIAN_POINT('Origin',(27.,0.,4.));
#43152=CARTESIAN_POINT('',(0.,0.,0.));
#43153=CARTESIAN_POINT('Origin',(29.4,0.,6.5));
#43154=CARTESIAN_POINT('',(31.03,-4.04133443718627E-17,6.83));
#43155=CARTESIAN_POINT('Origin',(31.03,0.,6.5));
#43156=CARTESIAN_POINT('',(29.4,-4.04133443718627E-17,6.83));
#43157=CARTESIAN_POINT('',(29.4,-4.04133443718627E-17,6.83));
#43158=CARTESIAN_POINT('Origin',(29.4,0.,6.5));
#43159=CARTESIAN_POINT('Origin',(29.4,0.,6.5));
#43160=CARTESIAN_POINT('',(31.03,-4.89858719658942E-17,6.9));
#43161=CARTESIAN_POINT('Origin',(31.03,0.,6.5));
#43162=CARTESIAN_POINT('',(29.4,-4.89858719658942E-17,6.9));
#43163=CARTESIAN_POINT('',(29.4,-4.89858719658942E-17,6.9));
#43164=CARTESIAN_POINT('Origin',(29.4,0.,6.5));
#43165=CARTESIAN_POINT('Origin',(31.03,0.,6.5));
#43166=CARTESIAN_POINT('Origin',(29.4,0.,6.5));
#43167=CARTESIAN_POINT('',(0.,0.,0.));
#43168=CARTESIAN_POINT('Origin',(29.4,0.,6.5));
#43169=CARTESIAN_POINT('',(31.,-4.95981953654678E-17,6.905));
#43170=CARTESIAN_POINT('Origin',(31.,0.,6.5));
#43171=CARTESIAN_POINT('',(29.4,-4.95981953654678E-17,6.905));
#43172=CARTESIAN_POINT('',(29.4,-4.95981953654678E-17,6.905));
#43173=CARTESIAN_POINT('Origin',(29.4,0.,6.5));
#43174=CARTESIAN_POINT('Origin',(29.4,0.,6.5));
#43175=CARTESIAN_POINT('',(31.,-1.10218211923262E-16,7.4));
#43176=CARTESIAN_POINT('Origin',(31.,0.,6.5));
#43177=CARTESIAN_POINT('',(29.4,-1.10218211923262E-16,7.4));
#43178=CARTESIAN_POINT('',(29.4,-1.10218211923262E-16,7.4));
#43179=CARTESIAN_POINT('Origin',(29.4,0.,6.5));
#43180=CARTESIAN_POINT('Origin',(31.,0.,6.5));
#43181=CARTESIAN_POINT('Origin',(29.4,0.,6.5));
#43182=CARTESIAN_POINT('',(0.,0.,0.));
#43183=CARTESIAN_POINT('Origin',(-1.,0.,0.35));
#43184=CARTESIAN_POINT('',(-1.,-0.26,0.6));
#43185=CARTESIAN_POINT('',(-1.,-0.3,0.56));
#43186=CARTESIAN_POINT('',(-1.,-0.2675,0.5925));
#43187=CARTESIAN_POINT('',(-1.,0.26,0.6));
#43188=CARTESIAN_POINT('',(-1.,0.,0.6));
#43189=CARTESIAN_POINT('',(-1.,0.3,0.56));
#43190=CARTESIAN_POINT('',(-1.,0.2675,0.5925));
#43191=CARTESIAN_POINT('',(-1.,0.3,0.04));
#43192=CARTESIAN_POINT('',(-1.,0.3,0.175));
#43193=CARTESIAN_POINT('',(-1.,0.26,0.));
#43194=CARTESIAN_POINT('',(-1.,0.2925,0.0325));
#43195=CARTESIAN_POINT('',(-1.,-0.26,0.));
#43196=CARTESIAN_POINT('',(-1.,0.,0.));
#43197=CARTESIAN_POINT('',(-1.,-0.3,0.04));
#43198=CARTESIAN_POINT('',(-1.,-0.2925,0.0325));
#43199=CARTESIAN_POINT('',(-1.,-0.3,0.175));
#43200=CARTESIAN_POINT('Origin',(0.75,0.28,0.02));
#43201=CARTESIAN_POINT('',(1.,0.3,0.04));
#43202=CARTESIAN_POINT('',(0.75,0.3,0.04));
#43203=CARTESIAN_POINT('',(1.,0.26,0.));
#43204=CARTESIAN_POINT('',(1.,0.2925,0.0325));
#43205=CARTESIAN_POINT('',(0.75,0.26,0.));
#43206=CARTESIAN_POINT('Origin',(1.5,0.3,0.));
#43207=CARTESIAN_POINT('',(1.,0.3,0.56));
#43208=CARTESIAN_POINT('',(0.75,0.3,0.56));
#43209=CARTESIAN_POINT('',(1.,0.3,0.175));
#43210=CARTESIAN_POINT('Origin',(0.75,0.28,0.58));
#43211=CARTESIAN_POINT('',(1.,0.26,0.6));
#43212=CARTESIAN_POINT('',(0.75,0.26,0.6));
#43213=CARTESIAN_POINT('',(1.,0.2675,0.5925));
#43214=CARTESIAN_POINT('Origin',(0.,0.,0.6));
#43215=CARTESIAN_POINT('',(1.,-0.26,0.6));
#43216=CARTESIAN_POINT('',(-0.75,-0.26,0.6));
#43217=CARTESIAN_POINT('',(1.,0.,0.6));
#43218=CARTESIAN_POINT('Origin',(1.,0.,0.35));
#43219=CARTESIAN_POINT('',(1.,-0.26,0.));
#43220=CARTESIAN_POINT('',(1.,-0.3,0.04));
#43221=CARTESIAN_POINT('',(1.,-0.2925,0.0325));
#43222=CARTESIAN_POINT('',(1.,0.,0.));
#43223=CARTESIAN_POINT('',(1.,-0.3,0.56));
#43224=CARTESIAN_POINT('',(1.,-0.2675,0.5925));
#43225=CARTESIAN_POINT('',(1.,-0.3,0.175));
#43226=CARTESIAN_POINT('Origin',(0.,0.,0.));
#43227=CARTESIAN_POINT('',(-0.75,-0.26,0.));
#43228=CARTESIAN_POINT('Origin',(-0.75,-0.28,0.58));
#43229=CARTESIAN_POINT('',(-0.75,-0.3,0.56));
#43230=CARTESIAN_POINT('Origin',(-0.75,-0.28,0.02));
#43231=CARTESIAN_POINT('',(-0.75,-0.3,0.04));
#43232=CARTESIAN_POINT('Origin',(-1.5,-0.3,0.));
#43233=CARTESIAN_POINT('',(0.,0.,0.));
#43234=CARTESIAN_POINT('Origin',(0.0721687836487032,0.,-0.125));
#43235=CARTESIAN_POINT('',(0.0721687836487032,0.,-0.125));
#43236=CARTESIAN_POINT('',(0.144337567297406,0.,0.));
#43237=CARTESIAN_POINT('',(0.117710979560879,0.,-0.0461186027918559));
#43238=CARTESIAN_POINT('',(0.0721687836487032,-0.25,-0.125));
#43239=CARTESIAN_POINT('',(0.0721687836487032,0.,-0.125));
#43240=CARTESIAN_POINT('',(0.144337567297406,-0.25,0.));
#43241=CARTESIAN_POINT('',(0.144337567297406,-0.25,0.));
#43242=CARTESIAN_POINT('',(0.144337567297406,0.,0.));
#43243=CARTESIAN_POINT('Origin',(-0.0721687836487032,0.,-0.125));
#43244=CARTESIAN_POINT('',(-0.0721687836487032,0.,-0.125));
#43245=CARTESIAN_POINT('',(0.0739156081756484,0.,-0.125));
#43246=CARTESIAN_POINT('',(-0.0721687836487032,-0.25,-0.125));
#43247=CARTESIAN_POINT('',(-0.0721687836487032,0.,-0.125));
#43248=CARTESIAN_POINT('',(0.0721687836487032,-0.25,-0.125));
#43249=CARTESIAN_POINT('Origin',(-0.144337567297406,0.,-4.16333634234434E-17));
#43250=CARTESIAN_POINT('',(-0.144337567297406,0.,-1.76762539787485E-17));
#43251=CARTESIAN_POINT('',(-0.0987953713852306,0.,-0.0788813972081442));
#43252=CARTESIAN_POINT('',(-0.144337567297406,-0.25,-2.77555756156289E-17));
#43253=CARTESIAN_POINT('',(-0.144337567297406,0.,-1.76762539787485E-17));
#43254=CARTESIAN_POINT('',(-0.0721687836487032,-0.25,-0.125));
#43255=CARTESIAN_POINT('Origin',(-0.0721687836487033,0.,0.125));
#43256=CARTESIAN_POINT('',(-0.0721687836487033,0.,0.125));
#43257=CARTESIAN_POINT('',(-0.0627109795608791,0.,0.141381397208144));
#43258=CARTESIAN_POINT('',(-0.0721687836487033,-0.25,0.125));
#43259=CARTESIAN_POINT('',(-0.0721687836487033,0.,0.125));
#43260=CARTESIAN_POINT('',(-0.144337567297406,-0.25,-1.76762539787485E-17));
#43261=CARTESIAN_POINT('Origin',(0.0721687836487032,0.,0.125));
#43262=CARTESIAN_POINT('',(0.0721687836487032,0.,0.125));
#43263=CARTESIAN_POINT('',(0.146084391824352,0.,0.125));
#43264=CARTESIAN_POINT('',(0.0721687836487032,-0.25,0.125));
#43265=CARTESIAN_POINT('',(0.0721687836487032,0.,0.125));
#43266=CARTESIAN_POINT('',(-0.0721687836487033,-0.25,0.125));
#43267=CARTESIAN_POINT('Origin',(0.144337567297406,0.,0.));
#43268=CARTESIAN_POINT('',(0.153795371385231,0.,-0.0163813972081441));
#43269=CARTESIAN_POINT('',(0.0721687836487032,-0.25,0.125));
#43270=CARTESIAN_POINT('Origin',(0.,-0.25,0.));
#43271=CARTESIAN_POINT('Origin',(0.22,0.,0.));
#43272=CARTESIAN_POINT('',(-0.22,-8.67361737988404E-18,-2.69422295812418E-17));
#43273=CARTESIAN_POINT('Origin',(0.,0.,0.));
#43274=CARTESIAN_POINT('Origin',(0.,-0.015,0.));
#43275=CARTESIAN_POINT('',(-0.24505,-0.02505,-3.00099698131059E-17));
#43276=CARTESIAN_POINT('Origin',(0.,-0.02505,0.));
#43277=CARTESIAN_POINT('',(-0.235,-0.015,-2.87791997799628E-17));
#43278=CARTESIAN_POINT('Origin',(0.,-0.3775,0.));
#43279=CARTESIAN_POINT('',(-0.24505,-0.72995,3.00099698131059E-17));
#43280=CARTESIAN_POINT('Origin',(0.,-0.72995,0.));
#43281=CARTESIAN_POINT('',(-0.24505,-0.3775,-3.00099698131059E-17));
#43282=CARTESIAN_POINT('Origin',(0.,-0.7625,0.));
#43283=CARTESIAN_POINT('',(-0.175,-0.8,-2.14313189850787E-17));
#43284=CARTESIAN_POINT('Origin',(0.,-0.8,0.));
#43285=CARTESIAN_POINT('',(-0.2125,-0.7625,-2.60237444818813E-17));
#43286=CARTESIAN_POINT('Origin',(0.,-0.8,0.));
#43287=CARTESIAN_POINT('',(0.,0.,0.));
#43288=CARTESIAN_POINT('Origin',(0.,0.,0.));
#43289=CARTESIAN_POINT('',(-0.32,0.16,3.91886975727153E-17));
#43290=CARTESIAN_POINT('Origin',(0.,0.16,0.));
#43291=CARTESIAN_POINT('',(-0.32,0.,3.91886975727153E-17));
#43292=CARTESIAN_POINT('',(-0.32,0.,3.91886975727153E-17));
#43293=CARTESIAN_POINT('Origin',(0.,0.,0.));
#43294=CARTESIAN_POINT('Origin',(0.,0.,0.));
#43295=CARTESIAN_POINT('',(-0.6,0.16,7.34788079488412E-17));
#43296=CARTESIAN_POINT('Origin',(0.,0.16,0.));
#43297=CARTESIAN_POINT('',(-0.6,0.,7.34788079488412E-17));
#43298=CARTESIAN_POINT('',(-0.6,0.,7.34788079488412E-17));
#43299=CARTESIAN_POINT('Origin',(0.,0.,0.));
#43300=CARTESIAN_POINT('Origin',(0.,0.16,0.));
#43301=CARTESIAN_POINT('Origin',(0.,0.,0.));
#43302=CARTESIAN_POINT('',(0.,0.,0.));
#43303=CARTESIAN_POINT('Origin',(0.45,0.6,0.));
#43304=CARTESIAN_POINT('',(-0.45,0.6,-5.51091059616309E-17));
#43305=CARTESIAN_POINT('Origin',(0.,0.6,0.));
#43306=CARTESIAN_POINT('Origin',(0.,0.575,0.));
#43307=CARTESIAN_POINT('',(-0.5,0.55,-6.12323399573677E-17));
#43308=CARTESIAN_POINT('Origin',(0.,0.55,0.));
#43309=CARTESIAN_POINT('',(-0.475,0.575,-5.81707229594993E-17));
#43310=CARTESIAN_POINT('Origin',(0.,0.29,0.));
#43311=CARTESIAN_POINT('',(-0.5,0.0299999999999998,-6.12323399573677E-17));
#43312=CARTESIAN_POINT('Origin',(0.,0.0299999999999998,0.));
#43313=CARTESIAN_POINT('',(-0.5,0.29,-6.12323399573677E-17));
#43314=CARTESIAN_POINT('Origin',(0.,0.0150000000000001,0.));
#43315=CARTESIAN_POINT('',(-0.47,7.11236625150491E-17,-5.75583995599256E-17));
#43316=CARTESIAN_POINT('Origin',(0.,0.,0.));
#43317=CARTESIAN_POINT('',(-0.485,0.0150000000000001,-5.93953697586466E-17));
#43318=CARTESIAN_POINT('Origin',(0.32,0.,0.));
#43319=CARTESIAN_POINT('',(-0.32,-6.93889390390723E-18,-3.91886975727153E-17));
#43320=CARTESIAN_POINT('Origin',(0.,0.,0.));
#43321=CARTESIAN_POINT('Origin',(0.,-0.02,0.));
#43322=CARTESIAN_POINT('',(-0.2942,-0.0515999999999999,3.60291088309151E-17));
#43323=CARTESIAN_POINT('Origin',(0.,-0.0515999999999999,0.));
#43324=CARTESIAN_POINT('',(-0.31,-0.02,-3.7964050773568E-17));
#43325=CARTESIAN_POINT('Origin',(0.,-1.24,0.));
#43326=CARTESIAN_POINT('',(-0.2942,-2.4458,3.60291088309151E-17));
#43327=CARTESIAN_POINT('Origin',(0.,-2.4458,0.));
#43328=CARTESIAN_POINT('',(-0.2942,-1.24,-3.60291088309151E-17));
#43329=CARTESIAN_POINT('Origin',(0.,-2.47,0.));
#43330=CARTESIAN_POINT('',(-0.24,-2.5,-2.93915231795365E-17));
#43331=CARTESIAN_POINT('Origin',(0.,-2.5,0.));
#43332=CARTESIAN_POINT('',(-0.27,-2.47,-3.30654635769785E-17));
#43333=CARTESIAN_POINT('Origin',(0.,-2.5,0.));
#43334=CARTESIAN_POINT('Origin',(0.144337567297406,-0.6,-0.25));
#43335=CARTESIAN_POINT('',(0.288675134594813,-0.6,0.));
#43336=CARTESIAN_POINT('',(0.144337567297406,-0.6,-0.25));
#43337=CARTESIAN_POINT('',(0.288675134594813,-0.6,0.));
#43338=CARTESIAN_POINT('',(0.144337567297406,-0.96,-0.25));
#43339=CARTESIAN_POINT('',(0.144337567297406,-0.6,-0.25));
#43340=CARTESIAN_POINT('',(0.288675134594813,-0.96,0.));
#43341=CARTESIAN_POINT('',(0.288675134594813,-0.96,0.));
#43342=CARTESIAN_POINT('',(0.288675134594813,-0.6,0.));
#43343=CARTESIAN_POINT('Origin',(-0.144337567297406,-0.6,-0.25));
#43344=CARTESIAN_POINT('',(-0.144337567297406,-0.6,-0.25));
#43345=CARTESIAN_POINT('',(0.144337567297406,-0.6,-0.25));
#43346=CARTESIAN_POINT('',(-0.144337567297406,-0.96,-0.25));
#43347=CARTESIAN_POINT('',(-0.144337567297406,-0.6,-0.25));
#43348=CARTESIAN_POINT('',(0.144337567297406,-0.96,-0.25));
#43349=CARTESIAN_POINT('Origin',(-0.288675134594813,-0.6,-8.32667268468867E-17));
#43350=CARTESIAN_POINT('',(-0.288675134594813,-0.6,-3.53525079574969E-17));
#43351=CARTESIAN_POINT('',(-0.144337567297406,-0.6,-0.25));
#43352=CARTESIAN_POINT('',(-0.288675134594813,-0.96,-5.55111512312578E-17));
#43353=CARTESIAN_POINT('',(-0.288675134594813,-0.6,-3.53525079574969E-17));
#43354=CARTESIAN_POINT('',(-0.144337567297406,-0.96,-0.25));
#43355=CARTESIAN_POINT('Origin',(-0.144337567297407,-0.6,0.25));
#43356=CARTESIAN_POINT('',(-0.144337567297407,-0.6,0.25));
#43357=CARTESIAN_POINT('',(-0.288675134594813,-0.6,-3.53525079574969E-17));
#43358=CARTESIAN_POINT('',(-0.144337567297407,-0.96,0.25));
#43359=CARTESIAN_POINT('',(-0.144337567297407,-0.6,0.25));
#43360=CARTESIAN_POINT('',(-0.288675134594813,-0.96,-3.53525079574969E-17));
#43361=CARTESIAN_POINT('Origin',(0.144337567297406,-0.6,0.25));
#43362=CARTESIAN_POINT('',(0.144337567297406,-0.6,0.25));
#43363=CARTESIAN_POINT('',(-0.144337567297407,-0.6,0.25));
#43364=CARTESIAN_POINT('',(0.144337567297406,-0.96,0.25));
#43365=CARTESIAN_POINT('',(0.144337567297406,-0.6,0.25));
#43366=CARTESIAN_POINT('',(-0.144337567297407,-0.96,0.25));
#43367=CARTESIAN_POINT('Origin',(0.288675134594813,-0.6,0.));
#43368=CARTESIAN_POINT('',(0.144337567297406,-0.6,0.25));
#43369=CARTESIAN_POINT('',(0.144337567297406,-0.96,0.25));
#43370=CARTESIAN_POINT('Origin',(0.,-0.6,0.));
#43371=CARTESIAN_POINT('Origin',(0.,-0.96,0.));
#43372=CARTESIAN_POINT('',(0.,0.,0.));
#43373=CARTESIAN_POINT('',(0.,0.,0.));
#43374=CARTESIAN_POINT('',(0.,0.,0.));
#43375=CARTESIAN_POINT('',(0.,0.,0.));
#43376=CARTESIAN_POINT('',(0.,0.,0.));
#43377=CARTESIAN_POINT('',(0.,0.,0.));
#43378=CARTESIAN_POINT('',(28.2,0.,3.35));
#43379=CARTESIAN_POINT('',(25.8,1.8,4.));
#43380=CARTESIAN_POINT('',(28.,1.8,4.));
#43381=CARTESIAN_POINT('',(31.03,0.,6.5));
#43382=CARTESIAN_POINT('',(31.19,0.,6.5));
#43383=CARTESIAN_POINT('',(0.,0.,0.));
#43384=CARTESIAN_POINT('',(0.,0.,0.));
#43385=CARTESIAN_POINT('',(-2.,1.53589838486225,0.));
#43386=UNCERTAINTY_MEASURE_WITH_UNIT(LENGTH_MEASURE(0.001),#43522,
'DISTANCE_ACCURACY_VALUE',
'Maximum model space distance between geometric entities at asserted c
onnectivities');
#43387=UNCERTAINTY_MEASURE_WITH_UNIT(LENGTH_MEASURE(0.001),#43522,
'DISTANCE_ACCURACY_VALUE',
'Maximum model space distance between geometric entities at asserted c
onnectivities');
#43388=UNCERTAINTY_MEASURE_WITH_UNIT(LENGTH_MEASURE(0.001),#43522,
'DISTANCE_ACCURACY_VALUE',
'Maximum model space distance between geometric entities at asserted c
onnectivities');
#43389=UNCERTAINTY_MEASURE_WITH_UNIT(LENGTH_MEASURE(0.001),#43522,
'DISTANCE_ACCURACY_VALUE',
'Maximum model space distance between geometric entities at asserted c
onnectivities');
#43390=UNCERTAINTY_MEASURE_WITH_UNIT(LENGTH_MEASURE(0.001),#43522,
'DISTANCE_ACCURACY_VALUE',
'Maximum model space distance between geometric entities at asserted c
onnectivities');
#43391=UNCERTAINTY_MEASURE_WITH_UNIT(LENGTH_MEASURE(0.001),#43522,
'DISTANCE_ACCURACY_VALUE',
'Maximum model space distance between geometric entities at asserted c
onnectivities');
#43392=UNCERTAINTY_MEASURE_WITH_UNIT(LENGTH_MEASURE(0.001),#43522,
'DISTANCE_ACCURACY_VALUE',
'Maximum model space distance between geometric entities at asserted c
onnectivities');
#43393=UNCERTAINTY_MEASURE_WITH_UNIT(LENGTH_MEASURE(0.001),#43522,
'DISTANCE_ACCURACY_VALUE',
'Maximum model space distance between geometric entities at asserted c
onnectivities');
#43394=UNCERTAINTY_MEASURE_WITH_UNIT(LENGTH_MEASURE(0.001),#43522,
'DISTANCE_ACCURACY_VALUE',
'Maximum model space distance between geometric entities at asserted c
onnectivities');
#43395=UNCERTAINTY_MEASURE_WITH_UNIT(LENGTH_MEASURE(0.001),#43522,
'DISTANCE_ACCURACY_VALUE',
'Maximum model space distance between geometric entities at asserted c
onnectivities');
#43396=UNCERTAINTY_MEASURE_WITH_UNIT(LENGTH_MEASURE(0.001),#43522,
'DISTANCE_ACCURACY_VALUE',
'Maximum model space distance between geometric entities at asserted c
onnectivities');
#43397=UNCERTAINTY_MEASURE_WITH_UNIT(LENGTH_MEASURE(0.001),#43522,
'DISTANCE_ACCURACY_VALUE',
'Maximum model space distance between geometric entities at asserted c
onnectivities');
#43398=UNCERTAINTY_MEASURE_WITH_UNIT(LENGTH_MEASURE(0.001),#43522,
'DISTANCE_ACCURACY_VALUE',
'Maximum model space distance between geometric entities at asserted c
onnectivities');
#43399=UNCERTAINTY_MEASURE_WITH_UNIT(LENGTH_MEASURE(0.001),#43522,
'DISTANCE_ACCURACY_VALUE',
'Maximum model space distance between geometric entities at asserted c
onnectivities');
#43400=UNCERTAINTY_MEASURE_WITH_UNIT(LENGTH_MEASURE(0.001),#43522,
'DISTANCE_ACCURACY_VALUE',
'Maximum model space distance between geometric entities at asserted c
onnectivities');
#43401=UNCERTAINTY_MEASURE_WITH_UNIT(LENGTH_MEASURE(0.001),#43522,
'DISTANCE_ACCURACY_VALUE',
'Maximum model space distance between geometric entities at asserted c
onnectivities');
#43402=UNCERTAINTY_MEASURE_WITH_UNIT(LENGTH_MEASURE(0.001),#43522,
'DISTANCE_ACCURACY_VALUE',
'Maximum model space distance between geometric entities at asserted c
onnectivities');
#43403=UNCERTAINTY_MEASURE_WITH_UNIT(LENGTH_MEASURE(0.001),#43522,
'DISTANCE_ACCURACY_VALUE',
'Maximum model space distance between geometric entities at asserted c
onnectivities');
#43404=UNCERTAINTY_MEASURE_WITH_UNIT(LENGTH_MEASURE(0.001),#43522,
'DISTANCE_ACCURACY_VALUE',
'Maximum model space distance between geometric entities at asserted c
onnectivities');
#43405=UNCERTAINTY_MEASURE_WITH_UNIT(LENGTH_MEASURE(0.001),#43522,
'DISTANCE_ACCURACY_VALUE',
'Maximum model space distance between geometric entities at asserted c
onnectivities');
#43406=UNCERTAINTY_MEASURE_WITH_UNIT(LENGTH_MEASURE(0.001),#43522,
'DISTANCE_ACCURACY_VALUE',
'Maximum model space distance between geometric entities at asserted c
onnectivities');
#43407=UNCERTAINTY_MEASURE_WITH_UNIT(LENGTH_MEASURE(0.001),#43522,
'DISTANCE_ACCURACY_VALUE',
'Maximum model space distance between geometric entities at asserted c
onnectivities');
#43408=UNCERTAINTY_MEASURE_WITH_UNIT(LENGTH_MEASURE(0.001),#43522,
'DISTANCE_ACCURACY_VALUE',
'Maximum model space distance between geometric entities at asserted c
onnectivities');
#43409=UNCERTAINTY_MEASURE_WITH_UNIT(LENGTH_MEASURE(0.001),#43522,
'DISTANCE_ACCURACY_VALUE',
'Maximum model space distance between geometric entities at asserted c
onnectivities');
#43410=UNCERTAINTY_MEASURE_WITH_UNIT(LENGTH_MEASURE(0.001),#43522,
'DISTANCE_ACCURACY_VALUE',
'Maximum model space distance between geometric entities at asserted c
onnectivities');
#43411=UNCERTAINTY_MEASURE_WITH_UNIT(LENGTH_MEASURE(0.001),#43522,
'DISTANCE_ACCURACY_VALUE',
'Maximum model space distance between geometric entities at asserted c
onnectivities');
#43412=UNCERTAINTY_MEASURE_WITH_UNIT(LENGTH_MEASURE(0.001),#43522,
'DISTANCE_ACCURACY_VALUE',
'Maximum model space distance between geometric entities at asserted c
onnectivities');
#43413=UNCERTAINTY_MEASURE_WITH_UNIT(LENGTH_MEASURE(0.001),#43522,
'DISTANCE_ACCURACY_VALUE',
'Maximum model space distance between geometric entities at asserted c
onnectivities');
#43414=UNCERTAINTY_MEASURE_WITH_UNIT(LENGTH_MEASURE(0.001),#43522,
'DISTANCE_ACCURACY_VALUE',
'Maximum model space distance between geometric entities at asserted c
onnectivities');
#43415=UNCERTAINTY_MEASURE_WITH_UNIT(LENGTH_MEASURE(0.001),#43522,
'DISTANCE_ACCURACY_VALUE',
'Maximum model space distance between geometric entities at asserted c
onnectivities');
#43416=UNCERTAINTY_MEASURE_WITH_UNIT(LENGTH_MEASURE(0.001),#43522,
'DISTANCE_ACCURACY_VALUE',
'Maximum model space distance between geometric entities at asserted c
onnectivities');
#43417=UNCERTAINTY_MEASURE_WITH_UNIT(LENGTH_MEASURE(0.001),#43522,
'DISTANCE_ACCURACY_VALUE',
'Maximum model space distance between geometric entities at asserted c
onnectivities');
#43418=UNCERTAINTY_MEASURE_WITH_UNIT(LENGTH_MEASURE(0.001),#43522,
'DISTANCE_ACCURACY_VALUE',
'Maximum model space distance between geometric entities at asserted c
onnectivities');
#43419=UNCERTAINTY_MEASURE_WITH_UNIT(LENGTH_MEASURE(0.001),#43522,
'DISTANCE_ACCURACY_VALUE',
'Maximum model space distance between geometric entities at asserted c
onnectivities');
#43420=UNCERTAINTY_MEASURE_WITH_UNIT(LENGTH_MEASURE(0.001),#43522,
'DISTANCE_ACCURACY_VALUE',
'Maximum model space distance between geometric entities at asserted c
onnectivities');
#43421=UNCERTAINTY_MEASURE_WITH_UNIT(LENGTH_MEASURE(0.001),#43522,
'DISTANCE_ACCURACY_VALUE',
'Maximum model space distance between geometric entities at asserted c
onnectivities');
#43422=UNCERTAINTY_MEASURE_WITH_UNIT(LENGTH_MEASURE(0.001),#43522,
'DISTANCE_ACCURACY_VALUE',
'Maximum model space distance between geometric entities at asserted c
onnectivities');
#43423=UNCERTAINTY_MEASURE_WITH_UNIT(LENGTH_MEASURE(0.001),#43522,
'DISTANCE_ACCURACY_VALUE',
'Maximum model space distance between geometric entities at asserted c
onnectivities');
#43424=UNCERTAINTY_MEASURE_WITH_UNIT(LENGTH_MEASURE(0.001),#43522,
'DISTANCE_ACCURACY_VALUE',
'Maximum model space distance between geometric entities at asserted c
onnectivities');
#43425=UNCERTAINTY_MEASURE_WITH_UNIT(LENGTH_MEASURE(0.001),#43522,
'DISTANCE_ACCURACY_VALUE',
'Maximum model space distance between geometric entities at asserted c
onnectivities');
#43426=UNCERTAINTY_MEASURE_WITH_UNIT(LENGTH_MEASURE(0.001),#43522,
'DISTANCE_ACCURACY_VALUE',
'Maximum model space distance between geometric entities at asserted c
onnectivities');
#43427=UNCERTAINTY_MEASURE_WITH_UNIT(LENGTH_MEASURE(0.001),#43522,
'DISTANCE_ACCURACY_VALUE',
'Maximum model space distance between geometric entities at asserted c
onnectivities');
#43428=UNCERTAINTY_MEASURE_WITH_UNIT(LENGTH_MEASURE(0.001),#43522,
'DISTANCE_ACCURACY_VALUE',
'Maximum model space distance between geometric entities at asserted c
onnectivities');
#43429=UNCERTAINTY_MEASURE_WITH_UNIT(LENGTH_MEASURE(0.001),#43522,
'DISTANCE_ACCURACY_VALUE',
'Maximum model space distance between geometric entities at asserted c
onnectivities');
#43430=UNCERTAINTY_MEASURE_WITH_UNIT(LENGTH_MEASURE(0.001),#43522,
'DISTANCE_ACCURACY_VALUE',
'Maximum model space distance between geometric entities at asserted c
onnectivities');
#43431=UNCERTAINTY_MEASURE_WITH_UNIT(LENGTH_MEASURE(0.001),#43522,
'DISTANCE_ACCURACY_VALUE',
'Maximum model space distance between geometric entities at asserted c
onnectivities');
#43432=UNCERTAINTY_MEASURE_WITH_UNIT(LENGTH_MEASURE(0.001),#43522,
'DISTANCE_ACCURACY_VALUE',
'Maximum model space distance between geometric entities at asserted c
onnectivities');
#43433=UNCERTAINTY_MEASURE_WITH_UNIT(LENGTH_MEASURE(0.001),#43522,
'DISTANCE_ACCURACY_VALUE',
'Maximum model space distance between geometric entities at asserted c
onnectivities');
#43434=UNCERTAINTY_MEASURE_WITH_UNIT(LENGTH_MEASURE(0.001),#43522,
'DISTANCE_ACCURACY_VALUE',
'Maximum model space distance between geometric entities at asserted c
onnectivities');
#43435=UNCERTAINTY_MEASURE_WITH_UNIT(LENGTH_MEASURE(0.001),#43522,
'DISTANCE_ACCURACY_VALUE',
'Maximum model space distance between geometric entities at asserted c
onnectivities');
#43436=UNCERTAINTY_MEASURE_WITH_UNIT(LENGTH_MEASURE(0.001),#43522,
'DISTANCE_ACCURACY_VALUE',
'Maximum model space distance between geometric entities at asserted c
onnectivities');
#43437=UNCERTAINTY_MEASURE_WITH_UNIT(LENGTH_MEASURE(0.001),#43522,
'DISTANCE_ACCURACY_VALUE',
'Maximum model space distance between geometric entities at asserted c
onnectivities');
#43438=UNCERTAINTY_MEASURE_WITH_UNIT(LENGTH_MEASURE(0.001),#43522,
'DISTANCE_ACCURACY_VALUE',
'Maximum model space distance between geometric entities at asserted c
onnectivities');
#43439=UNCERTAINTY_MEASURE_WITH_UNIT(LENGTH_MEASURE(0.001),#43522,
'DISTANCE_ACCURACY_VALUE',
'Maximum model space distance between geometric entities at asserted c
onnectivities');
#43440=UNCERTAINTY_MEASURE_WITH_UNIT(LENGTH_MEASURE(0.001),#43522,
'DISTANCE_ACCURACY_VALUE',
'Maximum model space distance between geometric entities at asserted c
onnectivities');
#43441=UNCERTAINTY_MEASURE_WITH_UNIT(LENGTH_MEASURE(0.001),#43522,
'DISTANCE_ACCURACY_VALUE',
'Maximum model space distance between geometric entities at asserted c
onnectivities');
#43442=UNCERTAINTY_MEASURE_WITH_UNIT(LENGTH_MEASURE(0.001),#43522,
'DISTANCE_ACCURACY_VALUE',
'Maximum model space distance between geometric entities at asserted c
onnectivities');
#43443=UNCERTAINTY_MEASURE_WITH_UNIT(LENGTH_MEASURE(0.001),#43522,
'DISTANCE_ACCURACY_VALUE',
'Maximum model space distance between geometric entities at asserted c
onnectivities');
#43444=UNCERTAINTY_MEASURE_WITH_UNIT(LENGTH_MEASURE(0.001),#43522,
'DISTANCE_ACCURACY_VALUE',
'Maximum model space distance between geometric entities at asserted c
onnectivities');
#43445=UNCERTAINTY_MEASURE_WITH_UNIT(LENGTH_MEASURE(0.001),#43522,
'DISTANCE_ACCURACY_VALUE',
'Maximum model space distance between geometric entities at asserted c
onnectivities');
#43446=UNCERTAINTY_MEASURE_WITH_UNIT(LENGTH_MEASURE(0.001),#43522,
'DISTANCE_ACCURACY_VALUE',
'Maximum model space distance between geometric entities at asserted c
onnectivities');
#43447=UNCERTAINTY_MEASURE_WITH_UNIT(LENGTH_MEASURE(0.001),#43522,
'DISTANCE_ACCURACY_VALUE',
'Maximum model space distance between geometric entities at asserted c
onnectivities');
#43448=UNCERTAINTY_MEASURE_WITH_UNIT(LENGTH_MEASURE(0.001),#43522,
'DISTANCE_ACCURACY_VALUE',
'Maximum model space distance between geometric entities at asserted c
onnectivities');
#43449=UNCERTAINTY_MEASURE_WITH_UNIT(LENGTH_MEASURE(0.001),#43522,
'DISTANCE_ACCURACY_VALUE',
'Maximum model space distance between geometric entities at asserted c
onnectivities');
#43450=UNCERTAINTY_MEASURE_WITH_UNIT(LENGTH_MEASURE(0.001),#43522,
'DISTANCE_ACCURACY_VALUE',
'Maximum model space distance between geometric entities at asserted c
onnectivities');
#43451=UNCERTAINTY_MEASURE_WITH_UNIT(LENGTH_MEASURE(0.001),#43522,
'DISTANCE_ACCURACY_VALUE',
'Maximum model space distance between geometric entities at asserted c
onnectivities');
#43452=UNCERTAINTY_MEASURE_WITH_UNIT(LENGTH_MEASURE(0.001),#43522,
'DISTANCE_ACCURACY_VALUE',
'Maximum model space distance between geometric entities at asserted c
onnectivities');
#43453=UNCERTAINTY_MEASURE_WITH_UNIT(LENGTH_MEASURE(0.001),#43522,
'DISTANCE_ACCURACY_VALUE',
'Maximum model space distance between geometric entities at asserted c
onnectivities');
#43454=(
GEOMETRIC_REPRESENTATION_CONTEXT(3)
GLOBAL_UNCERTAINTY_ASSIGNED_CONTEXT((#43386))
GLOBAL_UNIT_ASSIGNED_CONTEXT((#43522,#43524,#43525))
REPRESENTATION_CONTEXT('','3D')
);
#43455=(
GEOMETRIC_REPRESENTATION_CONTEXT(3)
GLOBAL_UNCERTAINTY_ASSIGNED_CONTEXT((#43387))
GLOBAL_UNIT_ASSIGNED_CONTEXT((#43522,#43524,#43525))
REPRESENTATION_CONTEXT('','3D')
);
#43456=(
GEOMETRIC_REPRESENTATION_CONTEXT(3)
GLOBAL_UNCERTAINTY_ASSIGNED_CONTEXT((#43388))
GLOBAL_UNIT_ASSIGNED_CONTEXT((#43522,#43524,#43525))
REPRESENTATION_CONTEXT('','3D')
);
#43457=(
GEOMETRIC_REPRESENTATION_CONTEXT(3)
GLOBAL_UNCERTAINTY_ASSIGNED_CONTEXT((#43389))
GLOBAL_UNIT_ASSIGNED_CONTEXT((#43522,#43524,#43525))
REPRESENTATION_CONTEXT('','3D')
);
#43458=(
GEOMETRIC_REPRESENTATION_CONTEXT(3)
GLOBAL_UNCERTAINTY_ASSIGNED_CONTEXT((#43390))
GLOBAL_UNIT_ASSIGNED_CONTEXT((#43522,#43524,#43525))
REPRESENTATION_CONTEXT('','3D')
);
#43459=(
GEOMETRIC_REPRESENTATION_CONTEXT(3)
GLOBAL_UNCERTAINTY_ASSIGNED_CONTEXT((#43391))
GLOBAL_UNIT_ASSIGNED_CONTEXT((#43522,#43524,#43525))
REPRESENTATION_CONTEXT('','3D')
);
#43460=(
GEOMETRIC_REPRESENTATION_CONTEXT(3)
GLOBAL_UNCERTAINTY_ASSIGNED_CONTEXT((#43392))
GLOBAL_UNIT_ASSIGNED_CONTEXT((#43522,#43524,#43525))
REPRESENTATION_CONTEXT('','3D')
);
#43461=(
GEOMETRIC_REPRESENTATION_CONTEXT(3)
GLOBAL_UNCERTAINTY_ASSIGNED_CONTEXT((#43393))
GLOBAL_UNIT_ASSIGNED_CONTEXT((#43522,#43524,#43525))
REPRESENTATION_CONTEXT('','3D')
);
#43462=(
GEOMETRIC_REPRESENTATION_CONTEXT(3)
GLOBAL_UNCERTAINTY_ASSIGNED_CONTEXT((#43394))
GLOBAL_UNIT_ASSIGNED_CONTEXT((#43522,#43524,#43525))
REPRESENTATION_CONTEXT('','3D')
);
#43463=(
GEOMETRIC_REPRESENTATION_CONTEXT(3)
GLOBAL_UNCERTAINTY_ASSIGNED_CONTEXT((#43395))
GLOBAL_UNIT_ASSIGNED_CONTEXT((#43522,#43524,#43525))
REPRESENTATION_CONTEXT('','3D')
);
#43464=(
GEOMETRIC_REPRESENTATION_CONTEXT(3)
GLOBAL_UNCERTAINTY_ASSIGNED_CONTEXT((#43396))
GLOBAL_UNIT_ASSIGNED_CONTEXT((#43522,#43524,#43525))
REPRESENTATION_CONTEXT('','3D')
);
#43465=(
GEOMETRIC_REPRESENTATION_CONTEXT(3)
GLOBAL_UNCERTAINTY_ASSIGNED_CONTEXT((#43397))
GLOBAL_UNIT_ASSIGNED_CONTEXT((#43522,#43524,#43525))
REPRESENTATION_CONTEXT('','3D')
);
#43466=(
GEOMETRIC_REPRESENTATION_CONTEXT(3)
GLOBAL_UNCERTAINTY_ASSIGNED_CONTEXT((#43398))
GLOBAL_UNIT_ASSIGNED_CONTEXT((#43522,#43524,#43525))
REPRESENTATION_CONTEXT('','3D')
);
#43467=(
GEOMETRIC_REPRESENTATION_CONTEXT(3)
GLOBAL_UNCERTAINTY_ASSIGNED_CONTEXT((#43399))
GLOBAL_UNIT_ASSIGNED_CONTEXT((#43522,#43524,#43525))
REPRESENTATION_CONTEXT('','3D')
);
#43468=(
GEOMETRIC_REPRESENTATION_CONTEXT(3)
GLOBAL_UNCERTAINTY_ASSIGNED_CONTEXT((#43400))
GLOBAL_UNIT_ASSIGNED_CONTEXT((#43522,#43524,#43525))
REPRESENTATION_CONTEXT('','3D')
);
#43469=(
GEOMETRIC_REPRESENTATION_CONTEXT(3)
GLOBAL_UNCERTAINTY_ASSIGNED_CONTEXT((#43401))
GLOBAL_UNIT_ASSIGNED_CONTEXT((#43522,#43524,#43525))
REPRESENTATION_CONTEXT('','3D')
);
#43470=(
GEOMETRIC_REPRESENTATION_CONTEXT(3)
GLOBAL_UNCERTAINTY_ASSIGNED_CONTEXT((#43402))
GLOBAL_UNIT_ASSIGNED_CONTEXT((#43522,#43524,#43525))
REPRESENTATION_CONTEXT('','3D')
);
#43471=(
GEOMETRIC_REPRESENTATION_CONTEXT(3)
GLOBAL_UNCERTAINTY_ASSIGNED_CONTEXT((#43403))
GLOBAL_UNIT_ASSIGNED_CONTEXT((#43522,#43524,#43525))
REPRESENTATION_CONTEXT('','3D')
);
#43472=(
GEOMETRIC_REPRESENTATION_CONTEXT(3)
GLOBAL_UNCERTAINTY_ASSIGNED_CONTEXT((#43404))
GLOBAL_UNIT_ASSIGNED_CONTEXT((#43522,#43524,#43525))
REPRESENTATION_CONTEXT('','3D')
);
#43473=(
GEOMETRIC_REPRESENTATION_CONTEXT(3)
GLOBAL_UNCERTAINTY_ASSIGNED_CONTEXT((#43405))
GLOBAL_UNIT_ASSIGNED_CONTEXT((#43522,#43524,#43525))
REPRESENTATION_CONTEXT('','3D')
);
#43474=(
GEOMETRIC_REPRESENTATION_CONTEXT(3)
GLOBAL_UNCERTAINTY_ASSIGNED_CONTEXT((#43406))
GLOBAL_UNIT_ASSIGNED_CONTEXT((#43522,#43524,#43525))
REPRESENTATION_CONTEXT('','3D')
);
#43475=(
GEOMETRIC_REPRESENTATION_CONTEXT(3)
GLOBAL_UNCERTAINTY_ASSIGNED_CONTEXT((#43407))
GLOBAL_UNIT_ASSIGNED_CONTEXT((#43522,#43524,#43525))
REPRESENTATION_CONTEXT('','3D')
);
#43476=(
GEOMETRIC_REPRESENTATION_CONTEXT(3)
GLOBAL_UNCERTAINTY_ASSIGNED_CONTEXT((#43408))
GLOBAL_UNIT_ASSIGNED_CONTEXT((#43522,#43524,#43525))
REPRESENTATION_CONTEXT('','3D')
);
#43477=(
GEOMETRIC_REPRESENTATION_CONTEXT(3)
GLOBAL_UNCERTAINTY_ASSIGNED_CONTEXT((#43409))
GLOBAL_UNIT_ASSIGNED_CONTEXT((#43522,#43524,#43525))
REPRESENTATION_CONTEXT('','3D')
);
#43478=(
GEOMETRIC_REPRESENTATION_CONTEXT(3)
GLOBAL_UNCERTAINTY_ASSIGNED_CONTEXT((#43410))
GLOBAL_UNIT_ASSIGNED_CONTEXT((#43522,#43524,#43525))
REPRESENTATION_CONTEXT('','3D')
);
#43479=(
GEOMETRIC_REPRESENTATION_CONTEXT(3)
GLOBAL_UNCERTAINTY_ASSIGNED_CONTEXT((#43411))
GLOBAL_UNIT_ASSIGNED_CONTEXT((#43522,#43524,#43525))
REPRESENTATION_CONTEXT('','3D')
);
#43480=(
GEOMETRIC_REPRESENTATION_CONTEXT(3)
GLOBAL_UNCERTAINTY_ASSIGNED_CONTEXT((#43412))
GLOBAL_UNIT_ASSIGNED_CONTEXT((#43522,#43524,#43525))
REPRESENTATION_CONTEXT('','3D')
);
#43481=(
GEOMETRIC_REPRESENTATION_CONTEXT(3)
GLOBAL_UNCERTAINTY_ASSIGNED_CONTEXT((#43413))
GLOBAL_UNIT_ASSIGNED_CONTEXT((#43522,#43524,#43525))
REPRESENTATION_CONTEXT('','3D')
);
#43482=(
GEOMETRIC_REPRESENTATION_CONTEXT(3)
GLOBAL_UNCERTAINTY_ASSIGNED_CONTEXT((#43414))
GLOBAL_UNIT_ASSIGNED_CONTEXT((#43522,#43524,#43525))
REPRESENTATION_CONTEXT('','3D')
);
#43483=(
GEOMETRIC_REPRESENTATION_CONTEXT(3)
GLOBAL_UNCERTAINTY_ASSIGNED_CONTEXT((#43415))
GLOBAL_UNIT_ASSIGNED_CONTEXT((#43522,#43524,#43525))
REPRESENTATION_CONTEXT('','3D')
);
#43484=(
GEOMETRIC_REPRESENTATION_CONTEXT(3)
GLOBAL_UNCERTAINTY_ASSIGNED_CONTEXT((#43416))
GLOBAL_UNIT_ASSIGNED_CONTEXT((#43522,#43524,#43525))
REPRESENTATION_CONTEXT('','3D')
);
#43485=(
GEOMETRIC_REPRESENTATION_CONTEXT(3)
GLOBAL_UNCERTAINTY_ASSIGNED_CONTEXT((#43417))
GLOBAL_UNIT_ASSIGNED_CONTEXT((#43522,#43524,#43525))
REPRESENTATION_CONTEXT('','3D')
);
#43486=(
GEOMETRIC_REPRESENTATION_CONTEXT(3)
GLOBAL_UNCERTAINTY_ASSIGNED_CONTEXT((#43418))
GLOBAL_UNIT_ASSIGNED_CONTEXT((#43522,#43524,#43525))
REPRESENTATION_CONTEXT('','3D')
);
#43487=(
GEOMETRIC_REPRESENTATION_CONTEXT(3)
GLOBAL_UNCERTAINTY_ASSIGNED_CONTEXT((#43419))
GLOBAL_UNIT_ASSIGNED_CONTEXT((#43522,#43524,#43525))
REPRESENTATION_CONTEXT('','3D')
);
#43488=(
GEOMETRIC_REPRESENTATION_CONTEXT(3)
GLOBAL_UNCERTAINTY_ASSIGNED_CONTEXT((#43420))
GLOBAL_UNIT_ASSIGNED_CONTEXT((#43522,#43524,#43525))
REPRESENTATION_CONTEXT('','3D')
);
#43489=(
GEOMETRIC_REPRESENTATION_CONTEXT(3)
GLOBAL_UNCERTAINTY_ASSIGNED_CONTEXT((#43421))
GLOBAL_UNIT_ASSIGNED_CONTEXT((#43522,#43524,#43525))
REPRESENTATION_CONTEXT('','3D')
);
#43490=(
GEOMETRIC_REPRESENTATION_CONTEXT(3)
GLOBAL_UNCERTAINTY_ASSIGNED_CONTEXT((#43422))
GLOBAL_UNIT_ASSIGNED_CONTEXT((#43522,#43524,#43525))
REPRESENTATION_CONTEXT('','3D')
);
#43491=(
GEOMETRIC_REPRESENTATION_CONTEXT(3)
GLOBAL_UNCERTAINTY_ASSIGNED_CONTEXT((#43423))
GLOBAL_UNIT_ASSIGNED_CONTEXT((#43522,#43524,#43525))
REPRESENTATION_CONTEXT('','3D')
);
#43492=(
GEOMETRIC_REPRESENTATION_CONTEXT(3)
GLOBAL_UNCERTAINTY_ASSIGNED_CONTEXT((#43424))
GLOBAL_UNIT_ASSIGNED_CONTEXT((#43522,#43524,#43525))
REPRESENTATION_CONTEXT('','3D')
);
#43493=(
GEOMETRIC_REPRESENTATION_CONTEXT(3)
GLOBAL_UNCERTAINTY_ASSIGNED_CONTEXT((#43425))
GLOBAL_UNIT_ASSIGNED_CONTEXT((#43522,#43524,#43525))
REPRESENTATION_CONTEXT('','3D')
);
#43494=(
GEOMETRIC_REPRESENTATION_CONTEXT(3)
GLOBAL_UNCERTAINTY_ASSIGNED_CONTEXT((#43426))
GLOBAL_UNIT_ASSIGNED_CONTEXT((#43522,#43524,#43525))
REPRESENTATION_CONTEXT('','3D')
);
#43495=(
GEOMETRIC_REPRESENTATION_CONTEXT(3)
GLOBAL_UNCERTAINTY_ASSIGNED_CONTEXT((#43427))
GLOBAL_UNIT_ASSIGNED_CONTEXT((#43522,#43524,#43525))
REPRESENTATION_CONTEXT('','3D')
);
#43496=(
GEOMETRIC_REPRESENTATION_CONTEXT(3)
GLOBAL_UNCERTAINTY_ASSIGNED_CONTEXT((#43428))
GLOBAL_UNIT_ASSIGNED_CONTEXT((#43522,#43524,#43525))
REPRESENTATION_CONTEXT('','3D')
);
#43497=(
GEOMETRIC_REPRESENTATION_CONTEXT(3)
GLOBAL_UNCERTAINTY_ASSIGNED_CONTEXT((#43429))
GLOBAL_UNIT_ASSIGNED_CONTEXT((#43522,#43524,#43525))
REPRESENTATION_CONTEXT('','3D')
);
#43498=(
GEOMETRIC_REPRESENTATION_CONTEXT(3)
GLOBAL_UNCERTAINTY_ASSIGNED_CONTEXT((#43430))
GLOBAL_UNIT_ASSIGNED_CONTEXT((#43522,#43524,#43525))
REPRESENTATION_CONTEXT('','3D')
);
#43499=(
GEOMETRIC_REPRESENTATION_CONTEXT(3)
GLOBAL_UNCERTAINTY_ASSIGNED_CONTEXT((#43431))
GLOBAL_UNIT_ASSIGNED_CONTEXT((#43522,#43524,#43525))
REPRESENTATION_CONTEXT('','3D')
);
#43500=(
GEOMETRIC_REPRESENTATION_CONTEXT(3)
GLOBAL_UNCERTAINTY_ASSIGNED_CONTEXT((#43432))
GLOBAL_UNIT_ASSIGNED_CONTEXT((#43522,#43524,#43525))
REPRESENTATION_CONTEXT('','3D')
);
#43501=(
GEOMETRIC_REPRESENTATION_CONTEXT(3)
GLOBAL_UNCERTAINTY_ASSIGNED_CONTEXT((#43433))
GLOBAL_UNIT_ASSIGNED_CONTEXT((#43522,#43524,#43525))
REPRESENTATION_CONTEXT('','3D')
);
#43502=(
GEOMETRIC_REPRESENTATION_CONTEXT(3)
GLOBAL_UNCERTAINTY_ASSIGNED_CONTEXT((#43434))
GLOBAL_UNIT_ASSIGNED_CONTEXT((#43522,#43524,#43525))
REPRESENTATION_CONTEXT('','3D')
);
#43503=(
GEOMETRIC_REPRESENTATION_CONTEXT(3)
GLOBAL_UNCERTAINTY_ASSIGNED_CONTEXT((#43435))
GLOBAL_UNIT_ASSIGNED_CONTEXT((#43522,#43524,#43525))
REPRESENTATION_CONTEXT('','3D')
);
#43504=(
GEOMETRIC_REPRESENTATION_CONTEXT(3)
GLOBAL_UNCERTAINTY_ASSIGNED_CONTEXT((#43436))
GLOBAL_UNIT_ASSIGNED_CONTEXT((#43522,#43524,#43525))
REPRESENTATION_CONTEXT('','3D')
);
#43505=(
GEOMETRIC_REPRESENTATION_CONTEXT(3)
GLOBAL_UNCERTAINTY_ASSIGNED_CONTEXT((#43437))
GLOBAL_UNIT_ASSIGNED_CONTEXT((#43522,#43524,#43525))
REPRESENTATION_CONTEXT('','3D')
);
#43506=(
GEOMETRIC_REPRESENTATION_CONTEXT(3)
GLOBAL_UNCERTAINTY_ASSIGNED_CONTEXT((#43438))
GLOBAL_UNIT_ASSIGNED_CONTEXT((#43522,#43524,#43525))
REPRESENTATION_CONTEXT('','3D')
);
#43507=(
GEOMETRIC_REPRESENTATION_CONTEXT(3)
GLOBAL_UNCERTAINTY_ASSIGNED_CONTEXT((#43439))
GLOBAL_UNIT_ASSIGNED_CONTEXT((#43522,#43524,#43525))
REPRESENTATION_CONTEXT('','3D')
);
#43508=(
GEOMETRIC_REPRESENTATION_CONTEXT(3)
GLOBAL_UNCERTAINTY_ASSIGNED_CONTEXT((#43440))
GLOBAL_UNIT_ASSIGNED_CONTEXT((#43522,#43524,#43525))
REPRESENTATION_CONTEXT('','3D')
);
#43509=(
GEOMETRIC_REPRESENTATION_CONTEXT(3)
GLOBAL_UNCERTAINTY_ASSIGNED_CONTEXT((#43441))
GLOBAL_UNIT_ASSIGNED_CONTEXT((#43522,#43524,#43525))
REPRESENTATION_CONTEXT('','3D')
);
#43510=(
GEOMETRIC_REPRESENTATION_CONTEXT(3)
GLOBAL_UNCERTAINTY_ASSIGNED_CONTEXT((#43442))
GLOBAL_UNIT_ASSIGNED_CONTEXT((#43522,#43524,#43525))
REPRESENTATION_CONTEXT('','3D')
);
#43511=(
GEOMETRIC_REPRESENTATION_CONTEXT(3)
GLOBAL_UNCERTAINTY_ASSIGNED_CONTEXT((#43443))
GLOBAL_UNIT_ASSIGNED_CONTEXT((#43522,#43524,#43525))
REPRESENTATION_CONTEXT('','3D')
);
#43512=(
GEOMETRIC_REPRESENTATION_CONTEXT(3)
GLOBAL_UNCERTAINTY_ASSIGNED_CONTEXT((#43444))
GLOBAL_UNIT_ASSIGNED_CONTEXT((#43522,#43524,#43525))
REPRESENTATION_CONTEXT('','3D')
);
#43513=(
GEOMETRIC_REPRESENTATION_CONTEXT(3)
GLOBAL_UNCERTAINTY_ASSIGNED_CONTEXT((#43445))
GLOBAL_UNIT_ASSIGNED_CONTEXT((#43522,#43524,#43525))
REPRESENTATION_CONTEXT('','3D')
);
#43514=(
GEOMETRIC_REPRESENTATION_CONTEXT(3)
GLOBAL_UNCERTAINTY_ASSIGNED_CONTEXT((#43446))
GLOBAL_UNIT_ASSIGNED_CONTEXT((#43522,#43524,#43525))
REPRESENTATION_CONTEXT('','3D')
);
#43515=(
GEOMETRIC_REPRESENTATION_CONTEXT(3)
GLOBAL_UNCERTAINTY_ASSIGNED_CONTEXT((#43447))
GLOBAL_UNIT_ASSIGNED_CONTEXT((#43522,#43524,#43525))
REPRESENTATION_CONTEXT('','3D')
);
#43516=(
GEOMETRIC_REPRESENTATION_CONTEXT(3)
GLOBAL_UNCERTAINTY_ASSIGNED_CONTEXT((#43448))
GLOBAL_UNIT_ASSIGNED_CONTEXT((#43522,#43524,#43525))
REPRESENTATION_CONTEXT('','3D')
);
#43517=(
GEOMETRIC_REPRESENTATION_CONTEXT(3)
GLOBAL_UNCERTAINTY_ASSIGNED_CONTEXT((#43449))
GLOBAL_UNIT_ASSIGNED_CONTEXT((#43522,#43524,#43525))
REPRESENTATION_CONTEXT('','3D')
);
#43518=(
GEOMETRIC_REPRESENTATION_CONTEXT(3)
GLOBAL_UNCERTAINTY_ASSIGNED_CONTEXT((#43450))
GLOBAL_UNIT_ASSIGNED_CONTEXT((#43522,#43524,#43525))
REPRESENTATION_CONTEXT('','3D')
);
#43519=(
GEOMETRIC_REPRESENTATION_CONTEXT(3)
GLOBAL_UNCERTAINTY_ASSIGNED_CONTEXT((#43451))
GLOBAL_UNIT_ASSIGNED_CONTEXT((#43522,#43524,#43525))
REPRESENTATION_CONTEXT('','3D')
);
#43520=(
GEOMETRIC_REPRESENTATION_CONTEXT(3)
GLOBAL_UNCERTAINTY_ASSIGNED_CONTEXT((#43452))
GLOBAL_UNIT_ASSIGNED_CONTEXT((#43522,#43524,#43525))
REPRESENTATION_CONTEXT('','3D')
);
#43521=(
GEOMETRIC_REPRESENTATION_CONTEXT(3)
GLOBAL_UNCERTAINTY_ASSIGNED_CONTEXT((#43453))
GLOBAL_UNIT_ASSIGNED_CONTEXT((#43522,#43524,#43525))
REPRESENTATION_CONTEXT('','3D')
);
#43522=(
LENGTH_UNIT()
NAMED_UNIT(*)
SI_UNIT(.CENTI.,.METRE.)
);
#43523=(
LENGTH_UNIT()
NAMED_UNIT(*)
SI_UNIT($,.METRE.)
);
#43524=(
NAMED_UNIT(*)
PLANE_ANGLE_UNIT()
SI_UNIT($,.RADIAN.)
);
#43525=(
NAMED_UNIT(*)
SI_UNIT($,.STERADIAN.)
SOLID_ANGLE_UNIT()
);
#43526=SHAPE_DEFINITION_REPRESENTATION(#43593,#43794);
#43527=SHAPE_DEFINITION_REPRESENTATION(#43594,#43795);
#43528=SHAPE_DEFINITION_REPRESENTATION(#43595,#43796);
#43529=SHAPE_DEFINITION_REPRESENTATION(#43596,#43797);
#43530=SHAPE_DEFINITION_REPRESENTATION(#43597,#43798);
#43531=SHAPE_DEFINITION_REPRESENTATION(#43598,#43799);
#43532=SHAPE_DEFINITION_REPRESENTATION(#43599,#43800);
#43533=SHAPE_DEFINITION_REPRESENTATION(#43600,#43801);
#43534=SHAPE_DEFINITION_REPRESENTATION(#43601,#43802);
#43535=SHAPE_DEFINITION_REPRESENTATION(#43602,#43803);
#43536=SHAPE_DEFINITION_REPRESENTATION(#43603,#43804);
#43537=SHAPE_DEFINITION_REPRESENTATION(#43604,#43805);
#43538=SHAPE_DEFINITION_REPRESENTATION(#43605,#43806);
#43539=SHAPE_DEFINITION_REPRESENTATION(#43606,#43807);
#43540=SHAPE_DEFINITION_REPRESENTATION(#43607,#43808);
#43541=SHAPE_DEFINITION_REPRESENTATION(#43608,#43809);
#43542=SHAPE_DEFINITION_REPRESENTATION(#43609,#43810);
#43543=SHAPE_DEFINITION_REPRESENTATION(#43610,#43811);
#43544=SHAPE_DEFINITION_REPRESENTATION(#43611,#43812);
#43545=SHAPE_DEFINITION_REPRESENTATION(#43612,#43813);
#43546=SHAPE_DEFINITION_REPRESENTATION(#43613,#43814);
#43547=SHAPE_DEFINITION_REPRESENTATION(#43614,#43815);
#43548=SHAPE_DEFINITION_REPRESENTATION(#43615,#43816);
#43549=SHAPE_DEFINITION_REPRESENTATION(#43616,#43817);
#43550=SHAPE_DEFINITION_REPRESENTATION(#43617,#43818);
#43551=SHAPE_DEFINITION_REPRESENTATION(#43618,#43819);
#43552=SHAPE_DEFINITION_REPRESENTATION(#43619,#43820);
#43553=SHAPE_DEFINITION_REPRESENTATION(#43620,#43821);
#43554=SHAPE_DEFINITION_REPRESENTATION(#43621,#43822);
#43555=SHAPE_DEFINITION_REPRESENTATION(#43622,#43823);
#43556=SHAPE_DEFINITION_REPRESENTATION(#43623,#43824);
#43557=SHAPE_DEFINITION_REPRESENTATION(#43629,#43825);
#43558=SHAPE_DEFINITION_REPRESENTATION(#43630,#43826);
#43559=SHAPE_DEFINITION_REPRESENTATION(#43631,#43827);
#43560=SHAPE_DEFINITION_REPRESENTATION(#43632,#43828);
#43561=SHAPE_DEFINITION_REPRESENTATION(#43633,#43829);
#43562=SHAPE_DEFINITION_REPRESENTATION(#43634,#43830);
#43563=SHAPE_DEFINITION_REPRESENTATION(#43640,#43831);
#43564=SHAPE_DEFINITION_REPRESENTATION(#43641,#43832);
#43565=SHAPE_DEFINITION_REPRESENTATION(#43642,#43833);
#43566=SHAPE_DEFINITION_REPRESENTATION(#43643,#43834);
#43567=SHAPE_DEFINITION_REPRESENTATION(#43644,#43835);
#43568=SHAPE_DEFINITION_REPRESENTATION(#43645,#43836);
#43569=SHAPE_DEFINITION_REPRESENTATION(#43646,#43837);
#43570=SHAPE_DEFINITION_REPRESENTATION(#43647,#43838);
#43571=SHAPE_DEFINITION_REPRESENTATION(#43648,#43839);
#43572=SHAPE_DEFINITION_REPRESENTATION(#43649,#43840);
#43573=SHAPE_DEFINITION_REPRESENTATION(#43650,#43841);
#43574=SHAPE_DEFINITION_REPRESENTATION(#43651,#43842);
#43575=SHAPE_DEFINITION_REPRESENTATION(#43652,#43843);
#43576=SHAPE_DEFINITION_REPRESENTATION(#43653,#43844);
#43577=SHAPE_DEFINITION_REPRESENTATION(#43654,#43845);
#43578=SHAPE_DEFINITION_REPRESENTATION(#43655,#43846);
#43579=SHAPE_DEFINITION_REPRESENTATION(#43658,#43847);
#43580=SHAPE_DEFINITION_REPRESENTATION(#43659,#43848);
#43581=SHAPE_DEFINITION_REPRESENTATION(#43660,#43849);
#43582=SHAPE_DEFINITION_REPRESENTATION(#43769,#43850);
#43583=SHAPE_DEFINITION_REPRESENTATION(#43770,#43851);
#43584=SHAPE_DEFINITION_REPRESENTATION(#43771,#43852);
#43585=SHAPE_DEFINITION_REPRESENTATION(#43772,#43853);
#43586=SHAPE_DEFINITION_REPRESENTATION(#43773,#43854);
#43587=SHAPE_DEFINITION_REPRESENTATION(#43774,#43855);
#43588=SHAPE_DEFINITION_REPRESENTATION(#43775,#43856);
#43589=SHAPE_DEFINITION_REPRESENTATION(#43776,#43857);
#43590=SHAPE_DEFINITION_REPRESENTATION(#43777,#43858);
#43591=SHAPE_DEFINITION_REPRESENTATION(#43778,#43859);
#43592=SHAPE_DEFINITION_REPRESENTATION(#43779,#43860);
#43593=PRODUCT_DEFINITION_SHAPE('',$,#43862);
#43594=PRODUCT_DEFINITION_SHAPE('',$,#43863);
#43595=PRODUCT_DEFINITION_SHAPE('',$,#43864);
#43596=PRODUCT_DEFINITION_SHAPE('',$,#43865);
#43597=PRODUCT_DEFINITION_SHAPE('',$,#43866);
#43598=PRODUCT_DEFINITION_SHAPE('',$,#43867);
#43599=PRODUCT_DEFINITION_SHAPE('',$,#43868);
#43600=PRODUCT_DEFINITION_SHAPE('',$,#43869);
#43601=PRODUCT_DEFINITION_SHAPE('',$,#43870);
#43602=PRODUCT_DEFINITION_SHAPE('',$,#43871);
#43603=PRODUCT_DEFINITION_SHAPE('',$,#43872);
#43604=PRODUCT_DEFINITION_SHAPE('',$,#43873);
#43605=PRODUCT_DEFINITION_SHAPE('',$,#43874);
#43606=PRODUCT_DEFINITION_SHAPE('',$,#43875);
#43607=PRODUCT_DEFINITION_SHAPE('',$,#43876);
#43608=PRODUCT_DEFINITION_SHAPE('',$,#43877);
#43609=PRODUCT_DEFINITION_SHAPE('',$,#43878);
#43610=PRODUCT_DEFINITION_SHAPE('',$,#43879);
#43611=PRODUCT_DEFINITION_SHAPE('',$,#43880);
#43612=PRODUCT_DEFINITION_SHAPE('',$,#43881);
#43613=PRODUCT_DEFINITION_SHAPE('',$,#43882);
#43614=PRODUCT_DEFINITION_SHAPE('',$,#43883);
#43615=PRODUCT_DEFINITION_SHAPE('',$,#43884);
#43616=PRODUCT_DEFINITION_SHAPE('',$,#43885);
#43617=PRODUCT_DEFINITION_SHAPE('',$,#43886);
#43618=PRODUCT_DEFINITION_SHAPE('',$,#43887);
#43619=PRODUCT_DEFINITION_SHAPE('',$,#43888);
#43620=PRODUCT_DEFINITION_SHAPE('',$,#43889);
#43621=PRODUCT_DEFINITION_SHAPE('',$,#43890);
#43622=PRODUCT_DEFINITION_SHAPE('',$,#43891);
#43623=PRODUCT_DEFINITION_SHAPE('',$,#43892);
#43624=PRODUCT_DEFINITION_SHAPE($,$,#419);
#43625=PRODUCT_DEFINITION_SHAPE($,$,#420);
#43626=PRODUCT_DEFINITION_SHAPE($,$,#421);
#43627=PRODUCT_DEFINITION_SHAPE($,$,#422);
#43628=PRODUCT_DEFINITION_SHAPE($,$,#423);
#43629=PRODUCT_DEFINITION_SHAPE('',$,#43893);
#43630=PRODUCT_DEFINITION_SHAPE('',$,#43894);
#43631=PRODUCT_DEFINITION_SHAPE('',$,#43895);
#43632=PRODUCT_DEFINITION_SHAPE('',$,#43896);
#43633=PRODUCT_DEFINITION_SHAPE('',$,#43897);
#43634=PRODUCT_DEFINITION_SHAPE('',$,#43898);
#43635=PRODUCT_DEFINITION_SHAPE($,$,#424);
#43636=PRODUCT_DEFINITION_SHAPE($,$,#425);
#43637=PRODUCT_DEFINITION_SHAPE($,$,#426);
#43638=PRODUCT_DEFINITION_SHAPE($,$,#427);
#43639=PRODUCT_DEFINITION_SHAPE($,$,#428);
#43640=PRODUCT_DEFINITION_SHAPE('',$,#43899);
#43641=PRODUCT_DEFINITION_SHAPE('',$,#43900);
#43642=PRODUCT_DEFINITION_SHAPE('',$,#43901);
#43643=PRODUCT_DEFINITION_SHAPE('',$,#43902);
#43644=PRODUCT_DEFINITION_SHAPE('',$,#43903);
#43645=PRODUCT_DEFINITION_SHAPE('',$,#43904);
#43646=PRODUCT_DEFINITION_SHAPE('',$,#43905);
#43647=PRODUCT_DEFINITION_SHAPE('',$,#43906);
#43648=PRODUCT_DEFINITION_SHAPE('',$,#43907);
#43649=PRODUCT_DEFINITION_SHAPE('',$,#43908);
#43650=PRODUCT_DEFINITION_SHAPE('',$,#43909);
#43651=PRODUCT_DEFINITION_SHAPE('',$,#43910);
#43652=PRODUCT_DEFINITION_SHAPE('',$,#43911);
#43653=PRODUCT_DEFINITION_SHAPE('',$,#43912);
#43654=PRODUCT_DEFINITION_SHAPE('',$,#43913);
#43655=PRODUCT_DEFINITION_SHAPE('',$,#43914);
#43656=PRODUCT_DEFINITION_SHAPE($,$,#429);
#43657=PRODUCT_DEFINITION_SHAPE($,$,#430);
#43658=PRODUCT_DEFINITION_SHAPE('',$,#43915);
#43659=PRODUCT_DEFINITION_SHAPE('',$,#43916);
#43660=PRODUCT_DEFINITION_SHAPE('',$,#43917);
#43661=PRODUCT_DEFINITION_SHAPE($,$,#431);
#43662=PRODUCT_DEFINITION_SHAPE($,$,#432);
#43663=PRODUCT_DEFINITION_SHAPE($,$,#433);
#43664=PRODUCT_DEFINITION_SHAPE($,$,#434);
#43665=PRODUCT_DEFINITION_SHAPE($,$,#435);
#43666=PRODUCT_DEFINITION_SHAPE($,$,#436);
#43667=PRODUCT_DEFINITION_SHAPE($,$,#437);
#43668=PRODUCT_DEFINITION_SHAPE($,$,#438);
#43669=PRODUCT_DEFINITION_SHAPE($,$,#439);
#43670=PRODUCT_DEFINITION_SHAPE($,$,#440);
#43671=PRODUCT_DEFINITION_SHAPE($,$,#441);
#43672=PRODUCT_DEFINITION_SHAPE($,$,#442);
#43673=PRODUCT_DEFINITION_SHAPE($,$,#443);
#43674=PRODUCT_DEFINITION_SHAPE($,$,#444);
#43675=PRODUCT_DEFINITION_SHAPE($,$,#445);
#43676=PRODUCT_DEFINITION_SHAPE($,$,#446);
#43677=PRODUCT_DEFINITION_SHAPE($,$,#447);
#43678=PRODUCT_DEFINITION_SHAPE($,$,#448);
#43679=PRODUCT_DEFINITION_SHAPE($,$,#449);
#43680=PRODUCT_DEFINITION_SHAPE($,$,#450);
#43681=PRODUCT_DEFINITION_SHAPE($,$,#451);
#43682=PRODUCT_DEFINITION_SHAPE($,$,#452);
#43683=PRODUCT_DEFINITION_SHAPE($,$,#453);
#43684=PRODUCT_DEFINITION_SHAPE($,$,#454);
#43685=PRODUCT_DEFINITION_SHAPE($,$,#455);
#43686=PRODUCT_DEFINITION_SHAPE($,$,#456);
#43687=PRODUCT_DEFINITION_SHAPE($,$,#457);
#43688=PRODUCT_DEFINITION_SHAPE($,$,#458);
#43689=PRODUCT_DEFINITION_SHAPE($,$,#459);
#43690=PRODUCT_DEFINITION_SHAPE($,$,#460);
#43691=PRODUCT_DEFINITION_SHAPE($,$,#461);
#43692=PRODUCT_DEFINITION_SHAPE($,$,#462);
#43693=PRODUCT_DEFINITION_SHAPE($,$,#463);
#43694=PRODUCT_DEFINITION_SHAPE($,$,#464);
#43695=PRODUCT_DEFINITION_SHAPE($,$,#465);
#43696=PRODUCT_DEFINITION_SHAPE($,$,#466);
#43697=PRODUCT_DEFINITION_SHAPE($,$,#467);
#43698=PRODUCT_DEFINITION_SHAPE($,$,#468);
#43699=PRODUCT_DEFINITION_SHAPE($,$,#469);
#43700=PRODUCT_DEFINITION_SHAPE($,$,#470);
#43701=PRODUCT_DEFINITION_SHAPE($,$,#471);
#43702=PRODUCT_DEFINITION_SHAPE($,$,#472);
#43703=PRODUCT_DEFINITION_SHAPE($,$,#473);
#43704=PRODUCT_DEFINITION_SHAPE($,$,#474);
#43705=PRODUCT_DEFINITION_SHAPE($,$,#475);
#43706=PRODUCT_DEFINITION_SHAPE($,$,#476);
#43707=PRODUCT_DEFINITION_SHAPE($,$,#477);
#43708=PRODUCT_DEFINITION_SHAPE($,$,#478);
#43709=PRODUCT_DEFINITION_SHAPE($,$,#479);
#43710=PRODUCT_DEFINITION_SHAPE($,$,#480);
#43711=PRODUCT_DEFINITION_SHAPE($,$,#481);
#43712=PRODUCT_DEFINITION_SHAPE($,$,#482);
#43713=PRODUCT_DEFINITION_SHAPE($,$,#483);
#43714=PRODUCT_DEFINITION_SHAPE($,$,#484);
#43715=PRODUCT_DEFINITION_SHAPE($,$,#485);
#43716=PRODUCT_DEFINITION_SHAPE($,$,#486);
#43717=PRODUCT_DEFINITION_SHAPE($,$,#487);
#43718=PRODUCT_DEFINITION_SHAPE($,$,#488);
#43719=PRODUCT_DEFINITION_SHAPE($,$,#489);
#43720=PRODUCT_DEFINITION_SHAPE($,$,#490);
#43721=PRODUCT_DEFINITION_SHAPE($,$,#491);
#43722=PRODUCT_DEFINITION_SHAPE($,$,#492);
#43723=PRODUCT_DEFINITION_SHAPE($,$,#493);
#43724=PRODUCT_DEFINITION_SHAPE($,$,#494);
#43725=PRODUCT_DEFINITION_SHAPE($,$,#495);
#43726=PRODUCT_DEFINITION_SHAPE($,$,#496);
#43727=PRODUCT_DEFINITION_SHAPE($,$,#497);
#43728=PRODUCT_DEFINITION_SHAPE($,$,#498);
#43729=PRODUCT_DEFINITION_SHAPE($,$,#499);
#43730=PRODUCT_DEFINITION_SHAPE($,$,#500);
#43731=PRODUCT_DEFINITION_SHAPE($,$,#501);
#43732=PRODUCT_DEFINITION_SHAPE($,$,#502);
#43733=PRODUCT_DEFINITION_SHAPE($,$,#503);
#43734=PRODUCT_DEFINITION_SHAPE($,$,#504);
#43735=PRODUCT_DEFINITION_SHAPE($,$,#505);
#43736=PRODUCT_DEFINITION_SHAPE($,$,#506);
#43737=PRODUCT_DEFINITION_SHAPE($,$,#507);
#43738=PRODUCT_DEFINITION_SHAPE($,$,#508);
#43739=PRODUCT_DEFINITION_SHAPE($,$,#509);
#43740=PRODUCT_DEFINITION_SHAPE($,$,#510);
#43741=PRODUCT_DEFINITION_SHAPE($,$,#511);
#43742=PRODUCT_DEFINITION_SHAPE($,$,#512);
#43743=PRODUCT_DEFINITION_SHAPE($,$,#513);
#43744=PRODUCT_DEFINITION_SHAPE($,$,#514);
#43745=PRODUCT_DEFINITION_SHAPE($,$,#515);
#43746=PRODUCT_DEFINITION_SHAPE($,$,#516);
#43747=PRODUCT_DEFINITION_SHAPE($,$,#517);
#43748=PRODUCT_DEFINITION_SHAPE($,$,#518);
#43749=PRODUCT_DEFINITION_SHAPE($,$,#519);
#43750=PRODUCT_DEFINITION_SHAPE($,$,#520);
#43751=PRODUCT_DEFINITION_SHAPE($,$,#521);
#43752=PRODUCT_DEFINITION_SHAPE($,$,#522);
#43753=PRODUCT_DEFINITION_SHAPE($,$,#523);
#43754=PRODUCT_DEFINITION_SHAPE($,$,#524);
#43755=PRODUCT_DEFINITION_SHAPE($,$,#525);
#43756=PRODUCT_DEFINITION_SHAPE($,$,#526);
#43757=PRODUCT_DEFINITION_SHAPE($,$,#527);
#43758=PRODUCT_DEFINITION_SHAPE($,$,#528);
#43759=PRODUCT_DEFINITION_SHAPE($,$,#529);
#43760=PRODUCT_DEFINITION_SHAPE($,$,#530);
#43761=PRODUCT_DEFINITION_SHAPE($,$,#531);
#43762=PRODUCT_DEFINITION_SHAPE($,$,#532);
#43763=PRODUCT_DEFINITION_SHAPE($,$,#533);
#43764=PRODUCT_DEFINITION_SHAPE($,$,#534);
#43765=PRODUCT_DEFINITION_SHAPE($,$,#535);
#43766=PRODUCT_DEFINITION_SHAPE($,$,#536);
#43767=PRODUCT_DEFINITION_SHAPE($,$,#537);
#43768=PRODUCT_DEFINITION_SHAPE($,$,#538);
#43769=PRODUCT_DEFINITION_SHAPE('',$,#43918);
#43770=PRODUCT_DEFINITION_SHAPE('',$,#43919);
#43771=PRODUCT_DEFINITION_SHAPE('',$,#43920);
#43772=PRODUCT_DEFINITION_SHAPE('',$,#43921);
#43773=PRODUCT_DEFINITION_SHAPE('',$,#43922);
#43774=PRODUCT_DEFINITION_SHAPE('',$,#43923);
#43775=PRODUCT_DEFINITION_SHAPE('',$,#43924);
#43776=PRODUCT_DEFINITION_SHAPE('',$,#43925);
#43777=PRODUCT_DEFINITION_SHAPE('',$,#43926);
#43778=PRODUCT_DEFINITION_SHAPE('',$,#43927);
#43779=PRODUCT_DEFINITION_SHAPE('',$,#43928);
#43780=PRODUCT_DEFINITION_SHAPE($,$,#539);
#43781=PRODUCT_DEFINITION_SHAPE($,$,#540);
#43782=PRODUCT_DEFINITION_SHAPE($,$,#541);
#43783=PRODUCT_DEFINITION_SHAPE($,$,#542);
#43784=PRODUCT_DEFINITION_SHAPE($,$,#543);
#43785=PRODUCT_DEFINITION_SHAPE($,$,#544);
#43786=PRODUCT_DEFINITION_SHAPE($,$,#545);
#43787=PRODUCT_DEFINITION_SHAPE($,$,#546);
#43788=PRODUCT_DEFINITION_SHAPE($,$,#547);
#43789=PRODUCT_DEFINITION_SHAPE($,$,#548);
#43790=PRODUCT_DEFINITION_SHAPE($,$,#549);
#43791=PRODUCT_DEFINITION_SHAPE($,$,#550);
#43792=PRODUCT_DEFINITION_SHAPE($,$,#551);
#43793=PRODUCT_DEFINITION_SHAPE($,$,#552);
#43794=SHAPE_REPRESENTATION('',(#19284,#21193,#21194,#21195),#43454);
#43795=SHAPE_REPRESENTATION('',(#19285,#20790,#20791,#20792,#20793,#20794,
#20795,#20796,#20797,#20798,#20799,#20800,#20801,#20802,#20803,#20804,#20805,
#20806,#20807,#20808,#20809,#20810,#20811,#20812,#20813,#20814,#20815,#20816,
#20817,#20818,#20819,#20820,#20821,#20822,#20823,#20824,#20825,#20826,#20827,
#20828,#20829,#20830,#20831,#20832,#20833,#20834,#20835,#20836,#20837,#20838,
#20839,#20840,#20841,#20842,#20843,#20844,#20845,#20846,#20847,#20848,#20849,
#20850,#20851,#20852,#20853,#20854,#20855,#20856,#20857,#20858,#20859,#20860,
#20861,#20862,#20863,#20864,#20865,#20866,#20867,#20868,#20869,#20870,#20871,
#20872,#20873),#43455);
#43796=SHAPE_REPRESENTATION('',(#19286),#43456);
#43797=SHAPE_REPRESENTATION('',(#19361),#43457);
#43798=SHAPE_REPRESENTATION('',(#19368),#43458);
#43799=SHAPE_REPRESENTATION('',(#19375),#43459);
#43800=SHAPE_REPRESENTATION('',(#19416),#43460);
#43801=SHAPE_REPRESENTATION('',(#19445),#43461);
#43802=SHAPE_REPRESENTATION('',(#19474),#43462);
#43803=SHAPE_REPRESENTATION('',(#19495),#43463);
#43804=SHAPE_REPRESENTATION('',(#19522),#43464);
#43805=SHAPE_REPRESENTATION('',(#19543),#43465);
#43806=SHAPE_REPRESENTATION('',(#19570),#43466);
#43807=SHAPE_REPRESENTATION('',(#19613),#43467);
#43808=SHAPE_REPRESENTATION('',(#19664),#43468);
#43809=SHAPE_REPRESENTATION('',(#19686),#43469);
#43810=SHAPE_REPRESENTATION('',(#19708),#43470);
#43811=SHAPE_REPRESENTATION('',(#19718),#43471);
#43812=SHAPE_REPRESENTATION('',(#19728),#43472);
#43813=SHAPE_REPRESENTATION('',(#19738),#43473);
#43814=SHAPE_REPRESENTATION('',(#19748),#43474);
#43815=SHAPE_REPRESENTATION('',(#19782),#43475);
#43816=SHAPE_REPRESENTATION('',(#19920),#43476);
#43817=SHAPE_REPRESENTATION('',(#19930),#43477);
#43818=SHAPE_REPRESENTATION('',(#19968),#43478);
#43819=SHAPE_REPRESENTATION('',(#19992,#20115,#20116,#20117,#20118,#20119),
#43479);
#43820=SHAPE_REPRESENTATION('',(#19993),#43480);
#43821=SHAPE_REPRESENTATION('',(#20013),#43481);
#43822=SHAPE_REPRESENTATION('',(#20033),#43482);
#43823=SHAPE_REPRESENTATION('',(#20048),#43483);
#43824=SHAPE_REPRESENTATION('',(#20098),#43484);
#43825=SHAPE_REPRESENTATION('',(#20120,#20249,#20250,#20251,#20252,#20253),
#43485);
#43826=SHAPE_REPRESENTATION('',(#20121),#43486);
#43827=SHAPE_REPRESENTATION('',(#20141),#43487);
#43828=SHAPE_REPRESENTATION('',(#20161),#43488);
#43829=SHAPE_REPRESENTATION('',(#20178),#43489);
#43830=SHAPE_REPRESENTATION('',(#20232),#43490);
#43831=SHAPE_REPRESENTATION('',(#20254),#43491);
#43832=SHAPE_REPRESENTATION('',(#20282),#43492);
#43833=SHAPE_REPRESENTATION('',(#20306),#43493);
#43834=SHAPE_REPRESENTATION('',(#20356),#43494);
#43835=SHAPE_REPRESENTATION('',(#20382),#43495);
#43836=SHAPE_REPRESENTATION('',(#20403),#43496);
#43837=SHAPE_REPRESENTATION('',(#20426,#20874,#20875,#20876,#20877,#20878,
#20879,#20880,#20881,#20882,#20883,#20884,#20885,#20886,#20887,#20888,#20889,
#20890,#20891,#20892,#20893,#20894,#20895,#20896,#20897),#43497);
#43838=SHAPE_REPRESENTATION('',(#20427),#43498);
#43839=SHAPE_REPRESENTATION('',(#20488),#43499);
#43840=SHAPE_REPRESENTATION('',(#20537),#43500);
#43841=SHAPE_REPRESENTATION('',(#20586),#43501);
#43842=SHAPE_REPRESENTATION('',(#20607),#43502);
#43843=SHAPE_REPRESENTATION('',(#20619),#43503);
#43844=SHAPE_REPRESENTATION('',(#20639,#20689,#20690),#43504);
#43845=SHAPE_REPRESENTATION('',(#20640),#43505);
#43846=SHAPE_REPRESENTATION('',(#20672),#43506);
#43847=SHAPE_REPRESENTATION('',(#20691),#43507);
#43848=SHAPE_REPRESENTATION('',(#20736),#43508);
#43849=SHAPE_REPRESENTATION('',(#20764),#43509);
#43850=SHAPE_REPRESENTATION('',(#20898,#21182,#21183,#21184,#21185,#21186,
#21187,#21188,#21189,#21190,#21191,#21192),#43510);
#43851=SHAPE_REPRESENTATION('',(#20899),#43511);
#43852=SHAPE_REPRESENTATION('',(#21054),#43512);
#43853=SHAPE_REPRESENTATION('',(#21063),#43513);
#43854=SHAPE_REPRESENTATION('',(#21077),#43514);
#43855=SHAPE_REPRESENTATION('',(#21101),#43515);
#43856=SHAPE_REPRESENTATION('',(#21110),#43516);
#43857=SHAPE_REPRESENTATION('',(#21119),#43517);
#43858=SHAPE_REPRESENTATION('',(#21130),#43518);
#43859=SHAPE_REPRESENTATION('',(#21147),#43519);
#43860=SHAPE_REPRESENTATION('',(#21156),#43520);
#43861=PRODUCT_DEFINITION_CONTEXT('part definition',#44064,'design');
#43862=PRODUCT_DEFINITION('PAT-098','PAT-098',#43929,
#43861);
#43863=PRODUCT_DEFINITION('Guide frame and screw bearings',
'Guide frame and screw bearings',#43930,#43861);
#43864=PRODUCT_DEFINITION('Base','Base',#43931,#43861);
#43865=PRODUCT_DEFINITION('Foot strip','Foot strip',#43932,#43861);
#43866=PRODUCT_DEFINITION('Foot strip (1)','Foot strip (1)',#43933,#43861);
#43867=PRODUCT_DEFINITION('Top guide plate','Top guide plate',#43934,#43861);
#43868=PRODUCT_DEFINITION('Frame upright','Frame upright',#43935,#43861);
#43869=PRODUCT_DEFINITION('Frame upright (1)','Frame upright (1)',#43936,
#43861);
#43870=PRODUCT_DEFINITION('Lower guide bracket','Lower guide bracket',#43937,
#43861);
#43871=PRODUCT_DEFINITION('Upper guide bracket','Upper guide bracket',#43938,
#43861);
#43872=PRODUCT_DEFINITION('Lower guide bracket (1)',
'Lower guide bracket (1)',#43939,#43861);
#43873=PRODUCT_DEFINITION('Upper guide bracket (1)',
'Upper guide bracket (1)',#43940,#43861);
#43874=PRODUCT_DEFINITION('Floating bearing pedestal',
'Floating bearing pedestal',#43941,#43861);
#43875=PRODUCT_DEFINITION('Fixed bearing crossbar',
'Fixed bearing crossbar',#43942,#43861);
#43876=PRODUCT_DEFINITION('Floating bearing cap','Floating bearing cap',
#43943,#43861);
#43877=PRODUCT_DEFINITION('Fixed bearing cap','Fixed bearing cap',#43944,
#43861);
#43878=PRODUCT_DEFINITION('Lower travel stop','Lower travel stop',#43945,
#43861);
#43879=PRODUCT_DEFINITION('Upper travel stop','Upper travel stop',#43946,
#43861);
#43880=PRODUCT_DEFINITION('Lower travel stop (1)','Lower travel stop (1)',
#43947,#43861);
#43881=PRODUCT_DEFINITION('Upper travel stop (1)','Upper travel stop (1)',
#43948,#43861);
#43882=PRODUCT_DEFINITION('Lower compression platen',
'Lower compression platen',#43949,#43861);
#43883=PRODUCT_DEFINITION('Graduated scale','Graduated scale',#43950,#43861);
#43884=PRODUCT_DEFINITION(
'Precision Shaft - 12 mm Diameter, 300 mm Long',
'Precision Shaft - 12 mm Diameter, 300 mm Long',#43951,#43861);
#43885=PRODUCT_DEFINITION('Shaft Support - 12 mm Bore',
'Shaft Support - 12 mm Bore',#43952,#43861);
#43886=PRODUCT_DEFINITION('M5x14 Cap Screw','M5x14 Cap Screw',#43953,#43861);
#43887=PRODUCT_DEFINITION('Sealed Ball Bearing - 12 x 32 x 10 mm',
'Sealed Ball Bearing - 12 x 32 x 10 mm',#43954,#43861);
#43888=PRODUCT_DEFINITION('Inner ring','Inner ring',#43955,#43861);
#43889=PRODUCT_DEFINITION('Outer ring','Outer ring',#43956,#43861);
#43890=PRODUCT_DEFINITION('Balls','Balls',#43957,#43861);
#43891=PRODUCT_DEFINITION('Cage','Cage',#43958,#43861);
#43892=PRODUCT_DEFINITION('Seals 2RS','Seals 2RS',#43959,#43861);
#43893=PRODUCT_DEFINITION('Sealed Ball Bearing - 20 x 47 x 14 mm',
'Sealed Ball Bearing - 20 x 47 x 14 mm',#43960,#43861);
#43894=PRODUCT_DEFINITION('Inner ring (1)','Inner ring (1)',#43961,#43861);
#43895=PRODUCT_DEFINITION('Outer ring (1)','Outer ring (1)',#43962,#43861);
#43896=PRODUCT_DEFINITION('Balls (1)','Balls (1)',#43963,#43861);
#43897=PRODUCT_DEFINITION('Cage (1)','Cage (1)',#43964,#43861);
#43898=PRODUCT_DEFINITION('Seals 2RS (1)','Seals 2RS (1)',#43965,#43861);
#43899=PRODUCT_DEFINITION('M5x25 stop screw','M5x25 stop screw',#43966,
#43861);
#43900=PRODUCT_DEFINITION('M4x10 Cap Screw','M4x10 Cap Screw',#43967,#43861);
#43901=PRODUCT_DEFINITION('Slotted Extrusion - 20 x 20 x 400 mm',
'Slotted Extrusion - 20 x 20 x 400 mm',#43968,#43861);
#43902=PRODUCT_DEFINITION('Cap Screw - M5x20','Cap Screw - M5x20',#43969,
#43861);
#43903=PRODUCT_DEFINITION('Captive slot nut','Captive slot nut',#43970,
#43861);
#43904=PRODUCT_DEFINITION('M5x8 ruler screw','M5x8 ruler screw',#43971,
#43861);
#43905=PRODUCT_DEFINITION('Platform and lead nut',
'Platform and lead nut',#43972,#43861);
#43906=PRODUCT_DEFINITION('Platform','Platform',#43973,#43861);
#43907=PRODUCT_DEFINITION('Linear bushing housing',
'Linear bushing housing',#43974,#43861);
#43908=PRODUCT_DEFINITION('Linear bushing housing (1)',
'Linear bushing housing (1)',#43975,#43861);
#43909=PRODUCT_DEFINITION('Nut carrier','Nut carrier',#43976,#43861);
#43910=PRODUCT_DEFINITION('Upper compression platen',
'Upper compression platen',#43977,#43861);
#43911=PRODUCT_DEFINITION('Scale pointer','Scale pointer',#43978,#43861);
#43912=PRODUCT_DEFINITION('Linear Ball Bushing - 12 x 21 x 30 mm',
'Linear Ball Bushing - 12 x 21 x 30 mm',#43979,#43861);
#43913=PRODUCT_DEFINITION('Steel sleeve','Steel sleeve',#43980,#43861);
#43914=PRODUCT_DEFINITION('Ball retainer (plastic)',
'Ball retainer (plastic)',#43981,#43861);
#43915=PRODUCT_DEFINITION('Flanged lead nut','Flanged lead nut',#43982,
#43861);
#43916=PRODUCT_DEFINITION('M4x30 nut screw','M4x30 nut screw',#43983,#43861);
#43917=PRODUCT_DEFINITION('Cap Screw - M4x16','Cap Screw - M4x16',#43984,
#43861);
#43918=PRODUCT_DEFINITION('Vertical screw and handwheel',
'Vertical screw and handwheel',#43985,#43861);
#43919=PRODUCT_DEFINITION('Supported TR12x3 screw',
'Supported TR12x3 screw',#43986,#43861);
#43920=PRODUCT_DEFINITION('Inner race spacer','Inner race spacer',#43987,
#43861);
#43921=PRODUCT_DEFINITION('Shaft retaining collar',
'Shaft retaining collar',#43988,#43861);
#43922=PRODUCT_DEFINITION('Handwheel','Handwheel',#43989,#43861);
#43923=PRODUCT_DEFINITION('Handle pivot sleeve','Handle pivot sleeve',#43990,
#43861);
#43924=PRODUCT_DEFINITION('Revolving handle','Revolving handle',#43991,
#43861);
#43925=PRODUCT_DEFINITION('Key 6x6x20','Key 6x6x20',#43992,#43861);
#43926=PRODUCT_DEFINITION('Socket Set Screw - M5x8',
'Socket Set Screw - M5x8',#43993,#43861);
#43927=PRODUCT_DEFINITION('Flat Washer - M6','Flat Washer - M6',#43994,
#43861);
#43928=PRODUCT_DEFINITION('Cap Screw - M6x25','Cap Screw - M6x25',#43995,
#43861);
#43929=PRODUCT_DEFINITION_FORMATION('',$,#44066);
#43930=PRODUCT_DEFINITION_FORMATION('',$,#44067);
#43931=PRODUCT_DEFINITION_FORMATION('',$,#44068);
#43932=PRODUCT_DEFINITION_FORMATION('',$,#44069);
#43933=PRODUCT_DEFINITION_FORMATION('',$,#44070);
#43934=PRODUCT_DEFINITION_FORMATION('',$,#44071);
#43935=PRODUCT_DEFINITION_FORMATION('',$,#44072);
#43936=PRODUCT_DEFINITION_FORMATION('',$,#44073);
#43937=PRODUCT_DEFINITION_FORMATION('',$,#44074);
#43938=PRODUCT_DEFINITION_FORMATION('',$,#44075);
#43939=PRODUCT_DEFINITION_FORMATION('',$,#44076);
#43940=PRODUCT_DEFINITION_FORMATION('',$,#44077);
#43941=PRODUCT_DEFINITION_FORMATION('',$,#44078);
#43942=PRODUCT_DEFINITION_FORMATION('',$,#44079);
#43943=PRODUCT_DEFINITION_FORMATION('',$,#44080);
#43944=PRODUCT_DEFINITION_FORMATION('',$,#44081);
#43945=PRODUCT_DEFINITION_FORMATION('',$,#44082);
#43946=PRODUCT_DEFINITION_FORMATION('',$,#44083);
#43947=PRODUCT_DEFINITION_FORMATION('',$,#44084);
#43948=PRODUCT_DEFINITION_FORMATION('',$,#44085);
#43949=PRODUCT_DEFINITION_FORMATION('',$,#44086);
#43950=PRODUCT_DEFINITION_FORMATION('',$,#44087);
#43951=PRODUCT_DEFINITION_FORMATION('',$,#44088);
#43952=PRODUCT_DEFINITION_FORMATION('',$,#44089);
#43953=PRODUCT_DEFINITION_FORMATION('',$,#44090);
#43954=PRODUCT_DEFINITION_FORMATION('',$,#44091);
#43955=PRODUCT_DEFINITION_FORMATION('',$,#44092);
#43956=PRODUCT_DEFINITION_FORMATION('',$,#44093);
#43957=PRODUCT_DEFINITION_FORMATION('',$,#44094);
#43958=PRODUCT_DEFINITION_FORMATION('',$,#44095);
#43959=PRODUCT_DEFINITION_FORMATION('',$,#44096);
#43960=PRODUCT_DEFINITION_FORMATION('',$,#44097);
#43961=PRODUCT_DEFINITION_FORMATION('',$,#44098);
#43962=PRODUCT_DEFINITION_FORMATION('',$,#44099);
#43963=PRODUCT_DEFINITION_FORMATION('',$,#44100);
#43964=PRODUCT_DEFINITION_FORMATION('',$,#44101);
#43965=PRODUCT_DEFINITION_FORMATION('',$,#44102);
#43966=PRODUCT_DEFINITION_FORMATION('',$,#44103);
#43967=PRODUCT_DEFINITION_FORMATION('',$,#44104);
#43968=PRODUCT_DEFINITION_FORMATION('',$,#44105);
#43969=PRODUCT_DEFINITION_FORMATION('',$,#44106);
#43970=PRODUCT_DEFINITION_FORMATION('',$,#44107);
#43971=PRODUCT_DEFINITION_FORMATION('',$,#44108);
#43972=PRODUCT_DEFINITION_FORMATION('',$,#44109);
#43973=PRODUCT_DEFINITION_FORMATION('',$,#44110);
#43974=PRODUCT_DEFINITION_FORMATION('',$,#44111);
#43975=PRODUCT_DEFINITION_FORMATION('',$,#44112);
#43976=PRODUCT_DEFINITION_FORMATION('',$,#44113);
#43977=PRODUCT_DEFINITION_FORMATION('',$,#44114);
#43978=PRODUCT_DEFINITION_FORMATION('',$,#44115);
#43979=PRODUCT_DEFINITION_FORMATION('',$,#44116);
#43980=PRODUCT_DEFINITION_FORMATION('',$,#44117);
#43981=PRODUCT_DEFINITION_FORMATION('',$,#44118);
#43982=PRODUCT_DEFINITION_FORMATION('',$,#44119);
#43983=PRODUCT_DEFINITION_FORMATION('',$,#44120);
#43984=PRODUCT_DEFINITION_FORMATION('',$,#44121);
#43985=PRODUCT_DEFINITION_FORMATION('',$,#44122);
#43986=PRODUCT_DEFINITION_FORMATION('',$,#44123);
#43987=PRODUCT_DEFINITION_FORMATION('',$,#44124);
#43988=PRODUCT_DEFINITION_FORMATION('',$,#44125);
#43989=PRODUCT_DEFINITION_FORMATION('',$,#44126);
#43990=PRODUCT_DEFINITION_FORMATION('',$,#44127);
#43991=PRODUCT_DEFINITION_FORMATION('',$,#44128);
#43992=PRODUCT_DEFINITION_FORMATION('',$,#44129);
#43993=PRODUCT_DEFINITION_FORMATION('',$,#44130);
#43994=PRODUCT_DEFINITION_FORMATION('',$,#44131);
#43995=PRODUCT_DEFINITION_FORMATION('',$,#44132);
#43996=PRODUCT_RELATED_PRODUCT_CATEGORY('PAT-098','PAT-098',(#44066));
#43997=PRODUCT_RELATED_PRODUCT_CATEGORY(
'Guide frame and screw bearings','Guide frame and screw bearings',(#44067));
#43998=PRODUCT_RELATED_PRODUCT_CATEGORY('Base','Base',(#44068));
#43999=PRODUCT_RELATED_PRODUCT_CATEGORY('Foot strip','Foot strip',(#44069));
#44000=PRODUCT_RELATED_PRODUCT_CATEGORY('Foot strip (1)',
'Foot strip (1)',(#44070));
#44001=PRODUCT_RELATED_PRODUCT_CATEGORY('Top guide plate',
'Top guide plate',(#44071));
#44002=PRODUCT_RELATED_PRODUCT_CATEGORY('Frame upright','Frame upright',
(#44072));
#44003=PRODUCT_RELATED_PRODUCT_CATEGORY('Frame upright (1)',
'Frame upright (1)',(#44073));
#44004=PRODUCT_RELATED_PRODUCT_CATEGORY('Lower guide bracket',
'Lower guide bracket',(#44074));
#44005=PRODUCT_RELATED_PRODUCT_CATEGORY('Upper guide bracket',
'Upper guide bracket',(#44075));
#44006=PRODUCT_RELATED_PRODUCT_CATEGORY('Lower guide bracket (1)',
'Lower guide bracket (1)',(#44076));
#44007=PRODUCT_RELATED_PRODUCT_CATEGORY('Upper guide bracket (1)',
'Upper guide bracket (1)',(#44077));
#44008=PRODUCT_RELATED_PRODUCT_CATEGORY('Floating bearing pedestal',
'Floating bearing pedestal',(#44078));
#44009=PRODUCT_RELATED_PRODUCT_CATEGORY('Fixed bearing crossbar',
'Fixed bearing crossbar',(#44079));
#44010=PRODUCT_RELATED_PRODUCT_CATEGORY('Floating bearing cap',
'Floating bearing cap',(#44080));
#44011=PRODUCT_RELATED_PRODUCT_CATEGORY('Fixed bearing cap',
'Fixed bearing cap',(#44081));
#44012=PRODUCT_RELATED_PRODUCT_CATEGORY('Lower travel stop',
'Lower travel stop',(#44082));
#44013=PRODUCT_RELATED_PRODUCT_CATEGORY('Upper travel stop',
'Upper travel stop',(#44083));
#44014=PRODUCT_RELATED_PRODUCT_CATEGORY('Lower travel stop (1)',
'Lower travel stop (1)',(#44084));
#44015=PRODUCT_RELATED_PRODUCT_CATEGORY('Upper travel stop (1)',
'Upper travel stop (1)',(#44085));
#44016=PRODUCT_RELATED_PRODUCT_CATEGORY('Lower compression platen',
'Lower compression platen',(#44086));
#44017=PRODUCT_RELATED_PRODUCT_CATEGORY('Graduated scale',
'Graduated scale',(#44087));
#44018=PRODUCT_RELATED_PRODUCT_CATEGORY(
'Precision Shaft - 12 mm Diameter, 300 mm Long',
'Precision Shaft - 12 mm Diameter, 300 mm Long',(#44088));
#44019=PRODUCT_RELATED_PRODUCT_CATEGORY('Shaft Support - 12 mm Bore',
'Shaft Support - 12 mm Bore',(#44089));
#44020=PRODUCT_RELATED_PRODUCT_CATEGORY('M5x14 Cap Screw',
'M5x14 Cap Screw',(#44090));
#44021=PRODUCT_RELATED_PRODUCT_CATEGORY(
'Sealed Ball Bearing - 12 x 32 x 10 mm',
'Sealed Ball Bearing - 12 x 32 x 10 mm',(#44091));
#44022=PRODUCT_RELATED_PRODUCT_CATEGORY('Inner ring','Inner ring',(#44092));
#44023=PRODUCT_RELATED_PRODUCT_CATEGORY('Outer ring','Outer ring',(#44093));
#44024=PRODUCT_RELATED_PRODUCT_CATEGORY('Balls','Balls',(#44094));
#44025=PRODUCT_RELATED_PRODUCT_CATEGORY('Cage','Cage',(#44095));
#44026=PRODUCT_RELATED_PRODUCT_CATEGORY('Seals 2RS','Seals 2RS',(#44096));
#44027=PRODUCT_RELATED_PRODUCT_CATEGORY(
'Sealed Ball Bearing - 20 x 47 x 14 mm',
'Sealed Ball Bearing - 20 x 47 x 14 mm',(#44097));
#44028=PRODUCT_RELATED_PRODUCT_CATEGORY('Inner ring (1)',
'Inner ring (1)',(#44098));
#44029=PRODUCT_RELATED_PRODUCT_CATEGORY('Outer ring (1)',
'Outer ring (1)',(#44099));
#44030=PRODUCT_RELATED_PRODUCT_CATEGORY('Balls (1)','Balls (1)',(#44100));
#44031=PRODUCT_RELATED_PRODUCT_CATEGORY('Cage (1)','Cage (1)',(#44101));
#44032=PRODUCT_RELATED_PRODUCT_CATEGORY('Seals 2RS (1)','Seals 2RS (1)',
(#44102));
#44033=PRODUCT_RELATED_PRODUCT_CATEGORY('M5x25 stop screw',
'M5x25 stop screw',(#44103));
#44034=PRODUCT_RELATED_PRODUCT_CATEGORY('M4x10 Cap Screw',
'M4x10 Cap Screw',(#44104));
#44035=PRODUCT_RELATED_PRODUCT_CATEGORY(
'Slotted Extrusion - 20 x 20 x 400 mm',
'Slotted Extrusion - 20 x 20 x 400 mm',(#44105));
#44036=PRODUCT_RELATED_PRODUCT_CATEGORY('Cap Screw - M5x20',
'Cap Screw - M5x20',(#44106));
#44037=PRODUCT_RELATED_PRODUCT_CATEGORY('Captive slot nut',
'Captive slot nut',(#44107));
#44038=PRODUCT_RELATED_PRODUCT_CATEGORY('M5x8 ruler screw',
'M5x8 ruler screw',(#44108));
#44039=PRODUCT_RELATED_PRODUCT_CATEGORY('Platform and lead nut',
'Platform and lead nut',(#44109));
#44040=PRODUCT_RELATED_PRODUCT_CATEGORY('Platform','Platform',(#44110));
#44041=PRODUCT_RELATED_PRODUCT_CATEGORY('Linear bushing housing',
'Linear bushing housing',(#44111));
#44042=PRODUCT_RELATED_PRODUCT_CATEGORY('Linear bushing housing (1)',
'Linear bushing housing (1)',(#44112));
#44043=PRODUCT_RELATED_PRODUCT_CATEGORY('Nut carrier','Nut carrier',(#44113));
#44044=PRODUCT_RELATED_PRODUCT_CATEGORY('Upper compression platen',
'Upper compression platen',(#44114));
#44045=PRODUCT_RELATED_PRODUCT_CATEGORY('Scale pointer','Scale pointer',
(#44115));
#44046=PRODUCT_RELATED_PRODUCT_CATEGORY(
'Linear Ball Bushing - 12 x 21 x 30 mm',
'Linear Ball Bushing - 12 x 21 x 30 mm',(#44116));
#44047=PRODUCT_RELATED_PRODUCT_CATEGORY('Steel sleeve','Steel sleeve',(#44117));
#44048=PRODUCT_RELATED_PRODUCT_CATEGORY('Ball retainer (plastic)',
'Ball retainer (plastic)',(#44118));
#44049=PRODUCT_RELATED_PRODUCT_CATEGORY('Flanged lead nut',
'Flanged lead nut',(#44119));
#44050=PRODUCT_RELATED_PRODUCT_CATEGORY('M4x30 nut screw',
'M4x30 nut screw',(#44120));
#44051=PRODUCT_RELATED_PRODUCT_CATEGORY('Cap Screw - M4x16',
'Cap Screw - M4x16',(#44121));
#44052=PRODUCT_RELATED_PRODUCT_CATEGORY('Vertical screw and handwheel',
'Vertical screw and handwheel',(#44122));
#44053=PRODUCT_RELATED_PRODUCT_CATEGORY('Supported TR12x3 screw',
'Supported TR12x3 screw',(#44123));
#44054=PRODUCT_RELATED_PRODUCT_CATEGORY('Inner race spacer',
'Inner race spacer',(#44124));
#44055=PRODUCT_RELATED_PRODUCT_CATEGORY('Shaft retaining collar',
'Shaft retaining collar',(#44125));
#44056=PRODUCT_RELATED_PRODUCT_CATEGORY('Handwheel','Handwheel',(#44126));
#44057=PRODUCT_RELATED_PRODUCT_CATEGORY('Handle pivot sleeve',
'Handle pivot sleeve',(#44127));
#44058=PRODUCT_RELATED_PRODUCT_CATEGORY('Revolving handle',
'Revolving handle',(#44128));
#44059=PRODUCT_RELATED_PRODUCT_CATEGORY('Key 6x6x20','Key 6x6x20',(#44129));
#44060=PRODUCT_RELATED_PRODUCT_CATEGORY('Socket Set Screw - M5x8',
'Socket Set Screw - M5x8',(#44130));
#44061=PRODUCT_RELATED_PRODUCT_CATEGORY('Flat Washer - M6',
'Flat Washer - M6',(#44131));
#44062=PRODUCT_RELATED_PRODUCT_CATEGORY('Cap Screw - M6x25',
'Cap Screw - M6x25',(#44132));
#44063=APPLICATION_PROTOCOL_DEFINITION('international standard',
'automotive_design',2009,#44064);
#44064=APPLICATION_CONTEXT(
'Core Data for Automotive Mechanical Design Process');
#44065=PRODUCT_CONTEXT('part definition',#44064,'mechanical');
#44066=PRODUCT('PAT-098','PAT-098',
'PAT-098',(#44065));
#44067=PRODUCT('Guide frame and screw bearings',
'Guide frame and screw bearings','Guide frame and screw bearings',(#44065));
#44068=PRODUCT('Base','Base','Base',(#44065));
#44069=PRODUCT('Foot strip','Foot strip','Foot strip',(#44065));
#44070=PRODUCT('Foot strip (1)','Foot strip (1)','Foot strip (1)',(#44065));
#44071=PRODUCT('Top guide plate','Top guide plate','Top guide plate',(#44065));
#44072=PRODUCT('Frame upright','Frame upright','Frame upright',(#44065));
#44073=PRODUCT('Frame upright (1)','Frame upright (1)','Frame upright (1)',(#44065));
#44074=PRODUCT('Lower guide bracket','Lower guide bracket',
'Lower guide bracket',(#44065));
#44075=PRODUCT('Upper guide bracket','Upper guide bracket',
'Upper guide bracket',(#44065));
#44076=PRODUCT('Lower guide bracket (1)','Lower guide bracket (1)',
'Lower guide bracket (1)',(#44065));
#44077=PRODUCT('Upper guide bracket (1)','Upper guide bracket (1)',
'Upper guide bracket (1)',(#44065));
#44078=PRODUCT('Floating bearing pedestal','Floating bearing pedestal',
'Floating bearing pedestal',(#44065));
#44079=PRODUCT('Fixed bearing crossbar','Fixed bearing crossbar',
'Fixed bearing crossbar',(#44065));
#44080=PRODUCT('Floating bearing cap','Floating bearing cap',
'Floating bearing cap',(#44065));
#44081=PRODUCT('Fixed bearing cap','Fixed bearing cap',
'Fixed bearing cap',(#44065));
#44082=PRODUCT('Lower travel stop','Lower travel stop',
'Lower travel stop',(#44065));
#44083=PRODUCT('Upper travel stop','Upper travel stop',
'Upper travel stop',(#44065));
#44084=PRODUCT('Lower travel stop (1)','Lower travel stop (1)',
'Lower travel stop (1)',(#44065));
#44085=PRODUCT('Upper travel stop (1)','Upper travel stop (1)',
'Upper travel stop (1)',(#44065));
#44086=PRODUCT('Lower compression platen','Lower compression platen',
'Lower compression platen',(#44065));
#44087=PRODUCT('Graduated scale','Graduated scale','Graduated scale',(#44065));
#44088=PRODUCT('Precision Shaft - 12 mm Diameter, 300 mm Long',
'Precision Shaft - 12 mm Diameter, 300 mm Long',
'Precision Shaft - 12 mm Diameter, 300 mm Long',(#44065));
#44089=PRODUCT('Shaft Support - 12 mm Bore',
'Shaft Support - 12 mm Bore','Shaft Support - 12 mm Bore',(#44065));
#44090=PRODUCT('M5x14 Cap Screw','M5x14 Cap Screw','M5x14 Cap Screw',(#44065));
#44091=PRODUCT('Sealed Ball Bearing - 12 x 32 x 10 mm',
'Sealed Ball Bearing - 12 x 32 x 10 mm',
'Sealed Ball Bearing - 12 x 32 x 10 mm',(#44065));
#44092=PRODUCT('Inner ring','Inner ring','Inner ring',(#44065));
#44093=PRODUCT('Outer ring','Outer ring','Outer ring',(#44065));
#44094=PRODUCT('Balls','Balls','Balls',(#44065));
#44095=PRODUCT('Cage','Cage','Cage',(#44065));
#44096=PRODUCT('Seals 2RS','Seals 2RS','Seals 2RS',(#44065));
#44097=PRODUCT('Sealed Ball Bearing - 20 x 47 x 14 mm',
'Sealed Ball Bearing - 20 x 47 x 14 mm',
'Sealed Ball Bearing - 20 x 47 x 14 mm',(#44065));
#44098=PRODUCT('Inner ring (1)','Inner ring (1)','Inner ring (1)',(#44065));
#44099=PRODUCT('Outer ring (1)','Outer ring (1)','Outer ring (1)',(#44065));
#44100=PRODUCT('Balls (1)','Balls (1)','Balls (1)',(#44065));
#44101=PRODUCT('Cage (1)','Cage (1)','Cage (1)',(#44065));
#44102=PRODUCT('Seals 2RS (1)','Seals 2RS (1)','Seals 2RS (1)',(#44065));
#44103=PRODUCT('M5x25 stop screw','M5x25 stop screw','M5x25 stop screw',
(#44065));
#44104=PRODUCT('M4x10 Cap Screw','M4x10 Cap Screw','M4x10 Cap Screw',(#44065));
#44105=PRODUCT('Slotted Extrusion - 20 x 20 x 400 mm',
'Slotted Extrusion - 20 x 20 x 400 mm',
'Slotted Extrusion - 20 x 20 x 400 mm',(#44065));
#44106=PRODUCT('Cap Screw - M5x20','Cap Screw - M5x20',
'Cap Screw - M5x20',(#44065));
#44107=PRODUCT('Captive slot nut','Captive slot nut','Captive slot nut',
(#44065));
#44108=PRODUCT('M5x8 ruler screw','M5x8 ruler screw','M5x8 ruler screw',
(#44065));
#44109=PRODUCT('Platform and lead nut','Platform and lead nut',
'Platform and lead nut',(#44065));
#44110=PRODUCT('Platform','Platform','Platform',(#44065));
#44111=PRODUCT('Linear bushing housing','Linear bushing housing',
'Linear bushing housing',(#44065));
#44112=PRODUCT('Linear bushing housing (1)','Linear bushing housing (1)',
'Linear bushing housing (1)',(#44065));
#44113=PRODUCT('Nut carrier','Nut carrier','Nut carrier',(#44065));
#44114=PRODUCT('Upper compression platen','Upper compression platen',
'Upper compression platen',(#44065));
#44115=PRODUCT('Scale pointer','Scale pointer','Scale pointer',(#44065));
#44116=PRODUCT('Linear Ball Bushing - 12 x 21 x 30 mm',
'Linear Ball Bushing - 12 x 21 x 30 mm',
'Linear Ball Bushing - 12 x 21 x 30 mm',(#44065));
#44117=PRODUCT('Steel sleeve','Steel sleeve','Steel sleeve',(#44065));
#44118=PRODUCT('Ball retainer (plastic)','Ball retainer (plastic)',
'Ball retainer (plastic)',(#44065));
#44119=PRODUCT('Flanged lead nut','Flanged lead nut','Flanged lead nut',
(#44065));
#44120=PRODUCT('M4x30 nut screw','M4x30 nut screw','M4x30 nut screw',(#44065));
#44121=PRODUCT('Cap Screw - M4x16','Cap Screw - M4x16',
'Cap Screw - M4x16',(#44065));
#44122=PRODUCT('Vertical screw and handwheel',
'Vertical screw and handwheel','Vertical screw and handwheel',(#44065));
#44123=PRODUCT('Supported TR12x3 screw','Supported TR12x3 screw',
'Supported TR12x3 screw',(#44065));
#44124=PRODUCT('Inner race spacer','Inner race spacer',
'Inner race spacer',(#44065));
#44125=PRODUCT('Shaft retaining collar','Shaft retaining collar',
'Shaft retaining collar',(#44065));
#44126=PRODUCT('Handwheel','Handwheel','Handwheel',(#44065));
#44127=PRODUCT('Handle pivot sleeve','Handle pivot sleeve',
'Handle pivot sleeve',(#44065));
#44128=PRODUCT('Revolving handle','Revolving handle','Revolving handle',
(#44065));
#44129=PRODUCT('Key 6x6x20','Key 6x6x20','Key 6x6x20',(#44065));
#44130=PRODUCT('Socket Set Screw - M5x8','Socket Set Screw - M5x8',
'Socket Set Screw - M5x8',(#44065));
#44131=PRODUCT('Flat Washer - M6','Flat Washer - M6','Flat Washer - M6',
(#44065));
#44132=PRODUCT('Cap Screw - M6x25','Cap Screw - M6x25',
'Cap Screw - M6x25',(#44065));
#44133=PRESENTATION_STYLE_ASSIGNMENT((#44139));
#44134=PRESENTATION_STYLE_ASSIGNMENT((#44140));
#44135=PRESENTATION_STYLE_ASSIGNMENT((#44141));
#44136=PRESENTATION_STYLE_ASSIGNMENT((#44142));
#44137=PRESENTATION_STYLE_ASSIGNMENT((#44143));
#44138=PRESENTATION_STYLE_ASSIGNMENT((#44144));
#44139=SURFACE_STYLE_USAGE(.BOTH.,#44145);
#44140=SURFACE_STYLE_USAGE(.BOTH.,#44146);
#44141=SURFACE_STYLE_USAGE(.BOTH.,#44147);
#44142=SURFACE_STYLE_USAGE(.BOTH.,#44148);
#44143=SURFACE_STYLE_USAGE(.BOTH.,#44149);
#44144=SURFACE_STYLE_USAGE(.BOTH.,#44150);
#44145=SURFACE_SIDE_STYLE('',(#44151));
#44146=SURFACE_SIDE_STYLE('',(#44152));
#44147=SURFACE_SIDE_STYLE('',(#44153));
#44148=SURFACE_SIDE_STYLE('',(#44154));
#44149=SURFACE_SIDE_STYLE('',(#44155));
#44150=SURFACE_SIDE_STYLE('',(#44156));
#44151=SURFACE_STYLE_FILL_AREA(#44157);
#44152=SURFACE_STYLE_FILL_AREA(#44158);
#44153=SURFACE_STYLE_FILL_AREA(#44159);
#44154=SURFACE_STYLE_FILL_AREA(#44160);
#44155=SURFACE_STYLE_FILL_AREA(#44161);
#44156=SURFACE_STYLE_FILL_AREA(#44162);
#44157=FILL_AREA_STYLE('Steel - Satin',(#44163));
#44158=FILL_AREA_STYLE('CAD Library Painted - Deep blue',(#44164));
#44159=FILL_AREA_STYLE('CAD Library Painted - Engineering blue',(#44165));
#44160=FILL_AREA_STYLE('CAD Library Painted - Steel gray',(#44166));
#44161=FILL_AREA_STYLE('CAD Library Painted - Graphite',(#44167));
#44162=FILL_AREA_STYLE('CAD Library Painted - Light blue',(#44168));
#44163=FILL_AREA_STYLE_COLOUR('Steel - Satin',#44169);
#44164=FILL_AREA_STYLE_COLOUR('CAD Library Painted - Deep blue',#44170);
#44165=FILL_AREA_STYLE_COLOUR('CAD Library Painted - Engineering blue',
#44171);
#44166=FILL_AREA_STYLE_COLOUR('CAD Library Painted - Steel gray',#44172);
#44167=FILL_AREA_STYLE_COLOUR('CAD Library Painted - Graphite',#44173);
#44168=FILL_AREA_STYLE_COLOUR('CAD Library Painted - Light blue',#44174);
#44169=COLOUR_RGB('Steel - Satin',0.627450980392157,0.627450980392157,0.627450980392157);
#44170=COLOUR_RGB('CAD Library Painted - Deep blue',0.0784313725490196,
0.203921568627451,0.349019607843137);
#44171=COLOUR_RGB('CAD Library Painted - Engineering blue',0.12156862745098,
0.356862745098039,0.6);
#44172=COLOUR_RGB('CAD Library Painted - Steel gray',0.592156862745098,
0.631372549019608,0.67843137254902);
#44173=COLOUR_RGB('CAD Library Painted - Graphite',0.168627450980392,0.192156862745098,
0.231372549019608);
#44174=COLOUR_RGB('CAD Library Painted - Light blue',0.286274509803922,
0.552941176470588,0.780392156862745);
#44175=COLOUR_RGB('Dark Blue',0.08,0.2,0.34);
#44176=FILL_AREA_STYLE_COLOUR('',#44175);
#44177=FILL_AREA_STYLE('',(#44176));
#44178=SURFACE_STYLE_FILL_AREA(#44177);
#44179=SURFACE_SIDE_STYLE('',(#44178));
#44180=SURFACE_STYLE_USAGE(.BOTH.,#44179);
#44181=PRESENTATION_STYLE_ASSIGNMENT((#44180));
#44182=COLOUR_RGB('Light Blue',0.38,0.62,0.78);
#44183=FILL_AREA_STYLE_COLOUR('',#44182);
#44184=FILL_AREA_STYLE('',(#44183));
#44185=SURFACE_STYLE_FILL_AREA(#44184);
#44186=SURFACE_SIDE_STYLE('',(#44185));
#44187=SURFACE_STYLE_USAGE(.BOTH.,#44186);
#44188=PRESENTATION_STYLE_ASSIGNMENT((#44187));
#44189=COLOUR_RGB('Sky Blue',0.24,0.69,0.87);
#44190=FILL_AREA_STYLE_COLOUR('',#44189);
#44191=FILL_AREA_STYLE('',(#44190));
#44192=SURFACE_STYLE_FILL_AREA(#44191);
#44193=SURFACE_SIDE_STYLE('',(#44192));
#44194=SURFACE_STYLE_USAGE(.BOTH.,#44193);
#44195=PRESENTATION_STYLE_ASSIGNMENT((#44194));
#44196=COLOUR_RGB('Grey',0.48,0.52,0.57);
#44197=FILL_AREA_STYLE_COLOUR('',#44196);
#44198=FILL_AREA_STYLE('',(#44197));
#44199=SURFACE_STYLE_FILL_AREA(#44198);
#44200=SURFACE_SIDE_STYLE('',(#44199));
#44201=SURFACE_STYLE_USAGE(.BOTH.,#44200);
#44202=PRESENTATION_STYLE_ASSIGNMENT((#44201));
#44203=COLOUR_RGB('Black',0.12,0.14,0.17);
#44204=FILL_AREA_STYLE_COLOUR('',#44203);
#44205=FILL_AREA_STYLE('',(#44204));
#44206=SURFACE_STYLE_FILL_AREA(#44205);
#44207=SURFACE_SIDE_STYLE('',(#44206));
#44208=SURFACE_STYLE_USAGE(.BOTH.,#44207);
#44209=PRESENTATION_STYLE_ASSIGNMENT((#44208));
#44210=COLOUR_RGB('Off White',0.89,0.88,0.83);
#44211=FILL_AREA_STYLE_COLOUR('',#44210);
#44212=FILL_AREA_STYLE('',(#44211));
#44213=SURFACE_STYLE_FILL_AREA(#44212);
#44214=SURFACE_SIDE_STYLE('',(#44213));
#44215=SURFACE_STYLE_USAGE(.BOTH.,#44214);
#44216=PRESENTATION_STYLE_ASSIGNMENT((#44215));
ENDSEC;
END-ISO-10303-21;
